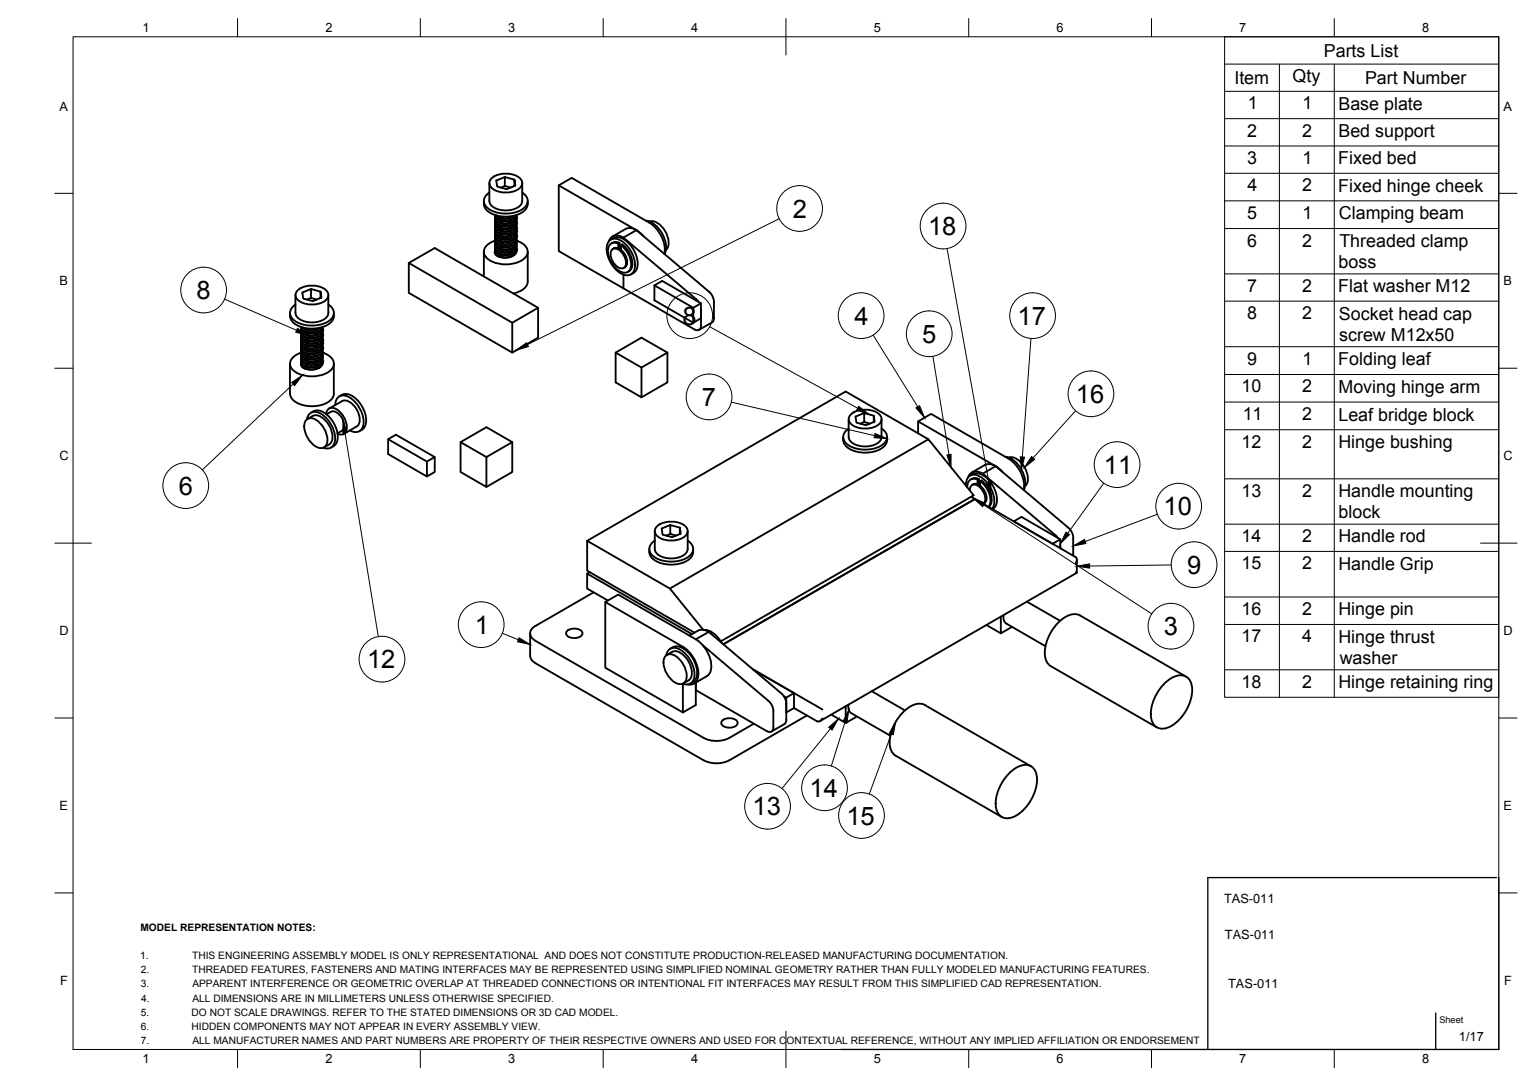
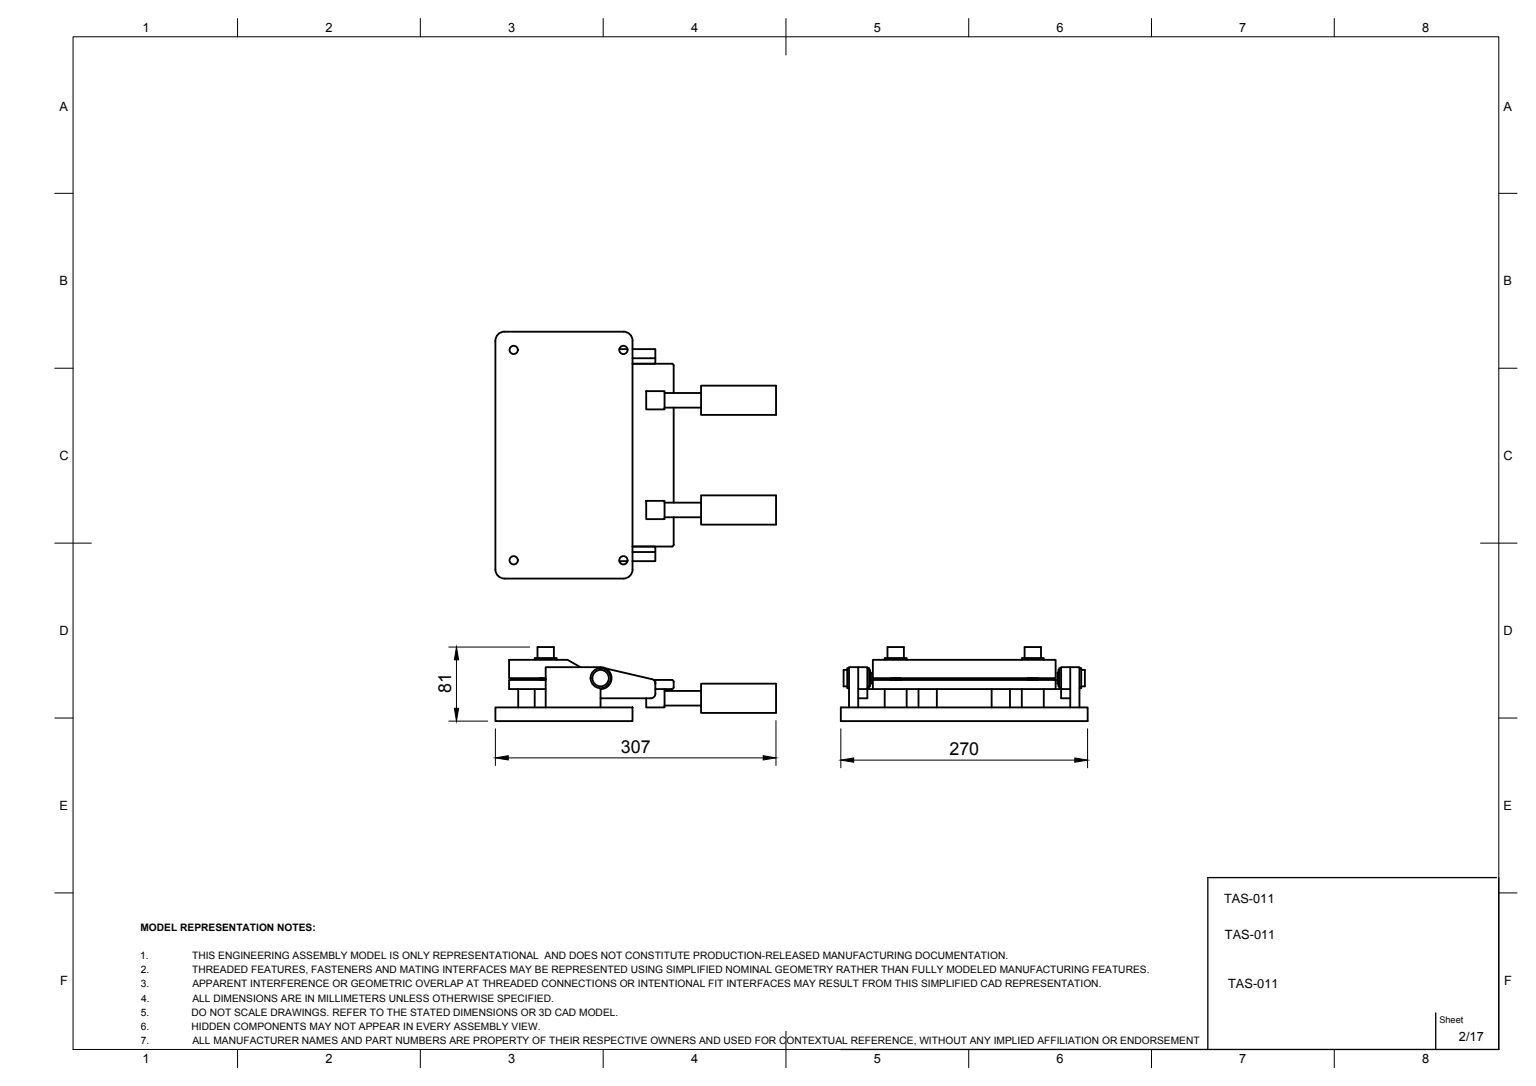
ISO-10303-21;
HEADER;
/* Generated by software containing ST-Developer
 * from STEP Tools, Inc. (www.steptools.com) 
 */

FILE_DESCRIPTION(
/* description */ (
'Independent manual bench leaf bending machine,200mm work width. Fabri
cated welded frame and folding leaf, repeated bushed and fully retaine
d hinge hardware, two handles with bonded grips, beveled clamping beam
 and modeledM12 clamp screws.2mm omitted-workpiece assembly reference 
gap, not a capacity claim. Native135deg hinge travel. Weld sizing, pro
duction fits, material condition, bending capacity, strength and life 
unassigned.'),
/* implementation_level */ '2;1');

FILE_NAME(
/* name */ 'TAS-011.step',
/* time_stamp */ '2026-11-14T09:11:34-08:00',
/* author */ (''),
/* organization */ (''),
/* preprocessor_version */ 'ST-DEVELOPER v20.2',
/* originating_system */ 'Autodesk Translation Framework v15.17.0.0',
/* authorisation */ '');

FILE_SCHEMA (('AUTOMOTIVE_DESIGN { 1 0 10303 214 3 1 1 }'));
ENDSEC;

DATA;
#10=MECHANICAL_DESIGN_GEOMETRIC_PRESENTATION_REPRESENTATION('',(#446,#447,
#448,#449,#450,#451,#452,#453,#454,#455,#456,#457,#458,#459,#460,#461,#462,
#463),#37701);
#11=ITEM_DEFINED_TRANSFORMATION($,$,#4362,#4673);
#12=ITEM_DEFINED_TRANSFORMATION($,$,#4434,#4674);
#13=ITEM_DEFINED_TRANSFORMATION($,$,#4393,#4675);
#14=ITEM_DEFINED_TRANSFORMATION($,$,#4441,#4676);
#15=ITEM_DEFINED_TRANSFORMATION($,$,#4406,#4677);
#16=ITEM_DEFINED_TRANSFORMATION($,$,#4454,#4678);
#17=ITEM_DEFINED_TRANSFORMATION($,$,#4488,#4679);
#18=ITEM_DEFINED_TRANSFORMATION($,$,#4497,#4680);
#19=ITEM_DEFINED_TRANSFORMATION($,$,#4419,#4681);
#20=ITEM_DEFINED_TRANSFORMATION($,$,#4577,#4682);
#21=ITEM_DEFINED_TRANSFORMATION($,$,#4596,#4683);
#22=ITEM_DEFINED_TRANSFORMATION($,$,#4603,#4684);
#23=ITEM_DEFINED_TRANSFORMATION($,$,#4612,#4685);
#24=ITEM_DEFINED_TRANSFORMATION($,$,#4619,#4686);
#25=ITEM_DEFINED_TRANSFORMATION($,$,#4625,#4687);
#26=ITEM_DEFINED_TRANSFORMATION($,$,#4635,#4688);
#27=ITEM_DEFINED_TRANSFORMATION($,$,#4653,#4689);
#28=ITEM_DEFINED_TRANSFORMATION($,$,#4662,#4690);
#29=ITEM_DEFINED_TRANSFORMATION($,$,#4434,#4691);
#30=ITEM_DEFINED_TRANSFORMATION($,$,#4441,#4692);
#31=ITEM_DEFINED_TRANSFORMATION($,$,#4454,#4693);
#32=ITEM_DEFINED_TRANSFORMATION($,$,#4488,#4694);
#33=ITEM_DEFINED_TRANSFORMATION($,$,#4497,#4695);
#34=ITEM_DEFINED_TRANSFORMATION($,$,#4577,#4696);
#35=ITEM_DEFINED_TRANSFORMATION($,$,#4596,#4697);
#36=ITEM_DEFINED_TRANSFORMATION($,$,#4603,#4698);
#37=ITEM_DEFINED_TRANSFORMATION($,$,#4612,#4699);
#38=ITEM_DEFINED_TRANSFORMATION($,$,#4619,#4700);
#39=ITEM_DEFINED_TRANSFORMATION($,$,#4625,#4701);
#40=ITEM_DEFINED_TRANSFORMATION($,$,#4653,#4702);
#41=ITEM_DEFINED_TRANSFORMATION($,$,#4635,#4703);
#42=ITEM_DEFINED_TRANSFORMATION($,$,#4653,#4704);
#43=ITEM_DEFINED_TRANSFORMATION($,$,#4653,#4705);
#44=ITEM_DEFINED_TRANSFORMATION($,$,#4662,#4706);
#45=(
REPRESENTATION_RELATIONSHIP($,$,#37779,#37778)
REPRESENTATION_RELATIONSHIP_WITH_TRANSFORMATION(#11)
SHAPE_REPRESENTATION_RELATIONSHIP()
);
#46=(
REPRESENTATION_RELATIONSHIP($,$,#37783,#37778)
REPRESENTATION_RELATIONSHIP_WITH_TRANSFORMATION(#12)
SHAPE_REPRESENTATION_RELATIONSHIP()
);
#47=(
REPRESENTATION_RELATIONSHIP($,$,#37780,#37778)
REPRESENTATION_RELATIONSHIP_WITH_TRANSFORMATION(#13)
SHAPE_REPRESENTATION_RELATIONSHIP()
);
#48=(
REPRESENTATION_RELATIONSHIP($,$,#37784,#37778)
REPRESENTATION_RELATIONSHIP_WITH_TRANSFORMATION(#14)
SHAPE_REPRESENTATION_RELATIONSHIP()
);
#49=(
REPRESENTATION_RELATIONSHIP($,$,#37781,#37778)
REPRESENTATION_RELATIONSHIP_WITH_TRANSFORMATION(#15)
SHAPE_REPRESENTATION_RELATIONSHIP()
);
#50=(
REPRESENTATION_RELATIONSHIP($,$,#37785,#37778)
REPRESENTATION_RELATIONSHIP_WITH_TRANSFORMATION(#16)
SHAPE_REPRESENTATION_RELATIONSHIP()
);
#51=(
REPRESENTATION_RELATIONSHIP($,$,#37786,#37778)
REPRESENTATION_RELATIONSHIP_WITH_TRANSFORMATION(#17)
SHAPE_REPRESENTATION_RELATIONSHIP()
);
#52=(
REPRESENTATION_RELATIONSHIP($,$,#37787,#37778)
REPRESENTATION_RELATIONSHIP_WITH_TRANSFORMATION(#18)
SHAPE_REPRESENTATION_RELATIONSHIP()
);
#53=(
REPRESENTATION_RELATIONSHIP($,$,#37782,#37778)
REPRESENTATION_RELATIONSHIP_WITH_TRANSFORMATION(#19)
SHAPE_REPRESENTATION_RELATIONSHIP()
);
#54=(
REPRESENTATION_RELATIONSHIP($,$,#37788,#37778)
REPRESENTATION_RELATIONSHIP_WITH_TRANSFORMATION(#20)
SHAPE_REPRESENTATION_RELATIONSHIP()
);
#55=(
REPRESENTATION_RELATIONSHIP($,$,#37789,#37778)
REPRESENTATION_RELATIONSHIP_WITH_TRANSFORMATION(#21)
SHAPE_REPRESENTATION_RELATIONSHIP()
);
#56=(
REPRESENTATION_RELATIONSHIP($,$,#37790,#37778)
REPRESENTATION_RELATIONSHIP_WITH_TRANSFORMATION(#22)
SHAPE_REPRESENTATION_RELATIONSHIP()
);
#57=(
REPRESENTATION_RELATIONSHIP($,$,#37791,#37778)
REPRESENTATION_RELATIONSHIP_WITH_TRANSFORMATION(#23)
SHAPE_REPRESENTATION_RELATIONSHIP()
);
#58=(
REPRESENTATION_RELATIONSHIP($,$,#37792,#37778)
REPRESENTATION_RELATIONSHIP_WITH_TRANSFORMATION(#24)
SHAPE_REPRESENTATION_RELATIONSHIP()
);
#59=(
REPRESENTATION_RELATIONSHIP($,$,#37793,#37778)
REPRESENTATION_RELATIONSHIP_WITH_TRANSFORMATION(#25)
SHAPE_REPRESENTATION_RELATIONSHIP()
);
#60=(
REPRESENTATION_RELATIONSHIP($,$,#37794,#37778)
REPRESENTATION_RELATIONSHIP_WITH_TRANSFORMATION(#26)
SHAPE_REPRESENTATION_RELATIONSHIP()
);
#61=(
REPRESENTATION_RELATIONSHIP($,$,#37795,#37778)
REPRESENTATION_RELATIONSHIP_WITH_TRANSFORMATION(#27)
SHAPE_REPRESENTATION_RELATIONSHIP()
);
#62=(
REPRESENTATION_RELATIONSHIP($,$,#37796,#37778)
REPRESENTATION_RELATIONSHIP_WITH_TRANSFORMATION(#28)
SHAPE_REPRESENTATION_RELATIONSHIP()
);
#63=(
REPRESENTATION_RELATIONSHIP($,$,#37783,#37778)
REPRESENTATION_RELATIONSHIP_WITH_TRANSFORMATION(#29)
SHAPE_REPRESENTATION_RELATIONSHIP()
);
#64=(
REPRESENTATION_RELATIONSHIP($,$,#37784,#37778)
REPRESENTATION_RELATIONSHIP_WITH_TRANSFORMATION(#30)
SHAPE_REPRESENTATION_RELATIONSHIP()
);
#65=(
REPRESENTATION_RELATIONSHIP($,$,#37785,#37778)
REPRESENTATION_RELATIONSHIP_WITH_TRANSFORMATION(#31)
SHAPE_REPRESENTATION_RELATIONSHIP()
);
#66=(
REPRESENTATION_RELATIONSHIP($,$,#37786,#37778)
REPRESENTATION_RELATIONSHIP_WITH_TRANSFORMATION(#32)
SHAPE_REPRESENTATION_RELATIONSHIP()
);
#67=(
REPRESENTATION_RELATIONSHIP($,$,#37787,#37778)
REPRESENTATION_RELATIONSHIP_WITH_TRANSFORMATION(#33)
SHAPE_REPRESENTATION_RELATIONSHIP()
);
#68=(
REPRESENTATION_RELATIONSHIP($,$,#37788,#37778)
REPRESENTATION_RELATIONSHIP_WITH_TRANSFORMATION(#34)
SHAPE_REPRESENTATION_RELATIONSHIP()
);
#69=(
REPRESENTATION_RELATIONSHIP($,$,#37789,#37778)
REPRESENTATION_RELATIONSHIP_WITH_TRANSFORMATION(#35)
SHAPE_REPRESENTATION_RELATIONSHIP()
);
#70=(
REPRESENTATION_RELATIONSHIP($,$,#37790,#37778)
REPRESENTATION_RELATIONSHIP_WITH_TRANSFORMATION(#36)
SHAPE_REPRESENTATION_RELATIONSHIP()
);
#71=(
REPRESENTATION_RELATIONSHIP($,$,#37791,#37778)
REPRESENTATION_RELATIONSHIP_WITH_TRANSFORMATION(#37)
SHAPE_REPRESENTATION_RELATIONSHIP()
);
#72=(
REPRESENTATION_RELATIONSHIP($,$,#37792,#37778)
REPRESENTATION_RELATIONSHIP_WITH_TRANSFORMATION(#38)
SHAPE_REPRESENTATION_RELATIONSHIP()
);
#73=(
REPRESENTATION_RELATIONSHIP($,$,#37793,#37778)
REPRESENTATION_RELATIONSHIP_WITH_TRANSFORMATION(#39)
SHAPE_REPRESENTATION_RELATIONSHIP()
);
#74=(
REPRESENTATION_RELATIONSHIP($,$,#37795,#37778)
REPRESENTATION_RELATIONSHIP_WITH_TRANSFORMATION(#40)
SHAPE_REPRESENTATION_RELATIONSHIP()
);
#75=(
REPRESENTATION_RELATIONSHIP($,$,#37794,#37778)
REPRESENTATION_RELATIONSHIP_WITH_TRANSFORMATION(#41)
SHAPE_REPRESENTATION_RELATIONSHIP()
);
#76=(
REPRESENTATION_RELATIONSHIP($,$,#37795,#37778)
REPRESENTATION_RELATIONSHIP_WITH_TRANSFORMATION(#42)
SHAPE_REPRESENTATION_RELATIONSHIP()
);
#77=(
REPRESENTATION_RELATIONSHIP($,$,#37795,#37778)
REPRESENTATION_RELATIONSHIP_WITH_TRANSFORMATION(#43)
SHAPE_REPRESENTATION_RELATIONSHIP()
);
#78=(
REPRESENTATION_RELATIONSHIP($,$,#37796,#37778)
REPRESENTATION_RELATIONSHIP_WITH_TRANSFORMATION(#44)
SHAPE_REPRESENTATION_RELATIONSHIP()
);
#79=CONTEXT_DEPENDENT_SHAPE_REPRESENTATION(#45,#37744);
#80=CONTEXT_DEPENDENT_SHAPE_REPRESENTATION(#46,#37745);
#81=CONTEXT_DEPENDENT_SHAPE_REPRESENTATION(#47,#37746);
#82=CONTEXT_DEPENDENT_SHAPE_REPRESENTATION(#48,#37747);
#83=CONTEXT_DEPENDENT_SHAPE_REPRESENTATION(#49,#37748);
#84=CONTEXT_DEPENDENT_SHAPE_REPRESENTATION(#50,#37749);
#85=CONTEXT_DEPENDENT_SHAPE_REPRESENTATION(#51,#37750);
#86=CONTEXT_DEPENDENT_SHAPE_REPRESENTATION(#52,#37751);
#87=CONTEXT_DEPENDENT_SHAPE_REPRESENTATION(#53,#37752);
#88=CONTEXT_DEPENDENT_SHAPE_REPRESENTATION(#54,#37753);
#89=CONTEXT_DEPENDENT_SHAPE_REPRESENTATION(#55,#37754);
#90=CONTEXT_DEPENDENT_SHAPE_REPRESENTATION(#56,#37755);
#91=CONTEXT_DEPENDENT_SHAPE_REPRESENTATION(#57,#37756);
#92=CONTEXT_DEPENDENT_SHAPE_REPRESENTATION(#58,#37757);
#93=CONTEXT_DEPENDENT_SHAPE_REPRESENTATION(#59,#37758);
#94=CONTEXT_DEPENDENT_SHAPE_REPRESENTATION(#60,#37759);
#95=CONTEXT_DEPENDENT_SHAPE_REPRESENTATION(#61,#37760);
#96=CONTEXT_DEPENDENT_SHAPE_REPRESENTATION(#62,#37761);
#97=CONTEXT_DEPENDENT_SHAPE_REPRESENTATION(#63,#37762);
#98=CONTEXT_DEPENDENT_SHAPE_REPRESENTATION(#64,#37763);
#99=CONTEXT_DEPENDENT_SHAPE_REPRESENTATION(#65,#37764);
#100=CONTEXT_DEPENDENT_SHAPE_REPRESENTATION(#66,#37765);
#101=CONTEXT_DEPENDENT_SHAPE_REPRESENTATION(#67,#37766);
#102=CONTEXT_DEPENDENT_SHAPE_REPRESENTATION(#68,#37767);
#103=CONTEXT_DEPENDENT_SHAPE_REPRESENTATION(#69,#37768);
#104=CONTEXT_DEPENDENT_SHAPE_REPRESENTATION(#70,#37769);
#105=CONTEXT_DEPENDENT_SHAPE_REPRESENTATION(#71,#37770);
#106=CONTEXT_DEPENDENT_SHAPE_REPRESENTATION(#72,#37771);
#107=CONTEXT_DEPENDENT_SHAPE_REPRESENTATION(#73,#37772);
#108=CONTEXT_DEPENDENT_SHAPE_REPRESENTATION(#74,#37773);
#109=CONTEXT_DEPENDENT_SHAPE_REPRESENTATION(#75,#37774);
#110=CONTEXT_DEPENDENT_SHAPE_REPRESENTATION(#76,#37775);
#111=CONTEXT_DEPENDENT_SHAPE_REPRESENTATION(#77,#37776);
#112=CONTEXT_DEPENDENT_SHAPE_REPRESENTATION(#78,#37777);
#113=NEXT_ASSEMBLY_USAGE_OCCURRENCE('Base plate:1','Base plate:1',
'Base plate:1',#37798,#37799,'Base plate:1');
#114=NEXT_ASSEMBLY_USAGE_OCCURRENCE('Bed support:1','Bed support:1',
'Bed support:1',#37798,#37803,'Bed support:1');
#115=NEXT_ASSEMBLY_USAGE_OCCURRENCE('Fixed bed:1','Fixed bed:1',
'Fixed bed:1',#37798,#37800,'Fixed bed:1');
#116=NEXT_ASSEMBLY_USAGE_OCCURRENCE('Fixed hinge cheek:1',
'Fixed hinge cheek:1','Fixed hinge cheek:1',#37798,#37804,
'Fixed hinge cheek:1');
#117=NEXT_ASSEMBLY_USAGE_OCCURRENCE('Clamping beam:1','Clamping beam:1',
'Clamping beam:1',#37798,#37801,'Clamping beam:1');
#118=NEXT_ASSEMBLY_USAGE_OCCURRENCE('Threaded clamp boss:1',
'Threaded clamp boss:1','Threaded clamp boss:1',#37798,#37805,
'Threaded clamp boss:1');
#119=NEXT_ASSEMBLY_USAGE_OCCURRENCE('Flat washer M12:1',
'Flat washer M12:1','Flat washer M12:1',#37798,#37806,
'Flat washer M12:1');
#120=NEXT_ASSEMBLY_USAGE_OCCURRENCE('Socket head cap screw M12x50:1',
'Socket head cap screw M12x50:1','Socket head cap screw M12x50:1',#37798,
#37807,'Socket head cap screw M12x50:1');
#121=NEXT_ASSEMBLY_USAGE_OCCURRENCE('Folding leaf:1','Folding leaf:1',
'Folding leaf:1',#37798,#37802,'Folding leaf:1');
#122=NEXT_ASSEMBLY_USAGE_OCCURRENCE('Moving hinge arm:1',
'Moving hinge arm:1','Moving hinge arm:1',#37798,#37808,
'Moving hinge arm:1');
#123=NEXT_ASSEMBLY_USAGE_OCCURRENCE('Leaf bridge block:1',
'Leaf bridge block:1','Leaf bridge block:1',#37798,#37809,
'Leaf bridge block:1');
#124=NEXT_ASSEMBLY_USAGE_OCCURRENCE('Hinge bushing:1','Hinge bushing:1',
'Hinge bushing:1',#37798,#37810,'Hinge bushing:1');
#125=NEXT_ASSEMBLY_USAGE_OCCURRENCE('Handle mounting block:1',
'Handle mounting block:1','Handle mounting block:1',#37798,#37811,
'Handle mounting block:1');
#126=NEXT_ASSEMBLY_USAGE_OCCURRENCE('Handle rod:1','Handle rod:1',
'Handle rod:1',#37798,#37812,'Handle rod:1');
#127=NEXT_ASSEMBLY_USAGE_OCCURRENCE('Handle grip:1','Handle grip:1',
'Handle grip:1',#37798,#37813,'Handle grip:1');
#128=NEXT_ASSEMBLY_USAGE_OCCURRENCE('Hinge pin:1','Hinge pin:1',
'Hinge pin:1',#37798,#37814,'Hinge pin:1');
#129=NEXT_ASSEMBLY_USAGE_OCCURRENCE('Hinge thrust washer:1',
'Hinge thrust washer:1','Hinge thrust washer:1',#37798,#37815,
'Hinge thrust washer:1');
#130=NEXT_ASSEMBLY_USAGE_OCCURRENCE('Hinge retaining ring:1',
'Hinge retaining ring:1','Hinge retaining ring:1',#37798,#37816,
'Hinge retaining ring:1');
#131=NEXT_ASSEMBLY_USAGE_OCCURRENCE('Bed support:2','Bed support:2',
'Bed support:2',#37798,#37803,'Bed support:2');
#132=NEXT_ASSEMBLY_USAGE_OCCURRENCE('Fixed hinge cheek:2',
'Fixed hinge cheek:2','Fixed hinge cheek:2',#37798,#37804,
'Fixed hinge cheek:2');
#133=NEXT_ASSEMBLY_USAGE_OCCURRENCE('Threaded clamp boss:2',
'Threaded clamp boss:2','Threaded clamp boss:2',#37798,#37805,
'Threaded clamp boss:2');
#134=NEXT_ASSEMBLY_USAGE_OCCURRENCE('Flat washer M12:2',
'Flat washer M12:2','Flat washer M12:2',#37798,#37806,
'Flat washer M12:2');
#135=NEXT_ASSEMBLY_USAGE_OCCURRENCE('Socket head cap screw M12x50:2',
'Socket head cap screw M12x50:2','Socket head cap screw M12x50:2',#37798,
#37807,'Socket head cap screw M12x50:2');
#136=NEXT_ASSEMBLY_USAGE_OCCURRENCE('Moving hinge arm:2',
'Moving hinge arm:2','Moving hinge arm:2',#37798,#37808,
'Moving hinge arm:2');
#137=NEXT_ASSEMBLY_USAGE_OCCURRENCE('Leaf bridge block:2',
'Leaf bridge block:2','Leaf bridge block:2',#37798,#37809,
'Leaf bridge block:2');
#138=NEXT_ASSEMBLY_USAGE_OCCURRENCE('Hinge bushing:2','Hinge bushing:2',
'Hinge bushing:2',#37798,#37810,'Hinge bushing:2');
#139=NEXT_ASSEMBLY_USAGE_OCCURRENCE('Handle mounting block:2',
'Handle mounting block:2','Handle mounting block:2',#37798,#37811,
'Handle mounting block:2');
#140=NEXT_ASSEMBLY_USAGE_OCCURRENCE('Handle rod:2','Handle rod:2',
'Handle rod:2',#37798,#37812,'Handle rod:2');
#141=NEXT_ASSEMBLY_USAGE_OCCURRENCE('Handle grip:2','Handle grip:2',
'Handle grip:2',#37798,#37813,'Handle grip:2');
#142=NEXT_ASSEMBLY_USAGE_OCCURRENCE('Hinge thrust washer:2',
'Hinge thrust washer:2','Hinge thrust washer:2',#37798,#37815,
'Hinge thrust washer:2');
#143=NEXT_ASSEMBLY_USAGE_OCCURRENCE('Hinge pin:2','Hinge pin:2',
'Hinge pin:2',#37798,#37814,'Hinge pin:2');
#144=NEXT_ASSEMBLY_USAGE_OCCURRENCE('Hinge thrust washer:3',
'Hinge thrust washer:3','Hinge thrust washer:3',#37798,#37815,
'Hinge thrust washer:3');
#145=NEXT_ASSEMBLY_USAGE_OCCURRENCE('Hinge thrust washer:4',
'Hinge thrust washer:4','Hinge thrust washer:4',#37798,#37815,
'Hinge thrust washer:4');
#146=NEXT_ASSEMBLY_USAGE_OCCURRENCE('Hinge retaining ring:2',
'Hinge retaining ring:2','Hinge retaining ring:2',#37798,#37816,
'Hinge retaining ring:2');
#147=CONICAL_SURFACE('',#4560,5.5,0.78539816339745);
#148=B_SPLINE_SURFACE_WITH_KNOTS('',3,3,((#12501,#12502,#12503,#12504,#12505,
#12506,#12507,#12508,#12509,#12510,#12511,#12512,#12513,#12514,#12515,#12516,
#12517,#12518,#12519,#12520,#12521,#12522,#12523,#12524,#12525,#12526,#12527,
#12528,#12529,#12530,#12531,#12532,#12533,#12534,#12535,#12536,#12537,#12538,
#12539,#12540,#12541,#12542,#12543,#12544,#12545,#12546,#12547,#12548,#12549,
#12550,#12551,#12552,#12553,#12554,#12555,#12556,#12557,#12558,#12559,#12560,
#12561,#12562,#12563,#12564,#12565,#12566,#12567,#12568,#12569,#12570,#12571,
#12572,#12573,#12574,#12575,#12576,#12577,#12578,#12579,#12580,#12581,#12582,
#12583,#12584,#12585,#12586,#12587,#12588,#12589,#12590,#12591,#12592,#12593,
#12594,#12595,#12596,#12597,#12598,#12599,#12600,#12601,#12602,#12603,#12604,
#12605,#12606,#12607,#12608,#12609,#12610,#12611,#12612,#12613,#12614,#12615,
#12616,#12617,#12618,#12619,#12620,#12621,#12622,#12623,#12624,#12625,#12626,
#12627,#12628,#12629,#12630,#12631,#12632,#12633,#12634,#12635,#12636,#12637,
#12638,#12639,#12640,#12641,#12642,#12643,#12644,#12645,#12646,#12647,#12648,
#12649,#12650,#12651),(#12652,#12653,#12654,#12655,#12656,#12657,#12658,
#12659,#12660,#12661,#12662,#12663,#12664,#12665,#12666,#12667,#12668,#12669,
#12670,#12671,#12672,#12673,#12674,#12675,#12676,#12677,#12678,#12679,#12680,
#12681,#12682,#12683,#12684,#12685,#12686,#12687,#12688,#12689,#12690,#12691,
#12692,#12693,#12694,#12695,#12696,#12697,#12698,#12699,#12700,#12701,#12702,
#12703,#12704,#12705,#12706,#12707,#12708,#12709,#12710,#12711,#12712,#12713,
#12714,#12715,#12716,#12717,#12718,#12719,#12720,#12721,#12722,#12723,#12724,
#12725,#12726,#12727,#12728,#12729,#12730,#12731,#12732,#12733,#12734,#12735,
#12736,#12737,#12738,#12739,#12740,#12741,#12742,#12743,#12744,#12745,#12746,
#12747,#12748,#12749,#12750,#12751,#12752,#12753,#12754,#12755,#12756,#12757,
#12758,#12759,#12760,#12761,#12762,#12763,#12764,#12765,#12766,#12767,#12768,
#12769,#12770,#12771,#12772,#12773,#12774,#12775,#12776,#12777,#12778,#12779,
#12780,#12781,#12782,#12783,#12784,#12785,#12786,#12787,#12788,#12789,#12790,
#12791,#12792,#12793,#12794,#12795,#12796,#12797,#12798,#12799,#12800,#12801,
#12802),(#12803,#12804,#12805,#12806,#12807,#12808,#12809,#12810,#12811,
#12812,#12813,#12814,#12815,#12816,#12817,#12818,#12819,#12820,#12821,#12822,
#12823,#12824,#12825,#12826,#12827,#12828,#12829,#12830,#12831,#12832,#12833,
#12834,#12835,#12836,#12837,#12838,#12839,#12840,#12841,#12842,#12843,#12844,
#12845,#12846,#12847,#12848,#12849,#12850,#12851,#12852,#12853,#12854,#12855,
#12856,#12857,#12858,#12859,#12860,#12861,#12862,#12863,#12864,#12865,#12866,
#12867,#12868,#12869,#12870,#12871,#12872,#12873,#12874,#12875,#12876,#12877,
#12878,#12879,#12880,#12881,#12882,#12883,#12884,#12885,#12886,#12887,#12888,
#12889,#12890,#12891,#12892,#12893,#12894,#12895,#12896,#12897,#12898,#12899,
#12900,#12901,#12902,#12903,#12904,#12905,#12906,#12907,#12908,#12909,#12910,
#12911,#12912,#12913,#12914,#12915,#12916,#12917,#12918,#12919,#12920,#12921,
#12922,#12923,#12924,#12925,#12926,#12927,#12928,#12929,#12930,#12931,#12932,
#12933,#12934,#12935,#12936,#12937,#12938,#12939,#12940,#12941,#12942,#12943,
#12944,#12945,#12946,#12947,#12948,#12949,#12950,#12951,#12952,#12953),
(#12954,#12955,#12956,#12957,#12958,#12959,#12960,#12961,#12962,#12963,
#12964,#12965,#12966,#12967,#12968,#12969,#12970,#12971,#12972,#12973,#12974,
#12975,#12976,#12977,#12978,#12979,#12980,#12981,#12982,#12983,#12984,#12985,
#12986,#12987,#12988,#12989,#12990,#12991,#12992,#12993,#12994,#12995,#12996,
#12997,#12998,#12999,#13000,#13001,#13002,#13003,#13004,#13005,#13006,#13007,
#13008,#13009,#13010,#13011,#13012,#13013,#13014,#13015,#13016,#13017,#13018,
#13019,#13020,#13021,#13022,#13023,#13024,#13025,#13026,#13027,#13028,#13029,
#13030,#13031,#13032,#13033,#13034,#13035,#13036,#13037,#13038,#13039,#13040,
#13041,#13042,#13043,#13044,#13045,#13046,#13047,#13048,#13049,#13050,#13051,
#13052,#13053,#13054,#13055,#13056,#13057,#13058,#13059,#13060,#13061,#13062,
#13063,#13064,#13065,#13066,#13067,#13068,#13069,#13070,#13071,#13072,#13073,
#13074,#13075,#13076,#13077,#13078,#13079,#13080,#13081,#13082,#13083,#13084,
#13085,#13086,#13087,#13088,#13089,#13090,#13091,#13092,#13093,#13094,#13095,
#13096,#13097,#13098,#13099,#13100,#13101,#13102,#13103,#13104)),
 .UNSPECIFIED.,.F.,.F.,.F.,(4,4),(4,1,1,1,1,1,1,1,1,1,1,1,1,1,1,1,1,1,1,
1,1,1,1,1,1,1,1,1,1,1,1,1,1,1,1,1,1,1,1,1,1,1,1,1,1,1,1,1,1,1,1,1,1,1,1,
1,1,1,1,1,1,1,1,1,1,1,1,1,1,1,1,1,1,1,1,1,1,1,1,1,1,1,1,1,1,1,1,1,1,1,1,
1,1,1,1,1,1,1,1,1,1,1,1,1,1,1,1,1,1,1,1,1,1,1,1,1,1,1,1,1,1,1,1,1,1,1,1,
1,1,1,1,1,1,1,1,1,1,1,1,1,1,1,1,1,1,1,1,1,4),(-6.2431789936198E-5,0.112802168308183),
(11.8516712330609,12.3505987470977,12.8494638293446,13.3483289115915,13.8471939938383,
14.3460590760852,14.8449241583321,15.343789240579,15.8426543228258,16.3415194050727,
16.8403844873196,17.3392495695665,17.8381146518133,18.3369797340602,18.8358448163071,
19.334709898554,19.8335749808009,20.3324400630477,20.8313051452946,21.3301702275415,
21.8290353097884,22.3279003920352,22.8267654742821,23.325630556529,23.8244956387759,
24.3233607210227,24.8222258032696,25.3210908855165,25.8199559677634,26.3188210500103,
26.8176861322571,27.316551214504,27.8154162967509,28.3142813789978,28.8131464612446,
29.3120115434915,29.8108766257384,30.3097417079853,30.8086067902321,31.307471872479,
31.8063369547259,32.3052020369728,32.8040671192197,33.3029322014665,33.8017972837134,
34.3006623659603,34.7995274482072,35.298392530454,35.7972576127009,36.2961226949478,
36.7949877771947,37.2938528594415,37.7927179416884,38.2915830239353,38.7904481061822,
39.2893131884291,39.7881782706759,40.2870433529228,40.7859084351697,41.2847735174166,
41.7836385996634,42.2825036819103,42.7813687641572,43.2802338464041,43.779098928651,
44.2779640108978,44.7768290931447,45.2756941753916,45.7745592576385,46.2734243398853,
46.7722894221322,47.2711545043791,47.770019586626,48.2688846688728,48.7677497511197,
49.2666148333666,49.7654799156135,50.2643449978603,50.7632100801072,51.2620751623541,
51.760940244601,52.2598053268479,52.7586704090947,53.2575354913416,53.7564005735885,
54.2552656558354,54.7541307380822,55.2529958203291,55.751860902576,56.2507259848229,
56.7495910670697,57.2484561493166,57.7473212315635,58.2461863138104,58.7450513960573,
59.2439164783041,59.742781560551,60.2416466427979,60.7405117250448,61.2393768072916,
61.7382418895385,62.2371069717854,62.7359720540323,63.2348371362792,63.733702218526,
64.2325673007729,64.7314323830198,65.2302974652667,65.7291625475135,66.2280276297604,
66.7268927120073,67.2257577942542,67.724622876501,68.2234879587479,68.7223530409948,
69.2212181232417,69.7200832054885,70.2189482877354,70.7178133699823,71.2166784522292,
71.7155435344761,72.2144086167229,72.7132736989698,73.2121387812167,73.7110038634636,
74.2098689457104,74.7087340279573,75.2075991102042,75.7064641924511,76.205329274698,
76.7041943569448,77.2030594391917,77.7019245214386,78.2007896036855,78.6996546859323,
79.1985197681792,79.6973848504261,80.196249932673,80.6951150149198,81.1939800971667,
81.6928451794136,82.1917102616605,82.6905753439074,83.1894404261542,83.6883055084011,
84.187170590648,84.6860356728949,85.1849007551417,85.6837658373886),
 .UNSPECIFIED.);
#149=B_SPLINE_SURFACE_WITH_KNOTS('',3,3,((#13322,#13323,#13324,#13325,#13326,
#13327,#13328,#13329,#13330,#13331,#13332,#13333,#13334,#13335,#13336,#13337,
#13338,#13339,#13340,#13341,#13342,#13343,#13344,#13345,#13346,#13347,#13348,
#13349,#13350,#13351,#13352,#13353,#13354,#13355,#13356,#13357,#13358,#13359,
#13360,#13361,#13362,#13363,#13364,#13365,#13366,#13367,#13368,#13369,#13370,
#13371,#13372,#13373,#13374,#13375,#13376,#13377,#13378,#13379,#13380,#13381,
#13382,#13383,#13384,#13385,#13386,#13387,#13388,#13389,#13390,#13391,#13392,
#13393,#13394,#13395,#13396,#13397,#13398,#13399,#13400,#13401,#13402,#13403,
#13404,#13405,#13406,#13407,#13408,#13409,#13410,#13411,#13412,#13413,#13414,
#13415,#13416,#13417,#13418,#13419,#13420,#13421,#13422,#13423,#13424,#13425,
#13426,#13427,#13428,#13429,#13430,#13431,#13432,#13433,#13434,#13435,#13436,
#13437,#13438,#13439,#13440,#13441,#13442,#13443,#13444,#13445,#13446,#13447,
#13448,#13449,#13450,#13451,#13452,#13453,#13454,#13455,#13456,#13457,#13458,
#13459,#13460,#13461,#13462,#13463,#13464,#13465,#13466,#13467,#13468,#13469,
#13470,#13471,#13472),(#13473,#13474,#13475,#13476,#13477,#13478,#13479,
#13480,#13481,#13482,#13483,#13484,#13485,#13486,#13487,#13488,#13489,#13490,
#13491,#13492,#13493,#13494,#13495,#13496,#13497,#13498,#13499,#13500,#13501,
#13502,#13503,#13504,#13505,#13506,#13507,#13508,#13509,#13510,#13511,#13512,
#13513,#13514,#13515,#13516,#13517,#13518,#13519,#13520,#13521,#13522,#13523,
#13524,#13525,#13526,#13527,#13528,#13529,#13530,#13531,#13532,#13533,#13534,
#13535,#13536,#13537,#13538,#13539,#13540,#13541,#13542,#13543,#13544,#13545,
#13546,#13547,#13548,#13549,#13550,#13551,#13552,#13553,#13554,#13555,#13556,
#13557,#13558,#13559,#13560,#13561,#13562,#13563,#13564,#13565,#13566,#13567,
#13568,#13569,#13570,#13571,#13572,#13573,#13574,#13575,#13576,#13577,#13578,
#13579,#13580,#13581,#13582,#13583,#13584,#13585,#13586,#13587,#13588,#13589,
#13590,#13591,#13592,#13593,#13594,#13595,#13596,#13597,#13598,#13599,#13600,
#13601,#13602,#13603,#13604,#13605,#13606,#13607,#13608,#13609,#13610,#13611,
#13612,#13613,#13614,#13615,#13616,#13617,#13618,#13619,#13620,#13621,#13622,
#13623),(#13624,#13625,#13626,#13627,#13628,#13629,#13630,#13631,#13632,
#13633,#13634,#13635,#13636,#13637,#13638,#13639,#13640,#13641,#13642,#13643,
#13644,#13645,#13646,#13647,#13648,#13649,#13650,#13651,#13652,#13653,#13654,
#13655,#13656,#13657,#13658,#13659,#13660,#13661,#13662,#13663,#13664,#13665,
#13666,#13667,#13668,#13669,#13670,#13671,#13672,#13673,#13674,#13675,#13676,
#13677,#13678,#13679,#13680,#13681,#13682,#13683,#13684,#13685,#13686,#13687,
#13688,#13689,#13690,#13691,#13692,#13693,#13694,#13695,#13696,#13697,#13698,
#13699,#13700,#13701,#13702,#13703,#13704,#13705,#13706,#13707,#13708,#13709,
#13710,#13711,#13712,#13713,#13714,#13715,#13716,#13717,#13718,#13719,#13720,
#13721,#13722,#13723,#13724,#13725,#13726,#13727,#13728,#13729,#13730,#13731,
#13732,#13733,#13734,#13735,#13736,#13737,#13738,#13739,#13740,#13741,#13742,
#13743,#13744,#13745,#13746,#13747,#13748,#13749,#13750,#13751,#13752,#13753,
#13754,#13755,#13756,#13757,#13758,#13759,#13760,#13761,#13762,#13763,#13764,
#13765,#13766,#13767,#13768,#13769,#13770,#13771,#13772,#13773,#13774),
(#13775,#13776,#13777,#13778,#13779,#13780,#13781,#13782,#13783,#13784,
#13785,#13786,#13787,#13788,#13789,#13790,#13791,#13792,#13793,#13794,#13795,
#13796,#13797,#13798,#13799,#13800,#13801,#13802,#13803,#13804,#13805,#13806,
#13807,#13808,#13809,#13810,#13811,#13812,#13813,#13814,#13815,#13816,#13817,
#13818,#13819,#13820,#13821,#13822,#13823,#13824,#13825,#13826,#13827,#13828,
#13829,#13830,#13831,#13832,#13833,#13834,#13835,#13836,#13837,#13838,#13839,
#13840,#13841,#13842,#13843,#13844,#13845,#13846,#13847,#13848,#13849,#13850,
#13851,#13852,#13853,#13854,#13855,#13856,#13857,#13858,#13859,#13860,#13861,
#13862,#13863,#13864,#13865,#13866,#13867,#13868,#13869,#13870,#13871,#13872,
#13873,#13874,#13875,#13876,#13877,#13878,#13879,#13880,#13881,#13882,#13883,
#13884,#13885,#13886,#13887,#13888,#13889,#13890,#13891,#13892,#13893,#13894,
#13895,#13896,#13897,#13898,#13899,#13900,#13901,#13902,#13903,#13904,#13905,
#13906,#13907,#13908,#13909,#13910,#13911,#13912,#13913,#13914,#13915,#13916,
#13917,#13918,#13919,#13920,#13921,#13922,#13923,#13924,#13925)),
 .UNSPECIFIED.,.F.,.F.,.F.,(4,4),(4,1,1,1,1,1,1,1,1,1,1,1,1,1,1,1,1,1,1,
1,1,1,1,1,1,1,1,1,1,1,1,1,1,1,1,1,1,1,1,1,1,1,1,1,1,1,1,1,1,1,1,1,1,1,1,
1,1,1,1,1,1,1,1,1,1,1,1,1,1,1,1,1,1,1,1,1,1,1,1,1,1,1,1,1,1,1,1,1,1,1,1,
1,1,1,1,1,1,1,1,1,1,1,1,1,1,1,1,1,1,1,1,1,1,1,1,1,1,1,1,1,1,1,1,1,1,1,1,
1,1,1,1,1,1,1,1,1,1,1,1,1,1,1,1,1,1,1,1,1,4),(-4.55374339698837E-5,0.1128189478572),
(14.3984001269718,14.8972652092187,15.3961302914656,15.8949953737124,16.3938604559593,
16.8927255382062,17.3915906204531,17.8904557026999,18.3893207849468,18.8881858671937,
19.3870509494406,19.8859160316874,20.3847811139343,20.8836461961812,21.3825112784281,
21.881376360675,22.3802414429218,22.8791065251687,23.3779716074156,23.8768366896625,
24.3757017719093,24.8745668541562,25.3734319364031,25.87229701865,26.3711621008968,
26.8700271831437,27.3688922653906,27.8677573476375,28.3666224298844,28.8654875121312,
29.3643525943781,29.863217676625,30.3620827588719,30.8609478411187,31.3598129233656,
31.8586780056125,32.3575430878594,32.8564081701062,33.3552732523531,33.8541383346,
34.3530034168469,34.8518684990938,35.3507335813406,35.8495986635875,36.3484637458344,
36.8473288280813,37.3461939103281,37.845058992575,38.3439240748219,38.8427891570688,
39.3416542393157,39.8405193215625,40.3393844038094,40.8382494860563,41.3371145683032,
41.83597965055,42.3348447327969,42.8337098150438,43.3325748972907,43.8314399795375,
44.3303050617844,44.8291701440313,45.3280352262782,45.8269003085251,46.3257653907719,
46.8246304730188,47.3234955552657,47.8223606375126,48.3212257197594,48.8200908020063,
49.3189558842532,49.8178209665001,50.316686048747,50.8155511309938,51.3144162132407,
51.8132812954876,52.3121463777345,52.8110114599813,53.3098765422282,53.8087416244751,
54.307606706722,54.8064717889688,55.3053368712157,55.8042019534626,56.3030670357095,
56.8019321179564,57.3007972002032,57.7996622824501,58.298527364697,58.7973924469439,
59.2962575291907,59.7951226114376,60.2939876936845,60.7928527759314,61.2917178581782,
61.7905829404251,62.289448022672,62.7883131049189,63.2871781871658,63.7860432694126,
64.2849083516595,64.7837734339064,65.2826385161533,65.7815035984001,66.280368680647,
66.7792337628939,67.2780988451408,67.7769639273876,68.2758290096345,68.7746940918814,
69.2735591741283,69.7724242563752,70.271289338622,70.7701544208689,71.2690195031158,
71.7678845853627,72.2667496676095,72.7656147498564,73.2644798321033,73.7633449143502,
74.2622099965971,74.7610750788439,75.2599401610908,75.7588052433377,76.2576703255846,
76.7565354078314,77.2554004900783,77.7542655723252,78.2531306545721,78.7519957368189,
79.2508608190658,79.7497259013127,80.2485909835596,80.7474560658064,81.2463211480533,
81.7451862303002,82.2440513125471,82.742916394794,83.2417814770408,83.7406465592877,
84.2395116415346,84.7383767237815,85.2372418060283,85.7361068882752,86.2349719705221,
86.733837052769,87.2327021350158,87.7315672172627,88.2304947397941),
 .UNSPECIFIED.);
#150=B_SPLINE_SURFACE_WITH_KNOTS('',3,3,((#34220,#34221,#34222,#34223,#34224,
#34225,#34226,#34227,#34228,#34229,#34230,#34231,#34232,#34233,#34234,#34235,
#34236,#34237,#34238,#34239,#34240,#34241,#34242,#34243,#34244,#34245,#34246,
#34247,#34248,#34249,#34250,#34251,#34252,#34253,#34254,#34255,#34256,#34257,
#34258,#34259,#34260,#34261,#34262,#34263,#34264,#34265,#34266,#34267,#34268,
#34269,#34270,#34271,#34272,#34273,#34274,#34275,#34276,#34277,#34278,#34279,
#34280,#34281,#34282,#34283,#34284,#34285,#34286,#34287,#34288,#34289,#34290,
#34291,#34292,#34293,#34294,#34295,#34296,#34297,#34298,#34299,#34300,#34301,
#34302,#34303,#34304,#34305,#34306,#34307,#34308,#34309,#34310,#34311,#34312,
#34313,#34314,#34315,#34316,#34317,#34318,#34319,#34320,#34321,#34322,#34323,
#34324,#34325,#34326,#34327,#34328,#34329,#34330,#34331,#34332,#34333,#34334,
#34335,#34336,#34337,#34338,#34339,#34340,#34341,#34342,#34343,#34344,#34345,
#34346,#34347,#34348,#34349,#34350,#34351,#34352,#34353,#34354,#34355,#34356,
#34357,#34358,#34359,#34360,#34361,#34362,#34363,#34364,#34365,#34366,#34367,
#34368,#34369,#34370,#34371,#34372,#34373,#34374,#34375,#34376,#34377,#34378,
#34379,#34380,#34381,#34382,#34383,#34384,#34385,#34386,#34387,#34388,#34389,
#34390,#34391,#34392,#34393,#34394,#34395,#34396,#34397,#34398,#34399,#34400,
#34401,#34402,#34403,#34404,#34405,#34406,#34407,#34408,#34409,#34410,#34411,
#34412,#34413,#34414,#34415,#34416,#34417,#34418,#34419,#34420,#34421,#34422,
#34423,#34424,#34425,#34426,#34427,#34428,#34429,#34430,#34431,#34432,#34433,
#34434,#34435,#34436,#34437,#34438,#34439,#34440,#34441,#34442,#34443,#34444,
#34445,#34446,#34447,#34448,#34449,#34450,#34451,#34452,#34453,#34454,#34455,
#34456,#34457,#34458,#34459,#34460,#34461,#34462,#34463,#34464,#34465,#34466,
#34467,#34468,#34469,#34470,#34471,#34472,#34473,#34474,#34475,#34476,#34477,
#34478,#34479,#34480,#34481,#34482,#34483,#34484,#34485,#34486,#34487,#34488,
#34489,#34490,#34491,#34492,#34493,#34494,#34495,#34496,#34497,#34498,#34499,
#34500,#34501,#34502,#34503,#34504,#34505,#34506,#34507,#34508,#34509,#34510,
#34511,#34512,#34513,#34514,#34515,#34516,#34517,#34518,#34519,#34520,#34521,
#34522,#34523,#34524,#34525,#34526,#34527,#34528,#34529,#34530,#34531,#34532,
#34533,#34534,#34535,#34536,#34537,#34538,#34539,#34540,#34541,#34542,#34543,
#34544,#34545,#34546,#34547,#34548,#34549,#34550,#34551,#34552,#34553,#34554,
#34555,#34556,#34557,#34558,#34559,#34560,#34561,#34562,#34563,#34564,#34565,
#34566,#34567,#34568,#34569,#34570,#34571,#34572,#34573,#34574,#34575,#34576,
#34577,#34578,#34579,#34580,#34581,#34582),(#34583,#34584,#34585,#34586,
#34587,#34588,#34589,#34590,#34591,#34592,#34593,#34594,#34595,#34596,#34597,
#34598,#34599,#34600,#34601,#34602,#34603,#34604,#34605,#34606,#34607,#34608,
#34609,#34610,#34611,#34612,#34613,#34614,#34615,#34616,#34617,#34618,#34619,
#34620,#34621,#34622,#34623,#34624,#34625,#34626,#34627,#34628,#34629,#34630,
#34631,#34632,#34633,#34634,#34635,#34636,#34637,#34638,#34639,#34640,#34641,
#34642,#34643,#34644,#34645,#34646,#34647,#34648,#34649,#34650,#34651,#34652,
#34653,#34654,#34655,#34656,#34657,#34658,#34659,#34660,#34661,#34662,#34663,
#34664,#34665,#34666,#34667,#34668,#34669,#34670,#34671,#34672,#34673,#34674,
#34675,#34676,#34677,#34678,#34679,#34680,#34681,#34682,#34683,#34684,#34685,
#34686,#34687,#34688,#34689,#34690,#34691,#34692,#34693,#34694,#34695,#34696,
#34697,#34698,#34699,#34700,#34701,#34702,#34703,#34704,#34705,#34706,#34707,
#34708,#34709,#34710,#34711,#34712,#34713,#34714,#34715,#34716,#34717,#34718,
#34719,#34720,#34721,#34722,#34723,#34724,#34725,#34726,#34727,#34728,#34729,
#34730,#34731,#34732,#34733,#34734,#34735,#34736,#34737,#34738,#34739,#34740,
#34741,#34742,#34743,#34744,#34745,#34746,#34747,#34748,#34749,#34750,#34751,
#34752,#34753,#34754,#34755,#34756,#34757,#34758,#34759,#34760,#34761,#34762,
#34763,#34764,#34765,#34766,#34767,#34768,#34769,#34770,#34771,#34772,#34773,
#34774,#34775,#34776,#34777,#34778,#34779,#34780,#34781,#34782,#34783,#34784,
#34785,#34786,#34787,#34788,#34789,#34790,#34791,#34792,#34793,#34794,#34795,
#34796,#34797,#34798,#34799,#34800,#34801,#34802,#34803,#34804,#34805,#34806,
#34807,#34808,#34809,#34810,#34811,#34812,#34813,#34814,#34815,#34816,#34817,
#34818,#34819,#34820,#34821,#34822,#34823,#34824,#34825,#34826,#34827,#34828,
#34829,#34830,#34831,#34832,#34833,#34834,#34835,#34836,#34837,#34838,#34839,
#34840,#34841,#34842,#34843,#34844,#34845,#34846,#34847,#34848,#34849,#34850,
#34851,#34852,#34853,#34854,#34855,#34856,#34857,#34858,#34859,#34860,#34861,
#34862,#34863,#34864,#34865,#34866,#34867,#34868,#34869,#34870,#34871,#34872,
#34873,#34874,#34875,#34876,#34877,#34878,#34879,#34880,#34881,#34882,#34883,
#34884,#34885,#34886,#34887,#34888,#34889,#34890,#34891,#34892,#34893,#34894,
#34895,#34896,#34897,#34898,#34899,#34900,#34901,#34902,#34903,#34904,#34905,
#34906,#34907,#34908,#34909,#34910,#34911,#34912,#34913,#34914,#34915,#34916,
#34917,#34918,#34919,#34920,#34921,#34922,#34923,#34924,#34925,#34926,#34927,
#34928,#34929,#34930,#34931,#34932,#34933,#34934,#34935,#34936,#34937,#34938,
#34939,#34940,#34941,#34942,#34943,#34944,#34945),(#34946,#34947,#34948,
#34949,#34950,#34951,#34952,#34953,#34954,#34955,#34956,#34957,#34958,#34959,
#34960,#34961,#34962,#34963,#34964,#34965,#34966,#34967,#34968,#34969,#34970,
#34971,#34972,#34973,#34974,#34975,#34976,#34977,#34978,#34979,#34980,#34981,
#34982,#34983,#34984,#34985,#34986,#34987,#34988,#34989,#34990,#34991,#34992,
#34993,#34994,#34995,#34996,#34997,#34998,#34999,#35000,#35001,#35002,#35003,
#35004,#35005,#35006,#35007,#35008,#35009,#35010,#35011,#35012,#35013,#35014,
#35015,#35016,#35017,#35018,#35019,#35020,#35021,#35022,#35023,#35024,#35025,
#35026,#35027,#35028,#35029,#35030,#35031,#35032,#35033,#35034,#35035,#35036,
#35037,#35038,#35039,#35040,#35041,#35042,#35043,#35044,#35045,#35046,#35047,
#35048,#35049,#35050,#35051,#35052,#35053,#35054,#35055,#35056,#35057,#35058,
#35059,#35060,#35061,#35062,#35063,#35064,#35065,#35066,#35067,#35068,#35069,
#35070,#35071,#35072,#35073,#35074,#35075,#35076,#35077,#35078,#35079,#35080,
#35081,#35082,#35083,#35084,#35085,#35086,#35087,#35088,#35089,#35090,#35091,
#35092,#35093,#35094,#35095,#35096,#35097,#35098,#35099,#35100,#35101,#35102,
#35103,#35104,#35105,#35106,#35107,#35108,#35109,#35110,#35111,#35112,#35113,
#35114,#35115,#35116,#35117,#35118,#35119,#35120,#35121,#35122,#35123,#35124,
#35125,#35126,#35127,#35128,#35129,#35130,#35131,#35132,#35133,#35134,#35135,
#35136,#35137,#35138,#35139,#35140,#35141,#35142,#35143,#35144,#35145,#35146,
#35147,#35148,#35149,#35150,#35151,#35152,#35153,#35154,#35155,#35156,#35157,
#35158,#35159,#35160,#35161,#35162,#35163,#35164,#35165,#35166,#35167,#35168,
#35169,#35170,#35171,#35172,#35173,#35174,#35175,#35176,#35177,#35178,#35179,
#35180,#35181,#35182,#35183,#35184,#35185,#35186,#35187,#35188,#35189,#35190,
#35191,#35192,#35193,#35194,#35195,#35196,#35197,#35198,#35199,#35200,#35201,
#35202,#35203,#35204,#35205,#35206,#35207,#35208,#35209,#35210,#35211,#35212,
#35213,#35214,#35215,#35216,#35217,#35218,#35219,#35220,#35221,#35222,#35223,
#35224,#35225,#35226,#35227,#35228,#35229,#35230,#35231,#35232,#35233,#35234,
#35235,#35236,#35237,#35238,#35239,#35240,#35241,#35242,#35243,#35244,#35245,
#35246,#35247,#35248,#35249,#35250,#35251,#35252,#35253,#35254,#35255,#35256,
#35257,#35258,#35259,#35260,#35261,#35262,#35263,#35264,#35265,#35266,#35267,
#35268,#35269,#35270,#35271,#35272,#35273,#35274,#35275,#35276,#35277,#35278,
#35279,#35280,#35281,#35282,#35283,#35284,#35285,#35286,#35287,#35288,#35289,
#35290,#35291,#35292,#35293,#35294,#35295,#35296,#35297,#35298,#35299,#35300,
#35301,#35302,#35303,#35304,#35305,#35306,#35307,#35308),(#35309,#35310,
#35311,#35312,#35313,#35314,#35315,#35316,#35317,#35318,#35319,#35320,#35321,
#35322,#35323,#35324,#35325,#35326,#35327,#35328,#35329,#35330,#35331,#35332,
#35333,#35334,#35335,#35336,#35337,#35338,#35339,#35340,#35341,#35342,#35343,
#35344,#35345,#35346,#35347,#35348,#35349,#35350,#35351,#35352,#35353,#35354,
#35355,#35356,#35357,#35358,#35359,#35360,#35361,#35362,#35363,#35364,#35365,
#35366,#35367,#35368,#35369,#35370,#35371,#35372,#35373,#35374,#35375,#35376,
#35377,#35378,#35379,#35380,#35381,#35382,#35383,#35384,#35385,#35386,#35387,
#35388,#35389,#35390,#35391,#35392,#35393,#35394,#35395,#35396,#35397,#35398,
#35399,#35400,#35401,#35402,#35403,#35404,#35405,#35406,#35407,#35408,#35409,
#35410,#35411,#35412,#35413,#35414,#35415,#35416,#35417,#35418,#35419,#35420,
#35421,#35422,#35423,#35424,#35425,#35426,#35427,#35428,#35429,#35430,#35431,
#35432,#35433,#35434,#35435,#35436,#35437,#35438,#35439,#35440,#35441,#35442,
#35443,#35444,#35445,#35446,#35447,#35448,#35449,#35450,#35451,#35452,#35453,
#35454,#35455,#35456,#35457,#35458,#35459,#35460,#35461,#35462,#35463,#35464,
#35465,#35466,#35467,#35468,#35469,#35470,#35471,#35472,#35473,#35474,#35475,
#35476,#35477,#35478,#35479,#35480,#35481,#35482,#35483,#35484,#35485,#35486,
#35487,#35488,#35489,#35490,#35491,#35492,#35493,#35494,#35495,#35496,#35497,
#35498,#35499,#35500,#35501,#35502,#35503,#35504,#35505,#35506,#35507,#35508,
#35509,#35510,#35511,#35512,#35513,#35514,#35515,#35516,#35517,#35518,#35519,
#35520,#35521,#35522,#35523,#35524,#35525,#35526,#35527,#35528,#35529,#35530,
#35531,#35532,#35533,#35534,#35535,#35536,#35537,#35538,#35539,#35540,#35541,
#35542,#35543,#35544,#35545,#35546,#35547,#35548,#35549,#35550,#35551,#35552,
#35553,#35554,#35555,#35556,#35557,#35558,#35559,#35560,#35561,#35562,#35563,
#35564,#35565,#35566,#35567,#35568,#35569,#35570,#35571,#35572,#35573,#35574,
#35575,#35576,#35577,#35578,#35579,#35580,#35581,#35582,#35583,#35584,#35585,
#35586,#35587,#35588,#35589,#35590,#35591,#35592,#35593,#35594,#35595,#35596,
#35597,#35598,#35599,#35600,#35601,#35602,#35603,#35604,#35605,#35606,#35607,
#35608,#35609,#35610,#35611,#35612,#35613,#35614,#35615,#35616,#35617,#35618,
#35619,#35620,#35621,#35622,#35623,#35624,#35625,#35626,#35627,#35628,#35629,
#35630,#35631,#35632,#35633,#35634,#35635,#35636,#35637,#35638,#35639,#35640,
#35641,#35642,#35643,#35644,#35645,#35646,#35647,#35648,#35649,#35650,#35651,
#35652,#35653,#35654,#35655,#35656,#35657,#35658,#35659,#35660,#35661,#35662,
#35663,#35664,#35665,#35666,#35667,#35668,#35669,#35670,#35671)),
 .UNSPECIFIED.,.F.,.F.,.F.,(4,4),(4,1,1,1,1,1,1,1,1,1,1,1,1,1,1,1,1,1,1,
1,1,1,1,1,1,1,1,1,1,1,1,1,1,1,1,1,1,1,1,1,1,1,1,1,1,1,1,1,1,1,1,1,1,1,1,
1,1,1,1,1,1,1,1,1,1,1,1,1,1,1,1,1,1,1,1,1,1,1,1,1,1,1,1,1,1,1,1,1,1,1,1,
1,1,1,1,1,1,1,1,1,1,1,1,1,1,1,1,1,1,1,1,1,1,1,1,1,1,1,1,1,1,1,1,1,1,1,1,
1,1,1,1,1,1,1,1,1,1,1,1,1,1,1,1,1,1,1,1,1,1,1,1,1,1,1,1,1,1,1,1,1,1,1,1,
1,1,1,1,1,1,1,1,1,1,1,1,1,1,1,1,1,1,1,1,1,1,1,1,1,1,1,1,1,1,1,1,1,1,1,1,
1,1,1,1,1,1,1,1,1,1,1,1,1,1,1,1,1,1,1,1,1,1,1,1,1,1,1,1,1,1,1,1,1,1,1,1,
1,1,1,1,1,1,1,1,1,1,1,1,1,1,1,1,1,1,1,1,1,1,1,1,1,1,1,1,1,1,1,1,1,1,1,1,
1,1,1,1,1,1,1,1,1,1,1,1,1,1,1,1,1,1,1,1,1,1,1,1,1,1,1,1,1,1,1,1,1,1,1,1,
1,1,1,1,1,1,1,1,1,1,1,1,1,1,1,1,1,1,1,1,1,1,1,1,1,1,1,1,1,1,1,1,1,1,1,1,
1,1,1,1,1,1,1,1,1,1,1,1,1,1,1,1,1,4),(-4.46121474024446E-5,0.115356621383595),
(11.6153617464843,12.1145577438013,12.6136939684918,13.1128301931823,13.6119664178728,
14.1111026425634,14.6102388672539,15.1093750919444,15.608511316635,16.1076475413255,
16.606783766016,17.1059199907065,17.6050562153971,18.1041924400876,18.6033286647781,
19.1024648894686,19.6016011141592,20.1007373388497,20.5998735635402,21.0990097882307,
21.5981460129213,22.0972822376118,22.5964184623023,23.0955546869928,23.5946909116834,
24.0938271363739,24.5929633610644,25.092099585755,25.5912358104455,26.090372035136,
26.5895082598265,27.0886444845171,27.5877807092076,28.0869169338981,28.5860531585886,
29.0851893832792,29.5843256079697,30.0834618326602,30.5825980573507,31.0817342820413,
31.5808705067318,32.0800067314223,32.5791429561128,33.0782791808034,33.5774154054939,
34.0765516301844,34.575687854875,35.0748240795655,35.573960304256,36.0730965289465,
36.5722327536371,37.0713689783276,37.5705052030181,38.0696414277086,38.5687776523992,
39.0679138770897,39.5670501017802,40.0661863264707,40.5653225511613,41.0644587758518,
41.5635950005423,42.0627312252329,42.5618674499234,43.0610036746139,43.5601398993044,
44.059276123995,44.5584123486855,45.057548573376,45.5566847980665,46.0558210227571,
46.5549572474476,47.0540934721381,47.5532296968286,48.0523659215192,48.5515021462097,
49.0506383709002,49.5497745955907,50.0489108202813,50.5480470449718,51.0471832696623,
51.5463194943529,52.0454557190434,52.5445919437339,53.0437281684244,53.542864393115,
54.0420006178055,54.541136842496,55.0402730671865,55.5394092918771,56.0385455165676,
56.5376817412581,57.0368179659486,57.5359541906392,58.0350904153297,58.5342266400202,
59.0333628647107,59.5324990894013,60.0316353140918,60.5307715387823,61.0299077634728,
61.5290439881634,62.0281802128539,62.5273164375444,63.026452662235,63.5255888869255,
64.024725111616,64.5238613363065,65.0229975609971,65.5221337856876,66.0212700103781,
66.5204062350686,67.0195424597592,67.5186786844497,68.0178149091402,68.5169511338307,
69.0160873585213,69.5152235832118,70.0143598079023,70.5134960325929,71.0126322572834,
71.5117684819739,72.0109047066644,72.510040931355,73.0091771560455,73.508313380736,
74.0074496054265,74.5065858301171,75.0057220548076,75.5048582794981,76.0039945041887,
76.5031307288792,77.0022669535697,77.5014031782602,78.0005394029507,78.4996756276413,
78.9988118523318,79.4979480770223,79.9970843017128,80.4962205264034,80.9953567510939,
81.4944929757844,81.993629200475,82.4927654251655,82.991901649856,83.4910378745465,
83.9901740992371,84.4893103239276,84.9884465486181,85.4875827733086,85.9867189979992,
86.4858552226897,86.9849914473802,87.4841276720708,87.9832638967613,88.4824001214518,
88.9815363461423,89.4806725708329,89.9798087955234,90.4789450202139,90.9780812449044,
91.477217469595,91.9763536942855,92.475489918976,92.9746261436665,93.4737623683571,
93.9728985930476,94.4720348177381,94.9711710424286,95.4703072671192,95.9694434918097,
96.4685797165002,96.9677159411908,97.4668521658813,97.9659883905718,98.4651246152623,
98.9642608399529,99.4633970646434,99.9625332893339,100.461669514024,100.960805738715,
101.459941963405,101.959078188096,102.458214412787,102.957350637477,103.456486862168,
103.955623086858,104.454759311549,104.953895536239,105.45303176093,105.95216798562,
106.451304210311,106.950440435001,107.449576659692,107.948712884382,108.447849109073,
108.946985333763,109.446121558454,109.945257783144,110.444394007835,110.943530232525,
111.442666457216,111.941802681907,112.440938906597,112.940075131288,113.439211355978,
113.938347580669,114.437483805359,114.93662003005,115.43575625474,115.934892479431,
116.434028704121,116.933164928812,117.432301153502,117.931437378193,118.430573602883,
118.929709827574,119.428846052264,119.927982276955,120.427118501645,120.926254726336,
121.425390951027,121.924527175717,122.423663400408,122.922799625098,123.421935849789,
123.921072074479,124.42020829917,124.91934452386,125.418480748551,125.917616973241,
126.416753197932,126.915889422622,127.415025647313,127.914161872003,128.413298096694,
128.912434321384,129.411570546075,129.910706770766,130.409842995456,130.908979220147,
131.408115444837,131.907251669528,132.406387894218,132.905524118909,133.404660343599,
133.90379656829,134.40293279298,134.902069017671,135.401205242361,135.900341467052,
136.399477691742,136.898613916433,137.397750141123,137.896886365814,138.396022590504,
138.895158815195,139.394295039885,139.893431264576,140.392567489267,140.891703713957,
141.390839938648,141.889976163338,142.389112388029,142.888248612719,143.38738483741,
143.8865210621,144.385657286791,144.884793511481,145.383929736172,145.883065960862,
146.382202185553,146.881338410243,147.380474634934,147.879610859624,148.378747084315,
148.877883309006,149.377019533696,149.876155758387,150.375291983077,150.874428207768,
151.373564432458,151.872700657149,152.371836881839,152.87097310653,153.37010933122,
153.869245555911,154.368381780601,154.867518005292,155.366654229982,155.865790454673,
156.364926679363,156.864062904054,157.363199128744,157.862335353435,158.361471578126,
158.860607802816,159.359744027507,159.858880252197,160.358016476888,160.857152701578,
161.356288926269,161.855425150959,162.35456137565,162.85369760034,163.352833825031,
163.851970049721,164.351106274412,164.850242499102,165.349378723793,165.848514948483,
166.347651173174,166.846787397864,167.345923622555,167.845059847246,168.344196071936,
168.843332296627,169.342468521317,169.841604746008,170.340740970698,170.839877195389,
171.339013420079,171.83814964477,172.33728586946,172.836422094151,173.335558318841,
173.834694543532,174.333830768222,174.832966992913,175.332103217603,175.831239442294,
176.330375666984,176.829511891675,177.328648116366,177.827784341056,178.326920565747,
178.826056790437,179.325193015128,179.824329239818,180.323465464509,180.822601689199,
181.32173791389,181.82087413858,182.320010363271,182.819146587961,183.318282812652,
183.817419037342,184.316555262033,184.815691486723,185.314827711414,185.813963936104,
186.313100160795,186.812236385486,187.311372610176,187.810508834867,188.309645059557,
188.808781284248,189.307917508938,189.807053733629,190.306189958319,190.80532618301,
191.3044624077),.UNSPECIFIED.);
#151=B_SPLINE_SURFACE_WITH_KNOTS('',3,3,((#35779,#35780,#35781,#35782,#35783,
#35784,#35785,#35786,#35787,#35788,#35789,#35790,#35791,#35792,#35793,#35794,
#35795,#35796,#35797,#35798,#35799,#35800,#35801,#35802,#35803,#35804,#35805,
#35806,#35807,#35808,#35809,#35810,#35811,#35812,#35813,#35814,#35815,#35816,
#35817,#35818,#35819,#35820,#35821,#35822,#35823,#35824,#35825,#35826,#35827,
#35828,#35829,#35830,#35831,#35832,#35833,#35834,#35835,#35836,#35837,#35838,
#35839,#35840,#35841,#35842,#35843,#35844,#35845,#35846,#35847,#35848,#35849,
#35850,#35851,#35852,#35853,#35854,#35855,#35856,#35857,#35858,#35859,#35860,
#35861,#35862,#35863,#35864,#35865,#35866,#35867,#35868,#35869,#35870,#35871,
#35872,#35873,#35874,#35875,#35876,#35877,#35878,#35879,#35880,#35881,#35882,
#35883,#35884,#35885,#35886,#35887,#35888,#35889,#35890,#35891,#35892,#35893,
#35894,#35895,#35896,#35897,#35898,#35899,#35900,#35901,#35902,#35903,#35904,
#35905,#35906,#35907,#35908,#35909,#35910,#35911,#35912,#35913,#35914,#35915,
#35916,#35917,#35918,#35919,#35920,#35921,#35922,#35923,#35924,#35925,#35926,
#35927,#35928,#35929,#35930,#35931,#35932,#35933,#35934,#35935,#35936,#35937,
#35938,#35939,#35940,#35941,#35942,#35943,#35944,#35945,#35946,#35947,#35948,
#35949,#35950,#35951,#35952,#35953,#35954,#35955,#35956,#35957,#35958,#35959,
#35960,#35961,#35962,#35963,#35964,#35965,#35966,#35967,#35968,#35969,#35970,
#35971,#35972,#35973,#35974,#35975,#35976,#35977,#35978,#35979,#35980,#35981,
#35982,#35983,#35984,#35985,#35986,#35987,#35988,#35989,#35990,#35991,#35992,
#35993,#35994,#35995,#35996,#35997,#35998,#35999,#36000,#36001,#36002,#36003,
#36004,#36005,#36006,#36007,#36008,#36009,#36010,#36011,#36012,#36013,#36014,
#36015,#36016,#36017,#36018,#36019,#36020,#36021,#36022,#36023,#36024,#36025,
#36026,#36027,#36028,#36029,#36030,#36031,#36032,#36033,#36034,#36035,#36036,
#36037,#36038,#36039,#36040,#36041,#36042,#36043,#36044,#36045,#36046,#36047,
#36048,#36049,#36050,#36051,#36052,#36053,#36054,#36055,#36056,#36057,#36058,
#36059,#36060,#36061,#36062,#36063,#36064,#36065,#36066,#36067,#36068,#36069,
#36070,#36071,#36072,#36073,#36074,#36075,#36076,#36077,#36078,#36079,#36080,
#36081,#36082,#36083,#36084,#36085,#36086,#36087,#36088,#36089,#36090,#36091,
#36092,#36093,#36094,#36095,#36096,#36097,#36098,#36099,#36100,#36101,#36102,
#36103,#36104,#36105,#36106,#36107,#36108,#36109,#36110,#36111,#36112,#36113,
#36114,#36115,#36116,#36117,#36118,#36119,#36120,#36121,#36122,#36123,#36124,
#36125,#36126,#36127,#36128,#36129,#36130,#36131,#36132,#36133,#36134,#36135,
#36136,#36137,#36138,#36139,#36140,#36141,#36142,#36143,#36144,#36145),
(#36146,#36147,#36148,#36149,#36150,#36151,#36152,#36153,#36154,#36155,
#36156,#36157,#36158,#36159,#36160,#36161,#36162,#36163,#36164,#36165,#36166,
#36167,#36168,#36169,#36170,#36171,#36172,#36173,#36174,#36175,#36176,#36177,
#36178,#36179,#36180,#36181,#36182,#36183,#36184,#36185,#36186,#36187,#36188,
#36189,#36190,#36191,#36192,#36193,#36194,#36195,#36196,#36197,#36198,#36199,
#36200,#36201,#36202,#36203,#36204,#36205,#36206,#36207,#36208,#36209,#36210,
#36211,#36212,#36213,#36214,#36215,#36216,#36217,#36218,#36219,#36220,#36221,
#36222,#36223,#36224,#36225,#36226,#36227,#36228,#36229,#36230,#36231,#36232,
#36233,#36234,#36235,#36236,#36237,#36238,#36239,#36240,#36241,#36242,#36243,
#36244,#36245,#36246,#36247,#36248,#36249,#36250,#36251,#36252,#36253,#36254,
#36255,#36256,#36257,#36258,#36259,#36260,#36261,#36262,#36263,#36264,#36265,
#36266,#36267,#36268,#36269,#36270,#36271,#36272,#36273,#36274,#36275,#36276,
#36277,#36278,#36279,#36280,#36281,#36282,#36283,#36284,#36285,#36286,#36287,
#36288,#36289,#36290,#36291,#36292,#36293,#36294,#36295,#36296,#36297,#36298,
#36299,#36300,#36301,#36302,#36303,#36304,#36305,#36306,#36307,#36308,#36309,
#36310,#36311,#36312,#36313,#36314,#36315,#36316,#36317,#36318,#36319,#36320,
#36321,#36322,#36323,#36324,#36325,#36326,#36327,#36328,#36329,#36330,#36331,
#36332,#36333,#36334,#36335,#36336,#36337,#36338,#36339,#36340,#36341,#36342,
#36343,#36344,#36345,#36346,#36347,#36348,#36349,#36350,#36351,#36352,#36353,
#36354,#36355,#36356,#36357,#36358,#36359,#36360,#36361,#36362,#36363,#36364,
#36365,#36366,#36367,#36368,#36369,#36370,#36371,#36372,#36373,#36374,#36375,
#36376,#36377,#36378,#36379,#36380,#36381,#36382,#36383,#36384,#36385,#36386,
#36387,#36388,#36389,#36390,#36391,#36392,#36393,#36394,#36395,#36396,#36397,
#36398,#36399,#36400,#36401,#36402,#36403,#36404,#36405,#36406,#36407,#36408,
#36409,#36410,#36411,#36412,#36413,#36414,#36415,#36416,#36417,#36418,#36419,
#36420,#36421,#36422,#36423,#36424,#36425,#36426,#36427,#36428,#36429,#36430,
#36431,#36432,#36433,#36434,#36435,#36436,#36437,#36438,#36439,#36440,#36441,
#36442,#36443,#36444,#36445,#36446,#36447,#36448,#36449,#36450,#36451,#36452,
#36453,#36454,#36455,#36456,#36457,#36458,#36459,#36460,#36461,#36462,#36463,
#36464,#36465,#36466,#36467,#36468,#36469,#36470,#36471,#36472,#36473,#36474,
#36475,#36476,#36477,#36478,#36479,#36480,#36481,#36482,#36483,#36484,#36485,
#36486,#36487,#36488,#36489,#36490,#36491,#36492,#36493,#36494,#36495,#36496,
#36497,#36498,#36499,#36500,#36501,#36502,#36503,#36504,#36505,#36506,#36507,
#36508,#36509,#36510,#36511,#36512),(#36513,#36514,#36515,#36516,#36517,
#36518,#36519,#36520,#36521,#36522,#36523,#36524,#36525,#36526,#36527,#36528,
#36529,#36530,#36531,#36532,#36533,#36534,#36535,#36536,#36537,#36538,#36539,
#36540,#36541,#36542,#36543,#36544,#36545,#36546,#36547,#36548,#36549,#36550,
#36551,#36552,#36553,#36554,#36555,#36556,#36557,#36558,#36559,#36560,#36561,
#36562,#36563,#36564,#36565,#36566,#36567,#36568,#36569,#36570,#36571,#36572,
#36573,#36574,#36575,#36576,#36577,#36578,#36579,#36580,#36581,#36582,#36583,
#36584,#36585,#36586,#36587,#36588,#36589,#36590,#36591,#36592,#36593,#36594,
#36595,#36596,#36597,#36598,#36599,#36600,#36601,#36602,#36603,#36604,#36605,
#36606,#36607,#36608,#36609,#36610,#36611,#36612,#36613,#36614,#36615,#36616,
#36617,#36618,#36619,#36620,#36621,#36622,#36623,#36624,#36625,#36626,#36627,
#36628,#36629,#36630,#36631,#36632,#36633,#36634,#36635,#36636,#36637,#36638,
#36639,#36640,#36641,#36642,#36643,#36644,#36645,#36646,#36647,#36648,#36649,
#36650,#36651,#36652,#36653,#36654,#36655,#36656,#36657,#36658,#36659,#36660,
#36661,#36662,#36663,#36664,#36665,#36666,#36667,#36668,#36669,#36670,#36671,
#36672,#36673,#36674,#36675,#36676,#36677,#36678,#36679,#36680,#36681,#36682,
#36683,#36684,#36685,#36686,#36687,#36688,#36689,#36690,#36691,#36692,#36693,
#36694,#36695,#36696,#36697,#36698,#36699,#36700,#36701,#36702,#36703,#36704,
#36705,#36706,#36707,#36708,#36709,#36710,#36711,#36712,#36713,#36714,#36715,
#36716,#36717,#36718,#36719,#36720,#36721,#36722,#36723,#36724,#36725,#36726,
#36727,#36728,#36729,#36730,#36731,#36732,#36733,#36734,#36735,#36736,#36737,
#36738,#36739,#36740,#36741,#36742,#36743,#36744,#36745,#36746,#36747,#36748,
#36749,#36750,#36751,#36752,#36753,#36754,#36755,#36756,#36757,#36758,#36759,
#36760,#36761,#36762,#36763,#36764,#36765,#36766,#36767,#36768,#36769,#36770,
#36771,#36772,#36773,#36774,#36775,#36776,#36777,#36778,#36779,#36780,#36781,
#36782,#36783,#36784,#36785,#36786,#36787,#36788,#36789,#36790,#36791,#36792,
#36793,#36794,#36795,#36796,#36797,#36798,#36799,#36800,#36801,#36802,#36803,
#36804,#36805,#36806,#36807,#36808,#36809,#36810,#36811,#36812,#36813,#36814,
#36815,#36816,#36817,#36818,#36819,#36820,#36821,#36822,#36823,#36824,#36825,
#36826,#36827,#36828,#36829,#36830,#36831,#36832,#36833,#36834,#36835,#36836,
#36837,#36838,#36839,#36840,#36841,#36842,#36843,#36844,#36845,#36846,#36847,
#36848,#36849,#36850,#36851,#36852,#36853,#36854,#36855,#36856,#36857,#36858,
#36859,#36860,#36861,#36862,#36863,#36864,#36865,#36866,#36867,#36868,#36869,
#36870,#36871,#36872,#36873,#36874,#36875,#36876,#36877,#36878,#36879),
(#36880,#36881,#36882,#36883,#36884,#36885,#36886,#36887,#36888,#36889,
#36890,#36891,#36892,#36893,#36894,#36895,#36896,#36897,#36898,#36899,#36900,
#36901,#36902,#36903,#36904,#36905,#36906,#36907,#36908,#36909,#36910,#36911,
#36912,#36913,#36914,#36915,#36916,#36917,#36918,#36919,#36920,#36921,#36922,
#36923,#36924,#36925,#36926,#36927,#36928,#36929,#36930,#36931,#36932,#36933,
#36934,#36935,#36936,#36937,#36938,#36939,#36940,#36941,#36942,#36943,#36944,
#36945,#36946,#36947,#36948,#36949,#36950,#36951,#36952,#36953,#36954,#36955,
#36956,#36957,#36958,#36959,#36960,#36961,#36962,#36963,#36964,#36965,#36966,
#36967,#36968,#36969,#36970,#36971,#36972,#36973,#36974,#36975,#36976,#36977,
#36978,#36979,#36980,#36981,#36982,#36983,#36984,#36985,#36986,#36987,#36988,
#36989,#36990,#36991,#36992,#36993,#36994,#36995,#36996,#36997,#36998,#36999,
#37000,#37001,#37002,#37003,#37004,#37005,#37006,#37007,#37008,#37009,#37010,
#37011,#37012,#37013,#37014,#37015,#37016,#37017,#37018,#37019,#37020,#37021,
#37022,#37023,#37024,#37025,#37026,#37027,#37028,#37029,#37030,#37031,#37032,
#37033,#37034,#37035,#37036,#37037,#37038,#37039,#37040,#37041,#37042,#37043,
#37044,#37045,#37046,#37047,#37048,#37049,#37050,#37051,#37052,#37053,#37054,
#37055,#37056,#37057,#37058,#37059,#37060,#37061,#37062,#37063,#37064,#37065,
#37066,#37067,#37068,#37069,#37070,#37071,#37072,#37073,#37074,#37075,#37076,
#37077,#37078,#37079,#37080,#37081,#37082,#37083,#37084,#37085,#37086,#37087,
#37088,#37089,#37090,#37091,#37092,#37093,#37094,#37095,#37096,#37097,#37098,
#37099,#37100,#37101,#37102,#37103,#37104,#37105,#37106,#37107,#37108,#37109,
#37110,#37111,#37112,#37113,#37114,#37115,#37116,#37117,#37118,#37119,#37120,
#37121,#37122,#37123,#37124,#37125,#37126,#37127,#37128,#37129,#37130,#37131,
#37132,#37133,#37134,#37135,#37136,#37137,#37138,#37139,#37140,#37141,#37142,
#37143,#37144,#37145,#37146,#37147,#37148,#37149,#37150,#37151,#37152,#37153,
#37154,#37155,#37156,#37157,#37158,#37159,#37160,#37161,#37162,#37163,#37164,
#37165,#37166,#37167,#37168,#37169,#37170,#37171,#37172,#37173,#37174,#37175,
#37176,#37177,#37178,#37179,#37180,#37181,#37182,#37183,#37184,#37185,#37186,
#37187,#37188,#37189,#37190,#37191,#37192,#37193,#37194,#37195,#37196,#37197,
#37198,#37199,#37200,#37201,#37202,#37203,#37204,#37205,#37206,#37207,#37208,
#37209,#37210,#37211,#37212,#37213,#37214,#37215,#37216,#37217,#37218,#37219,
#37220,#37221,#37222,#37223,#37224,#37225,#37226,#37227,#37228,#37229,#37230,
#37231,#37232,#37233,#37234,#37235,#37236,#37237,#37238,#37239,#37240,#37241,
#37242,#37243,#37244,#37245,#37246)),.UNSPECIFIED.,.F.,.F.,.F.,(4,4),(4,
1,1,1,1,1,1,1,1,1,1,1,1,1,1,1,1,1,1,1,1,1,1,1,1,1,1,1,1,1,1,1,1,1,1,1,1,
1,1,1,1,1,1,1,1,1,1,1,1,1,1,1,1,1,1,1,1,1,1,1,1,1,1,1,1,1,1,1,1,1,1,1,1,
1,1,1,1,1,1,1,1,1,1,1,1,1,1,1,1,1,1,1,1,1,1,1,1,1,1,1,1,1,1,1,1,1,1,1,1,
1,1,1,1,1,1,1,1,1,1,1,1,1,1,1,1,1,1,1,1,1,1,1,1,1,1,1,1,1,1,1,1,1,1,1,1,
1,1,1,1,1,1,1,1,1,1,1,1,1,1,1,1,1,1,1,1,1,1,1,1,1,1,1,1,1,1,1,1,1,1,1,1,
1,1,1,1,1,1,1,1,1,1,1,1,1,1,1,1,1,1,1,1,1,1,1,1,1,1,1,1,1,1,1,1,1,1,1,1,
1,1,1,1,1,1,1,1,1,1,1,1,1,1,1,1,1,1,1,1,1,1,1,1,1,1,1,1,1,1,1,1,1,1,1,1,
1,1,1,1,1,1,1,1,1,1,1,1,1,1,1,1,1,1,1,1,1,1,1,1,1,1,1,1,1,1,1,1,1,1,1,1,
1,1,1,1,1,1,1,1,1,1,1,1,1,1,1,1,1,1,1,1,1,1,1,1,1,1,1,1,1,1,1,1,1,1,1,1,
1,1,1,1,1,1,1,1,1,1,1,1,1,1,1,1,1,1,1,1,1,1,1,1,1,1,1,1,1,1,1,1,1,1,1,1,
1,1,1,4),(-5.96503795939263E-5,0.115340908092672),(8.30592286723182,8.80479480237994,
9.30366673752807,9.80253867267619,10.3014106078243,10.8002825429724,11.2991544781206,
11.7980264132687,12.2968983484168,12.7957702835649,13.2946422187131,13.7935141538612,
14.2923860890093,14.7912580241574,15.2901299593056,15.7890018944537,16.2878738296018,
16.7867457647499,17.2856176998981,17.7844896350462,18.2833615701943,18.7822335053424,
19.2811054404905,19.7799773756387,20.2788493107868,20.7777212459349,21.276593181083,
21.7754651162312,22.2743370513793,22.7732089865274,23.2720809216755,23.7709528568237,
24.2698247919718,24.7686967271199,25.267568662268,25.7664405974162,26.2653125325643,
26.7641844677124,27.2630564028605,27.7619283380087,28.2608002731568,28.7596722083049,
29.258544143453,29.7574160786012,30.2562880137493,30.7551599488974,31.2540318840455,
31.7529038191936,32.2517757543418,32.7506476894899,33.249519624638,33.7483915597861,
34.2472634949343,34.7461354300824,35.2450073652305,35.7438793003786,36.2427512355268,
36.7416231706749,37.240495105823,37.7393670409711,38.2382389761193,38.7371109112674,
39.2359828464155,39.7348547815636,40.2337267167118,40.7325986518599,41.231470587008,
41.7303425221561,42.2292144573043,42.7280863924524,43.2269583276005,43.7258302627486,
44.2247021978968,44.7235741330449,45.222446068193,45.7213180033411,46.2201899384892,
46.7190618736374,47.2179338087855,47.7168057439336,48.2156776790817,48.7145496142299,
49.213421549378,49.7122934845261,50.2111654196742,50.7100373548224,51.2089092899705,
51.7077812251186,52.2066531602667,52.7055250954149,53.204397030563,53.7032689657111,
54.2021409008592,54.7010128360074,55.1998847711555,55.6987567063036,56.1976286414517,
56.6965005765999,57.195372511748,57.6942444468961,58.1931163820442,58.6919883171924,
59.1908602523405,59.6897321874886,60.1886041226367,60.6874760577848,61.186347992933,
61.6852199280811,62.1840918632292,62.6829637983773,63.1818357335255,63.6807076686736,
64.1795796038217,64.6784515389698,65.177323474118,65.6761954092661,66.1750673444142,
66.6739392795623,67.1728112147104,67.6716831498586,68.1705550850067,68.6694270201548,
69.168298955303,69.6671708904511,70.1660428255992,70.6649147607473,71.1637866958955,
71.6626586310436,72.1615305661917,72.6604025013398,73.1592744364879,73.6581463716361,
74.1570183067842,74.6558902419323,75.1547621770804,75.6536341122286,76.1525060473767,
76.6513779825248,77.1502499176729,77.6491218528211,78.1479937879692,78.6468657231173,
79.1457376582654,79.6446095934135,80.1434815285617,80.6423534637098,81.1412253988579,
81.640097334006,82.1389692691542,82.6378412043023,83.1367131394504,83.6355850745985,
84.1344570097467,84.6333289448948,85.1322008800429,85.631072815191,86.1299447503392,
86.6288166854873,87.1276886206354,87.6265605557835,88.1254324909317,88.6243044260798,
89.1231763612279,89.622048296376,90.1209202315242,90.6197921666723,91.1186641018204,
91.6175360369685,92.1164079721167,92.6152799072648,93.1141518424129,93.613023777561,
94.1118957127092,94.6107676478573,95.1096395830054,95.6085115181535,96.1073834533017,
96.6062553884498,97.1051273235979,97.603999258746,98.1028711938941,98.6017431290423,
99.1006150641904,99.5994869993385,100.098358934487,100.597230869635,101.096102804783,
101.594974739931,102.093846675079,102.592718610227,103.091590545375,103.590462480524,
104.089334415672,104.58820635082,105.087078285968,105.585950221116,106.084822156264,
106.583694091412,107.08256602656,107.581437961709,108.080309896857,108.579181832005,
109.078053767153,109.576925702301,110.075797637449,110.574669572597,111.073541507745,
111.572413442893,112.071285378042,112.57015731319,113.069029248338,113.567901183486,
114.066773118634,114.565645053782,115.06451698893,115.563388924078,116.062260859227,
116.561132794375,117.060004729523,117.558876664671,118.057748599819,118.556620534967,
119.055492470115,119.554364405263,120.053236340412,120.55210827556,121.050980210708,
121.549852145856,122.048724081004,122.547596016152,123.0464679513,123.545339886448,
124.044211821597,124.543083756745,125.041955691893,125.540827627041,126.039699562189,
126.538571497337,127.037443432485,127.536315367633,128.035187302782,128.53405923793,
129.032931173078,129.531803108226,130.030675043374,130.529546978522,131.02841891367,
131.527290848818,132.026162783967,132.525034719115,133.023906654263,133.522778589411,
134.021650524559,134.520522459707,135.019394394855,135.518266330003,136.017138265152,
136.5160102003,137.014882135448,137.513754070596,138.012626005744,138.511497940892,
139.01036987604,139.509241811188,140.008113746337,140.506985681485,141.005857616633,
141.504729551781,142.003601486929,142.502473422077,143.001345357225,143.500217292373,
143.999089227522,144.49796116267,144.996833097818,145.495705032966,145.994576968114,
146.493448903262,146.99232083841,147.491192773558,147.990064708707,148.488936643855,
148.987808579003,149.486680514151,149.985552449299,150.484424384447,150.983296319595,
151.482168254743,151.981040189892,152.47991212504,152.978784060188,153.477655995336,
153.976527930484,154.475399865632,154.97427180078,155.473143735928,155.972015671077,
156.470887606225,156.969759541373,157.468631476521,157.967503411669,158.466375346817,
158.965247281965,159.464119217113,159.962991152262,160.46186308741,160.960735022558,
161.459606957706,161.958478892854,162.457350828002,162.95622276315,163.455094698298,
163.953966633447,164.452838568595,164.951710503743,165.450582438891,165.949454374039,
166.448326309187,166.947198244335,167.446070179483,167.944942114632,168.44381404978,
168.942685984928,169.441557920076,169.940429855224,170.439301790372,170.93817372552,
171.437045660668,171.935917595817,172.434789530965,172.933661466113,173.432533401261,
173.931405336409,174.430277271557,174.929149206705,175.428021141853,175.926893077002,
176.42576501215,176.924636947298,177.423508882446,177.922380817594,178.421252752742,
178.92012468789,179.418996623038,179.917868558187,180.416740493335,180.915612428483,
181.414484363631,181.913356298779,182.412228233927,182.911100169075,183.409972104223,
183.908844039372,184.40771597452,184.906587909668,185.405459844816,185.904331779964,
186.403203715112,186.90207565026,187.400947585408,187.899819520556,188.398691455705,
188.897563390853,189.396435326001,189.895366911529),.UNSPECIFIED.);
#152=B_SPLINE_CURVE_WITH_KNOTS('',3,(#5917,#5918,#5919,#5920,#5921,#5922,
#5923,#5924,#5925,#5926,#5927,#5928),.UNSPECIFIED.,.F.,.F.,(4,1,1,1,1,1,
1,1,1,4),(80.7654236598523,81.1939800971667,81.6928451794136,82.1917102616605,
82.6905753439074,83.1894404261542,83.6883055084011,84.187170590648,84.6860356728949,
84.8230016469244),.UNSPECIFIED.);
#153=B_SPLINE_CURVE_WITH_KNOTS('',3,(#5930,#5931,#5932,#5933,#5934),
 .UNSPECIFIED.,.F.,.F.,(4,1,4),(84.8230016469244,85.1849007551417,85.6837658373886),
 .UNSPECIFIED.);
#154=B_SPLINE_CURVE_WITH_KNOTS('',3,(#5938,#5939,#5940,#5941,#5942,#5943,
#5944,#5945,#5946,#5947,#5948,#5949,#5950,#5951,#5952,#5953,#5954,#5955,
#5956,#5957,#5958,#5959,#5960,#5961,#5962,#5963,#5964,#5965,#5966,#5967,
#5968,#5969,#5970,#5971,#5972,#5973,#5974,#5975,#5976,#5977,#5978,#5979,
#5980,#5981,#5982,#5983,#5984,#5985,#5986,#5987,#5988,#5989),
 .UNSPECIFIED.,.F.,.F.,(4,3,3,3,3,3,3,3,3,3,3,3,3,3,3,3,3,4),(84.8230016469244,
84.9058580301686,84.9887137387844,85.0715624591206,85.1544337152411,85.2372418060283,
85.3204458619835,85.4036336567022,85.4868246260799,85.5700099876162,85.6532174303604,
85.7361068882752,85.8191359181166,85.9021481942019,85.9851620989545,86.0681715464416,
86.151200160365,86.2062322090242),.UNSPECIFIED.);
#155=B_SPLINE_CURVE_WITH_KNOTS('',3,(#5990,#5991,#5992,#5993,#5994,#5995,
#5996,#5997,#5998,#5999,#6000,#6001),.UNSPECIFIED.,.F.,.F.,(4,1,1,1,1,1,
1,1,1,4),(80.7654089732259,81.2463211480533,81.7451862303002,82.2440513125471,
82.742916394794,83.2417814770408,83.7406465592877,84.2395116415346,84.7383767237815,
84.8230016469244),.UNSPECIFIED.);
#156=B_SPLINE_CURVE_WITH_KNOTS('',3,(#6007,#6008,#6009,#6010,#6011,#6012,
#6013,#6014,#6015,#6016,#6017,#6018,#6019,#6020,#6021,#6022,#6023,#6024,
#6025,#6026,#6027,#6028,#6029,#6030,#6031,#6032,#6033,#6034,#6035,#6036,
#6037,#6038,#6039,#6040,#6041,#6042,#6043,#6044,#6045,#6046,#6047,#6048,
#6049,#6050,#6051,#6052,#6053,#6054,#6055,#6056,#6057,#6058,#6059,#6060,
#6061,#6062,#6063,#6064,#6065,#6066,#6067,#6068,#6069,#6070,#6071,#6072,
#6073,#6074,#6075,#6076,#6077,#6078,#6079,#6080,#6081,#6082,#6083,#6084,
#6085,#6086,#6087,#6088,#6089,#6090,#6091,#6092,#6093,#6094,#6095,#6096,
#6097,#6098,#6099,#6100,#6101,#6102,#6103,#6104,#6105,#6106,#6107,#6108,
#6109,#6110,#6111,#6112,#6113,#6114,#6115,#6116,#6117,#6118,#6119,#6120,
#6121,#6122,#6123,#6124,#6125,#6126,#6127,#6128,#6129,#6130,#6131,#6132,
#6133,#6134,#6135,#6136,#6137,#6138,#6139,#6140,#6141,#6142,#6143,#6144,
#6145,#6146,#6147,#6148,#6149,#6150,#6151,#6152,#6153,#6154),
 .UNSPECIFIED.,.F.,.F.,(4,3,3,3,3,3,3,3,3,3,3,3,3,3,3,3,3,3,3,3,3,3,3,3,
3,3,3,3,3,3,3,3,3,3,3,3,3,3,3,3,3,3,3,3,3,3,3,3,3,4),(74.4822133280158,
74.5653991646366,74.6486051631925,74.7087340279573,74.7919387913187,74.8751273240303,
74.9583190715775,75.0415052315879,75.1247134988495,75.2075991102042,75.2908038725438,
75.3739924042304,75.4571841507579,75.5403703097531,75.6235785760172,75.7064641924511,
75.789668956311,75.8728574895209,75.9560492375621,76.039235398063,76.1224436658041,
76.205329274698,76.2885340372514,76.3717225691568,76.454914315908,76.5381004751292,
76.6213087416209,76.7041943569448,76.7873991181458,76.8705876486823,76.9537793940503,
77.0369655518835,77.1201738169931,77.2030594391917,77.2862642100853,77.3694527503662,
77.452644505469,77.5358306730124,77.619038947697,77.7019245214386,77.7851292641372,
77.8683177761065,77.9515095029856,78.034695642409,78.1179038894172,78.2007896036855,
78.2855462877003,78.3686837869672,78.454250063356,78.5398163397448),
 .UNSPECIFIED.);
#157=B_SPLINE_CURVE_WITH_KNOTS('',3,(#6155,#6156,#6157,#6158,#6159,#6160,
#6161,#6162,#6163),.UNSPECIFIED.,.F.,.F.,(4,1,1,1,1,1,4),(78.5398163723456,
78.6996546859323,79.1985197681792,79.6973848504261,80.196249932673,80.6951150149198,
80.7654236598523),.UNSPECIFIED.);
#158=B_SPLINE_CURVE_WITH_KNOTS('',3,(#6165,#6166,#6167,#6168,#6169,#6170,
#6171,#6172,#6173),.UNSPECIFIED.,.F.,.F.,(4,1,1,1,1,1,4),(78.5398163397448,
78.7519957368189,79.2508608190658,79.7497259013127,80.2485909835596,80.7474560658064,
80.7654089732259),.UNSPECIFIED.);
#159=B_SPLINE_CURVE_WITH_KNOTS('',3,(#6174,#6175,#6176,#6177,#6178,#6179,
#6180,#6181,#6182,#6183,#6184,#6185),.UNSPECIFIED.,.F.,.F.,(4,1,1,1,1,1,
1,1,1,4),(74.4822262911247,74.7610750788439,75.2599401610908,75.7588052433377,
76.2576703255846,76.7565354078314,77.2554004900783,77.7542655723252,78.2531306545721,
78.5398163397448),.UNSPECIFIED.);
#160=B_SPLINE_CURVE_WITH_KNOTS('',3,(#6191,#6192,#6193,#6194,#6195,#6196,
#6197,#6198,#6199,#6200,#6201,#6202,#6203,#6204,#6205,#6206,#6207,#6208,
#6209,#6210,#6211,#6212,#6213,#6214,#6215,#6216,#6217,#6218,#6219,#6220,
#6221,#6222,#6223,#6224,#6225,#6226,#6227,#6228,#6229,#6230,#6231,#6232,
#6233,#6234,#6235,#6236,#6237,#6238,#6239,#6240,#6241,#6242,#6243,#6244,
#6245,#6246,#6247,#6248,#6249,#6250,#6251,#6252,#6253,#6254,#6255,#6256,
#6257,#6258,#6259,#6260,#6261,#6262,#6263,#6264,#6265,#6266,#6267,#6268,
#6269,#6270,#6271,#6272,#6273,#6274,#6275,#6276,#6277,#6278,#6279,#6280,
#6281,#6282,#6283,#6284,#6285,#6286,#6287,#6288,#6289,#6290,#6291,#6292,
#6293,#6294,#6295,#6296,#6297,#6298,#6299,#6300,#6301,#6302,#6303,#6304,
#6305,#6306,#6307,#6308,#6309,#6310,#6311,#6312,#6313,#6314,#6315,#6316,
#6317,#6318,#6319,#6320,#6321,#6322,#6323,#6324,#6325,#6326,#6327,#6328,
#6329,#6330,#6331,#6332,#6333,#6334,#6335,#6336,#6337,#6338,#6339,#6340,
#6341),.UNSPECIFIED.,.F.,.F.,(4,3,3,3,3,3,3,3,3,3,3,3,3,3,3,3,3,3,3,3,3,
3,3,3,3,3,3,3,3,3,3,3,3,3,3,3,3,3,3,3,3,3,3,3,3,3,3,3,3,3,4),(68.1990246102961,
68.2234879587479,68.3066927217448,68.3898812540909,68.473073001274,68.5562591609217,
68.6394674278267,68.7223530409948,68.805557803992,68.8887463363385,68.9719380835218,
69.0551242431698,69.1383325100748,69.2212181232417,69.3044228862387,69.3876114185846,
69.4708031657675,69.5539893254153,69.6371975923201,69.7200832054885,69.8032879684856,
69.8864765008317,69.969668248015,70.052854407663,70.136062674568,70.2189482877354,
70.3021530507327,70.3853415830785,70.4685333302618,70.5517194899096,70.6349277568148,
70.7178133699823,70.8010181329782,70.8842066653234,70.9673984125055,71.0505845721522,
71.1337928390561,71.2166784522292,71.2998832152294,71.3830717475779,71.4662634947639,
71.5494496544144,71.6326579213223,71.7155435344761,71.7987482974668,71.8819368298066,
71.9651285769834,72.0483147366248,72.1315230035237,72.2144086167229,72.2566310325652),
 .UNSPECIFIED.);
#161=B_SPLINE_CURVE_WITH_KNOTS('',3,(#6342,#6343,#6344,#6345,#6346,#6347,
#6348,#6349,#6350,#6351,#6352,#6353,#6354,#6355,#6356,#6357,#6358,#6359,
#6360,#6361,#6362,#6363,#6364,#6365,#6366,#6367,#6368,#6369,#6370,#6371,
#6372,#6373,#6374,#6375,#6376,#6377,#6378,#6379,#6380,#6381,#6382,#6383,
#6384,#6385,#6386,#6387,#6388,#6389,#6390,#6391,#6392,#6393,#6394,#6395,
#6396,#6397,#6398,#6399,#6400,#6401,#6402,#6403,#6404,#6405,#6406,#6407,
#6408,#6409,#6410,#6411,#6412,#6413,#6414,#6415,#6416,#6417,#6418,#6419,
#6420,#6421,#6422,#6423,#6424,#6425,#6426),.UNSPECIFIED.,.F.,.F.,(4,3,3,
3,3,3,3,3,3,3,3,3,3,3,3,3,3,3,3,3,3,3,3,3,3,3,3,3,4),(72.2566310327204,
72.3395787750688,72.4225108202044,72.5054456631146,72.5883776325168,72.6713290333548,
72.7132736989698,72.7964784619549,72.8796669942889,72.9628587414601,73.046044901096,
73.1292531679893,73.2121387812167,73.2953435442142,73.3785320765606,73.4617238237443,
73.5449099833926,73.6281182502978,73.7110038634636,73.7942086265049,73.8773971588956,
73.9605889061234,74.0437750658158,74.1269833327648,74.2098689457104,74.2930744028643,
74.3762623723983,74.4594439181691,74.4822133280158),.UNSPECIFIED.);
#162=B_SPLINE_CURVE_WITH_KNOTS('',3,(#6428,#6429,#6430,#6431,#6432,#6433,
#6434,#6435,#6436),.UNSPECIFIED.,.F.,.F.,(4,1,1,1,1,1,4),(72.2566310325652,
72.2667496676095,72.7656147498564,73.2644798321033,73.7633449143502,74.2622099965971,
74.4822262911247),.UNSPECIFIED.);
#163=B_SPLINE_CURVE_WITH_KNOTS('',3,(#6437,#6438,#6439,#6440,#6441,#6442,
#6443,#6444,#6445,#6446,#6447,#6448,#6449,#6450,#6451,#6452,#6453,#6454,
#6455,#6456,#6457,#6458,#6459,#6460,#6461,#6462,#6463,#6464,#6465,#6466,
#6467,#6468,#6469,#6470,#6471,#6472,#6473,#6474,#6475,#6476,#6477,#6478,
#6479,#6480,#6481,#6482,#6483,#6484,#6485,#6486,#6487,#6488,#6489,#6490,
#6491,#6492,#6493,#6494,#6495,#6496,#6497,#6498,#6499,#6500,#6501,#6502,
#6503,#6504,#6505,#6506,#6507,#6508,#6509,#6510,#6511,#6512,#6513,#6514,
#6515,#6516,#6517,#6518,#6519,#6520,#6521,#6522,#6523,#6524,#6525,#6526,
#6527,#6528,#6529,#6530,#6531,#6532,#6533,#6534,#6535,#6536,#6537,#6538,
#6539,#6540,#6541,#6542,#6543,#6544,#6545,#6546,#6547,#6548,#6549,#6550,
#6551,#6552,#6553,#6554,#6555,#6556,#6557,#6558,#6559,#6560,#6561,#6562,
#6563,#6564,#6565,#6566,#6567,#6568,#6569,#6570,#6571,#6572,#6573,#6574,
#6575,#6576,#6577,#6578,#6579,#6580,#6581,#6582,#6583,#6584),
 .UNSPECIFIED.,.F.,.F.,(4,3,3,3,3,3,3,3,3,3,3,3,3,3,3,3,3,3,3,3,3,3,3,3,
3,3,3,3,3,3,3,3,3,3,3,3,3,3,3,3,3,3,3,3,3,3,3,3,3,4),(68.1990161073015,
68.2758290096345,68.3590337726316,68.4422223049775,68.5254140521607,68.6086002118086,
68.6918084787137,68.7746940918814,68.8578988548785,68.9410873872244,69.0242791344076,
69.1074652940555,69.1906735609605,69.2735591741283,69.3567639371251,69.4399524694712,
69.5231442166544,69.6063303763024,69.6895386432074,69.7724242563752,69.8556290193721,
69.9388175517181,70.0220092989012,70.1051954585491,70.1884037254542,70.271289338622,
70.3544941016189,70.4376826339646,70.5208743811479,70.6040605407956,70.6872688077007,
70.7701544208689,70.8533591838659,70.9365477162118,71.0197394633952,71.1029256230433,
71.1861338899484,71.2690195031158,71.352224266113,71.4354127984596,71.5186045456429,
71.6017907052906,71.6849989721958,71.7678845853627,71.8510125628734,71.9341240557072,
72.0172382375382,72.1003472864947,72.1834776083169,72.2566310325652),
 .UNSPECIFIED.);
#164=B_SPLINE_CURVE_WITH_KNOTS('',3,(#6590,#6591,#6592,#6593,#6594,#6595,
#6596,#6597,#6598,#6599,#6600,#6601),.UNSPECIFIED.,.F.,.F.,(4,1,1,1,1,1,
1,1,1,4),(61.9158664354373,62.2371069717854,62.7359720540323,63.2348371362792,
63.733702218526,64.2325673007729,64.7314323830198,65.2302974652667,65.7291625475135,
65.9734457216197),.UNSPECIFIED.);
#165=B_SPLINE_CURVE_WITH_KNOTS('',3,(#6602,#6603,#6604,#6605,#6606,#6607,
#6608,#6609,#6610,#6611,#6612,#6613,#6614,#6615,#6616,#6617,#6618,#6619,
#6620,#6621,#6622,#6623,#6624,#6625,#6626,#6627,#6628,#6629,#6630,#6631,
#6632,#6633,#6634,#6635,#6636,#6637,#6638,#6639,#6640,#6641,#6642,#6643,
#6644,#6645,#6646,#6647,#6648,#6649,#6650,#6651,#6652,#6653,#6654,#6655,
#6656,#6657,#6658,#6659,#6660,#6661,#6662,#6663,#6664,#6665,#6666,#6667,
#6668,#6669,#6670,#6671,#6672,#6673,#6674,#6675,#6676,#6677,#6678,#6679,
#6680,#6681,#6682,#6683),.UNSPECIFIED.,.F.,.F.,(4,3,3,3,3,3,3,3,3,3,3,3,
3,3,3,3,3,3,3,3,3,3,3,3,3,3,3,4),(65.9734457253856,66.0575770114745,66.1428023206174,
66.2280276297604,66.3112323927575,66.3944209251034,66.4776126722867,66.5607988319345,
66.6440070988396,66.7268927120073,66.8100974750044,66.8932860073503,66.9764777545334,
67.0596639141813,67.1428721810863,67.2257577942542,67.3089625572514,67.3921510895973,
67.4753428367804,67.5585289964282,67.6417372633332,67.724622876501,67.8078273552862,
67.8910155036496,67.974204708283,68.0573885356163,68.1405895310058,68.1990246102961),
 .UNSPECIFIED.);
#166=B_SPLINE_CURVE_WITH_KNOTS('',3,(#6685,#6686,#6687,#6688,#6689,#6690,
#6691,#6692,#6693,#6694,#6695,#6696,#6697,#6698,#6699,#6700,#6701,#6702,
#6703,#6704,#6705,#6706,#6707,#6708,#6709,#6710,#6711,#6712,#6713,#6714,
#6715,#6716,#6717,#6718,#6719,#6720,#6721,#6722,#6723,#6724,#6725,#6726,
#6727,#6728,#6729,#6730,#6731,#6732,#6733,#6734,#6735,#6736,#6737,#6738,
#6739,#6740,#6741,#6742,#6743,#6744,#6745,#6746,#6747,#6748,#6749,#6750,
#6751,#6752,#6753,#6754,#6755,#6756,#6757,#6758,#6759,#6760,#6761,#6762,
#6763,#6764,#6765,#6766),.UNSPECIFIED.,.F.,.F.,(4,3,3,3,3,3,3,3,3,3,3,3,
3,3,3,3,3,3,3,3,3,3,3,3,3,3,3,4),(65.9734457253856,66.0568706822057,66.1402945367021,
66.2237400485274,66.280368680647,66.3635734436441,66.4467619759899,66.529953723173,
66.6131398828208,66.6963481497259,66.7792337628939,66.8624385258909,66.945627058237,
67.0288188054201,67.1120049650679,67.1952132319729,67.2780988451408,67.3613036081377,
67.4444921404837,67.5276838876669,67.6108700473146,67.6940783142196,67.7769639273876,
67.8601680001445,67.9448800269338,68.0280644468231,68.1135402770623,68.1990161073015),
 .UNSPECIFIED.);
#167=B_SPLINE_CURVE_WITH_KNOTS('',3,(#6767,#6768,#6769,#6770,#6771,#6772,
#6773,#6774,#6775,#6776,#6777,#6778),.UNSPECIFIED.,.F.,.F.,(4,1,1,1,1,1,
1,1,1,4),(61.9158726512869,62.289448022672,62.7883131049189,63.2871781871658,
63.7860432694126,64.2849083516595,64.7837734339064,65.2826385161533,65.7815035984001,
65.9734456901994),.UNSPECIFIED.);
#168=B_SPLINE_CURVE_WITH_KNOTS('',3,(#6784,#6785,#6786,#6787,#6788,#6789,
#6790,#6791,#6792,#6793,#6794,#6795,#6796,#6797,#6798,#6799,#6800,#6801,
#6802,#6803,#6804,#6805,#6806,#6807,#6808,#6809,#6810,#6811,#6812,#6813,
#6814,#6815,#6816,#6817,#6818,#6819,#6820,#6821,#6822,#6823,#6824,#6825,
#6826,#6827,#6828,#6829,#6830,#6831,#6832,#6833,#6834,#6835,#6836,#6837,
#6838,#6839,#6840,#6841,#6842,#6843,#6844,#6845,#6846,#6847,#6848,#6849,
#6850,#6851,#6852,#6853,#6854,#6855,#6856,#6857,#6858,#6859,#6860,#6861,
#6862,#6863,#6864,#6865,#6866,#6867,#6868,#6869,#6870,#6871,#6872,#6873,
#6874,#6875,#6876,#6877,#6878,#6879,#6880,#6881,#6882,#6883,#6884,#6885,
#6886,#6887,#6888,#6889,#6890,#6891,#6892,#6893,#6894,#6895,#6896,#6897,
#6898,#6899,#6900,#6901,#6902,#6903,#6904,#6905,#6906,#6907,#6908,#6909,
#6910,#6911,#6912,#6913,#6914,#6915,#6916,#6917,#6918,#6919,#6920,#6921,
#6922,#6923,#6924,#6925,#6926,#6927,#6928,#6929,#6930,#6931,#6932,#6933,
#6934),.UNSPECIFIED.,.F.,.F.,(4,3,3,3,3,3,3,3,3,3,3,3,3,3,3,3,3,3,3,3,3,
3,3,3,3,3,3,3,3,3,3,3,3,3,3,3,3,3,3,3,3,3,3,3,3,3,3,3,3,3,4),(55.6326446456766,
55.7158491503551,55.751860902576,55.835065665573,55.9182541979186,56.0014459451018,
56.0846321047497,56.1678403716548,56.2507259848229,56.3339307478201,56.4171192801657,
56.5003110273488,56.5834971869966,56.6667054539017,56.7495910670697,56.8327958300666,
56.9159843624127,56.9991761095957,57.0823622692435,57.1655705361485,57.2484561493166,
57.3316609123136,57.4148494446596,57.4980411918429,57.5812273514908,57.6644356183958,
57.7473212315635,57.8305259945606,57.9137145269063,57.9969062740895,58.0800924337372,
58.1633007006423,58.2461863138104,58.3293910768073,58.4125796091535,58.4957713563367,
58.5789575159845,58.6621657828895,58.7450513960573,58.8282561590543,58.9114446914002,
58.9946364385832,59.0778225982313,59.1610308651363,59.2439164783041,59.3268318318306,
59.4097299979322,59.4926282254384,59.5755226544865,59.6584334114035,59.690260418206),
 .UNSPECIFIED.);
#169=B_SPLINE_CURVE_WITH_KNOTS('',3,(#6935,#6936,#6937,#6938,#6939,#6940,
#6941,#6942,#6943),.UNSPECIFIED.,.F.,.F.,(4,1,1,1,1,1,4),(59.690260418206,
59.742781560551,60.2416466427979,60.7405117250448,61.2393768072916,61.7382418895385,
61.9158664354373),.UNSPECIFIED.);
#170=B_SPLINE_CURVE_WITH_KNOTS('',3,(#6945,#6946,#6947,#6948,#6949,#6950,
#6951,#6952,#6953),.UNSPECIFIED.,.F.,.F.,(4,1,1,1,1,1,4),(59.690260418206,
59.7951226114376,60.2939876936845,60.7928527759314,61.2917178581782,61.7905829404251,
61.9158726512869),.UNSPECIFIED.);
#171=B_SPLINE_CURVE_WITH_KNOTS('',3,(#6954,#6955,#6956,#6957,#6958,#6959,
#6960,#6961,#6962,#6963,#6964,#6965,#6966,#6967,#6968,#6969,#6970,#6971,
#6972,#6973,#6974,#6975,#6976,#6977,#6978,#6979,#6980,#6981,#6982,#6983,
#6984,#6985,#6986,#6987,#6988,#6989,#6990,#6991,#6992,#6993,#6994,#6995,
#6996,#6997,#6998,#6999,#7000,#7001,#7002,#7003,#7004,#7005,#7006,#7007,
#7008,#7009,#7010,#7011,#7012,#7013,#7014,#7015,#7016,#7017,#7018,#7019,
#7020,#7021,#7022,#7023,#7024,#7025,#7026,#7027,#7028,#7029,#7030,#7031,
#7032,#7033,#7034,#7035,#7036,#7037,#7038,#7039,#7040,#7041,#7042,#7043,
#7044,#7045,#7046,#7047,#7048,#7049,#7050,#7051,#7052,#7053,#7054,#7055,
#7056,#7057,#7058,#7059,#7060,#7061,#7062,#7063,#7064,#7065,#7066,#7067,
#7068,#7069,#7070,#7071,#7072,#7073,#7074,#7075,#7076,#7077,#7078,#7079,
#7080,#7081,#7082,#7083,#7084,#7085,#7086,#7087,#7088,#7089,#7090,#7091,
#7092,#7093,#7094,#7095,#7096,#7097,#7098,#7099,#7100,#7101),
 .UNSPECIFIED.,.F.,.F.,(4,3,3,3,3,3,3,3,3,3,3,3,3,3,3,3,3,3,3,3,3,3,3,3,
3,3,3,3,3,3,3,3,3,3,3,3,3,3,3,3,3,3,3,3,3,3,3,3,3,4),(55.6326489767496,
55.7184254651061,55.8042019534626,55.8874067164596,55.970595248806,56.0537869959891,
56.136973155637,56.220181422542,56.3030670357095,56.3862717987066,56.4694603310523,
56.5526520782354,56.6358382378835,56.7190465047884,56.8019321179564,56.8851368809535,
56.9683254132997,57.0515171604829,57.1347033201307,57.2179115870357,57.3007972002032,
57.3840019632003,57.4671904955464,57.5503822427296,57.6335684023773,57.7167766692823,
57.7996622824501,57.8828670454471,57.9660555777933,58.0492473249765,58.1324334846246,
58.2156417515297,58.298527364697,58.3817321276939,58.4649206600397,58.5481124072229,
58.6312985668706,58.7145068337754,58.7973924469439,58.880597209941,58.9637857422865,
59.0469774894696,59.1301636491172,59.2133719160221,59.2962575291907,59.3791492032558,
59.4620306976914,59.5449010195121,59.627782428294,59.690260418206),
 .UNSPECIFIED.);
#172=B_SPLINE_CURVE_WITH_KNOTS('',3,(#7107,#7108,#7109,#7110,#7111,#7112,
#7113,#7114,#7115,#7116,#7117,#7118,#7119,#7120,#7121,#7122,#7123,#7124,
#7125,#7126,#7127,#7128,#7129,#7130,#7131,#7132,#7133,#7134,#7135,#7136,
#7137,#7138,#7139,#7140,#7141,#7142,#7143,#7144,#7145,#7146,#7147,#7148,
#7149,#7150,#7151,#7152,#7153,#7154,#7155,#7156,#7157,#7158,#7159,#7160,
#7161,#7162,#7163,#7164,#7165,#7166,#7167,#7168,#7169,#7170,#7171,#7172,
#7173,#7174,#7175,#7176,#7177,#7178,#7179,#7180,#7181,#7182,#7183,#7184,
#7185,#7186,#7187,#7188,#7189,#7190,#7191,#7192,#7193,#7194,#7195,#7196,
#7197,#7198,#7199,#7200,#7201,#7202,#7203,#7204,#7205,#7206,#7207,#7208,
#7209,#7210,#7211,#7212,#7213,#7214,#7215,#7216,#7217,#7218,#7219,#7220,
#7221,#7222,#7223,#7224,#7225,#7226,#7227,#7228,#7229,#7230,#7231,#7232,
#7233,#7234,#7235,#7236,#7237,#7238,#7239,#7240,#7241,#7242,#7243,#7244,
#7245,#7246,#7247,#7248,#7249,#7250,#7251,#7252,#7253,#7254),
 .UNSPECIFIED.,.F.,.F.,(4,3,3,3,3,3,3,3,3,3,3,3,3,3,3,3,3,3,3,3,3,3,3,3,
3,3,3,3,3,3,3,3,3,3,3,3,3,3,3,3,3,3,3,3,3,3,3,3,3,4),(49.3494924806201,
49.4326810632531,49.5158807763432,49.5990669442003,49.6822752488321,49.7654799156135,
49.8486846786105,49.9318732109565,50.0150649581396,50.0982511177874,50.1814593846924,
50.2643449978603,50.3475497608573,50.4307382932033,50.5139300403864,50.5971162000342,
50.6803244669392,50.7632100801072,50.8464148431043,50.9296033754502,51.0127951226334,
51.0959812822813,51.1791895491863,51.2620751623541,51.3452799253512,51.4284684576972,
51.5116602048803,51.5948463645282,51.6780546314332,51.760940244601,51.844145007598,
51.9273335399439,52.0105252871271,52.0937114467749,52.1769197136799,52.2598053268479,
52.343010089845,52.4261986221908,52.509390369374,52.5925765290218,52.6757847959268,
52.7586704090947,52.8418751720917,52.9250637044375,53.0082554516206,53.0914416112682,
53.1746498781732,53.2575354913416,53.3441594282935,53.4070751109103),
 .UNSPECIFIED.);
#173=B_SPLINE_CURVE_WITH_KNOTS('',3,(#7255,#7256,#7257,#7258,#7259,#7260,
#7261,#7262,#7263,#7264,#7265,#7266,#7267,#7268,#7269,#7270,#7271,#7272,
#7273,#7274,#7275,#7276,#7277,#7278,#7279,#7280,#7281,#7282,#7283,#7284,
#7285,#7286,#7287,#7288,#7289,#7290,#7291,#7292,#7293,#7294,#7295,#7296,
#7297,#7298,#7299,#7300,#7301,#7302,#7303,#7304,#7305,#7306,#7307,#7308,
#7309,#7310,#7311,#7312,#7313,#7314,#7315,#7316,#7317,#7318,#7319,#7320,
#7321,#7322,#7323,#7324,#7325,#7326,#7327,#7328,#7329,#7330,#7331,#7332,
#7333,#7334,#7335,#7336,#7337,#7338,#7339),.UNSPECIFIED.,.F.,.F.,(4,3,3,
3,3,3,3,3,3,3,3,3,3,3,3,3,3,3,3,3,3,3,3,3,3,3,3,3,4),(53.4070751110264,
53.4944064766669,53.577468684068,53.6605312927296,53.7436119100014,53.7564005735885,
53.8396053365855,53.9227938689313,54.0059856161145,54.0891717757623,54.1723800426672,
54.2552656558354,54.3384704188324,54.4216589511783,54.5048506983614,54.5880368580093,
54.6712451249142,54.7541307380822,54.8373355010792,54.920524033425,55.0037157806081,
55.0869019402558,55.1701102071608,55.2529958203291,55.3361997661843,55.419392877731,
55.5025745053791,55.5857617771024,55.6326446456766),.UNSPECIFIED.);
#174=B_SPLINE_CURVE_WITH_KNOTS('',3,(#7341,#7342,#7343,#7344,#7345,#7346,
#7347,#7348,#7349,#7350,#7351,#7352,#7353,#7354,#7355,#7356,#7357,#7358,
#7359,#7360,#7361,#7362,#7363,#7364,#7365,#7366,#7367,#7368,#7369,#7370,
#7371,#7372,#7373,#7374,#7375,#7376,#7377,#7378,#7379,#7380,#7381,#7382,
#7383,#7384,#7385,#7386,#7387,#7388,#7389,#7390,#7391,#7392,#7393,#7394,
#7395,#7396,#7397,#7398,#7399,#7400,#7401,#7402,#7403,#7404,#7405,#7406,
#7407,#7408,#7409,#7410,#7411,#7412,#7413,#7414,#7415,#7416,#7417,#7418,
#7419,#7420,#7421,#7422),.UNSPECIFIED.,.F.,.F.,(4,3,3,3,3,3,3,3,3,3,3,3,
3,3,3,3,3,3,3,3,3,3,3,3,3,3,3,4),(53.4070751111526,53.4899407286186,53.5728065866223,
53.6556666653888,53.7385482014372,53.8087416244751,53.8919463874721,53.9751349198181,
54.0583266670012,54.1415128266491,54.224721093554,54.307606706722,54.390811469719,
54.4740000020651,54.5571917492483,54.6403779088962,54.7235861758011,54.8064717889688,
54.8896765519659,54.9728650843119,55.056056831495,55.1392429911428,55.2224512580478,
55.3053368712157,55.3885448552999,55.4717348798802,55.5549254912121,55.6326489767496),
 .UNSPECIFIED.);
#175=B_SPLINE_CURVE_WITH_KNOTS('',3,(#7423,#7424,#7425,#7426,#7427,#7428,
#7429,#7430,#7431,#7432,#7433,#7434,#7435,#7436,#7437,#7438,#7439,#7440,
#7441,#7442,#7443,#7444,#7445,#7446,#7447,#7448,#7449,#7450,#7451,#7452,
#7453,#7454,#7455,#7456,#7457,#7458,#7459,#7460,#7461,#7462,#7463,#7464,
#7465,#7466,#7467,#7468,#7469,#7470,#7471,#7472,#7473,#7474,#7475,#7476,
#7477,#7478,#7479,#7480,#7481,#7482,#7483,#7484,#7485,#7486,#7487,#7488,
#7489,#7490,#7491,#7492,#7493,#7494,#7495,#7496,#7497,#7498,#7499,#7500,
#7501,#7502,#7503,#7504,#7505,#7506,#7507,#7508,#7509,#7510,#7511,#7512,
#7513,#7514,#7515,#7516,#7517,#7518,#7519,#7520,#7521,#7522,#7523,#7524,
#7525,#7526,#7527,#7528,#7529,#7530,#7531,#7532,#7533,#7534,#7535,#7536,
#7537,#7538,#7539,#7540,#7541,#7542,#7543,#7544,#7545,#7546,#7547,#7548,
#7549,#7550,#7551,#7552,#7553,#7554,#7555,#7556,#7557,#7558,#7559,#7560,
#7561,#7562,#7563,#7564,#7565,#7566,#7567,#7568,#7569,#7570,#7571,#7572,
#7573),.UNSPECIFIED.,.F.,.F.,(4,3,3,3,3,3,3,3,3,3,3,3,3,3,3,3,3,3,3,3,3,
3,3,3,3,3,3,3,3,3,3,3,3,3,3,3,3,3,3,3,3,3,3,3,3,3,3,3,3,3,4),(49.349485040032,
49.432683045519,49.5158673552897,49.5990562489482,49.6822420940411,49.7654475102057,
49.8178209665001,49.9010257294971,49.984214261843,50.0674060090262,50.150592168674,
50.233800435579,50.316686048747,50.399890811744,50.48307934409,50.5662710912732,
50.649457250921,50.732665517826,50.8155511309938,50.8987558939908,50.9819444263367,
51.0651361735199,51.1483223331677,51.2315306000727,51.3144162132407,51.3976209762378,
51.4808095085838,51.564001255767,51.6471874154149,51.7303956823199,51.8132812954876,
51.8964860584847,51.9796745908306,52.0628663380137,52.1460524976615,52.2292607645664,
52.3121463777345,52.3953511407315,52.4785396730773,52.5617314202605,52.6449175799084,
52.7281258468134,52.8110114599813,52.8942162229782,52.977404755324,53.060596502507,
53.1437826621548,53.2269909290597,53.3098765422282,53.3983951832703,53.4070751110264),
 .UNSPECIFIED.);
#176=B_SPLINE_CURVE_WITH_KNOTS('',3,(#7579,#7580,#7581,#7582,#7583,#7584,
#7585,#7586,#7587,#7588,#7589,#7590,#7591,#7592,#7593,#7594,#7595,#7596,
#7597,#7598,#7599,#7600,#7601,#7602,#7603,#7604,#7605,#7606,#7607,#7608,
#7609,#7610,#7611,#7612,#7613,#7614,#7615,#7616,#7617,#7618,#7619,#7620,
#7621,#7622,#7623,#7624,#7625,#7626,#7627,#7628,#7629,#7630,#7631,#7632,
#7633,#7634,#7635,#7636,#7637,#7638,#7639,#7640,#7641,#7642,#7643,#7644,
#7645,#7646,#7647,#7648,#7649,#7650,#7651,#7652,#7653,#7654,#7655,#7656,
#7657,#7658,#7659,#7660,#7661,#7662,#7663,#7664,#7665,#7666,#7667,#7668,
#7669,#7670,#7671,#7672,#7673,#7674,#7675,#7676,#7677,#7678,#7679,#7680,
#7681,#7682,#7683,#7684,#7685,#7686,#7687,#7688,#7689,#7690,#7691,#7692,
#7693,#7694,#7695,#7696,#7697,#7698,#7699,#7700,#7701,#7702,#7703,#7704,
#7705,#7706,#7707,#7708,#7709,#7710,#7711,#7712,#7713,#7714,#7715,#7716,
#7717,#7718,#7719,#7720,#7721,#7722,#7723,#7724,#7725,#7726,#7727,#7728,
#7729),.UNSPECIFIED.,.F.,.F.,(4,3,3,3,3,3,3,3,3,3,3,3,3,3,3,3,3,3,3,3,3,
3,3,3,3,3,3,3,3,3,3,3,3,3,3,3,3,3,3,3,3,3,3,3,3,3,3,3,3,3,4),(43.0662846573068,
43.1494705378359,43.2326756410144,43.2802338464041,43.3634386094009,43.4466271417468,
43.5298188889299,43.6130050485777,43.6962133154828,43.779098928651,43.8623036916481,
43.945492223994,44.0286839711771,44.1118701308249,44.1950783977299,44.2779640108978,
44.3611687738949,44.4443573062409,44.5275490534239,44.6107352130717,44.6939434799768,
44.7768290931447,44.8600338561417,44.9432223884882,45.0264141356714,45.1096002953193,
45.1928085622243,45.2756941753916,45.3588989383885,45.4420874707345,45.5252792179175,
45.6084653775653,45.6916736444701,45.7745592576385,45.8577640206358,45.9409525529818,
46.0241443001649,46.1073304598125,46.1905387267174,46.2734243398853,46.3566291028823,
46.439817635228,46.5230093824112,46.6061955420591,46.6894038089641,46.7722894221322,
46.8553557362354,46.9384085402281,47.0214499107393,47.1044938151874,47.1238898038469),
 .UNSPECIFIED.);
#177=B_SPLINE_CURVE_WITH_KNOTS('',3,(#7730,#7731,#7732,#7733,#7734,#7735,
#7736,#7737,#7738,#7739,#7740,#7741,#7742,#7743,#7744,#7745,#7746,#7747,
#7748,#7749,#7750,#7751,#7752,#7753,#7754,#7755,#7756,#7757,#7758,#7759,
#7760,#7761,#7762,#7763,#7764,#7765,#7766,#7767,#7768,#7769,#7770,#7771,
#7772,#7773,#7774,#7775,#7776,#7777,#7778,#7779,#7780,#7781,#7782,#7783,
#7784,#7785,#7786,#7787,#7788,#7789,#7790,#7791,#7792,#7793,#7794,#7795,
#7796,#7797,#7798,#7799,#7800,#7801,#7802,#7803,#7804,#7805,#7806,#7807,
#7808,#7809,#7810,#7811),.UNSPECIFIED.,.F.,.F.,(4,3,3,3,3,3,3,3,3,3,3,3,
3,3,3,3,3,3,3,3,3,3,3,3,3,3,3,4),(47.1238898039573,47.2105854036145,47.2711545043791,
47.3543592673762,47.4375477997221,47.5207395469052,47.603925706553,47.6871339734579,
47.770019586626,47.8532243496231,47.9364128819692,48.0196046291524,48.1027907888001,
48.1859990557052,48.2688846688728,48.3520894318698,48.4352779642157,48.5184697113989,
48.6016558710467,48.6848641379517,48.7677497511197,48.8509545141168,48.9341430464628,
49.017334793646,49.1005209532939,49.183729220199,49.2666148333666,49.3494924806201),
 .UNSPECIFIED.);
#178=B_SPLINE_CURVE_WITH_KNOTS('',3,(#7813,#7814,#7815,#7816,#7817,#7818,
#7819,#7820,#7821,#7822,#7823,#7824,#7825,#7826,#7827,#7828,#7829,#7830,
#7831,#7832,#7833,#7834,#7835,#7836,#7837,#7838,#7839,#7840,#7841,#7842,
#7843,#7844,#7845,#7846,#7847,#7848,#7849,#7850,#7851,#7852,#7853,#7854,
#7855,#7856,#7857,#7858,#7859,#7860,#7861,#7862,#7863,#7864,#7865,#7866,
#7867,#7868,#7869,#7870,#7871,#7872,#7873,#7874,#7875,#7876,#7877,#7878,
#7879,#7880,#7881,#7882,#7883,#7884,#7885,#7886,#7887,#7888,#7889,#7890,
#7891,#7892,#7893,#7894,#7895,#7896,#7897),.UNSPECIFIED.,.F.,.F.,(4,3,3,
3,3,3,3,3,3,3,3,3,3,3,3,3,3,3,3,3,3,3,3,3,3,3,3,3,4),(47.1238898039889,
47.2091197733778,47.2943777275482,47.3234955552657,47.4067003182626,47.4898888506086,
47.5730805977918,47.6562667574395,47.7394750243445,47.8223606375126,47.9055654005096,
47.9887539328555,48.0719456800387,48.1551318396864,48.2383401065915,48.3212257197594,
48.4044304827564,48.4876190151023,48.5708107622854,48.6539969219332,48.7372051888382,
48.8200908020063,48.9032955650034,48.9864840973494,49.0696758445326,49.1528620041804,
49.2360702710854,49.3189558842532,49.349485040032),.UNSPECIFIED.);
#179=B_SPLINE_CURVE_WITH_KNOTS('',3,(#7898,#7899,#7900,#7901,#7902,#7903,
#7904,#7905,#7906,#7907,#7908,#7909,#7910,#7911,#7912,#7913,#7914,#7915,
#7916,#7917,#7918,#7919,#7920,#7921,#7922,#7923,#7924,#7925,#7926,#7927,
#7928,#7929,#7930,#7931,#7932,#7933,#7934,#7935,#7936,#7937,#7938,#7939,
#7940,#7941,#7942,#7943,#7944,#7945,#7946,#7947,#7948,#7949,#7950,#7951,
#7952,#7953,#7954,#7955,#7956,#7957,#7958,#7959,#7960,#7961,#7962,#7963,
#7964,#7965,#7966,#7967,#7968,#7969,#7970,#7971,#7972,#7973,#7974,#7975,
#7976,#7977,#7978,#7979,#7980,#7981,#7982,#7983,#7984,#7985,#7986,#7987,
#7988,#7989,#7990,#7991,#7992,#7993,#7994,#7995,#7996,#7997,#7998,#7999,
#8000,#8001,#8002,#8003,#8004,#8005,#8006,#8007,#8008,#8009,#8010,#8011,
#8012,#8013,#8014,#8015,#8016,#8017,#8018,#8019,#8020,#8021,#8022,#8023,
#8024,#8025,#8026,#8027,#8028,#8029,#8030,#8031,#8032,#8033,#8034,#8035,
#8036,#8037,#8038,#8039,#8040,#8041,#8042,#8043,#8044,#8045,#8046,#8047,
#8048),.UNSPECIFIED.,.F.,.F.,(4,3,3,3,3,3,3,3,3,3,3,3,3,3,3,3,3,3,3,3,3,
3,3,3,3,3,3,3,3,3,3,3,3,3,3,3,3,3,3,3,3,3,3,3,3,3,3,3,3,3,4),(43.066293790228,
43.1494805290637,43.2326671870035,43.3158711701376,43.3325748972907,43.4157796602877,
43.4989681926337,43.5821599398169,43.6653460994647,43.7485543663697,43.8314399795375,
43.9146447425345,43.9978332748805,44.0810250220636,44.1642111817114,44.2474194486164,
44.3303050617844,44.4135098247815,44.4966983571275,44.5798901043107,44.6630762639585,
44.7462845308635,44.8291701440313,44.9123749070284,44.9955634393744,45.0787551865576,
45.1619413462055,45.2451496131105,45.3280352262782,45.4112399892752,45.4944285216212,
45.5776202688043,45.6608064284521,45.7440146953571,45.8269003085251,45.9101050715222,
45.993293603868,46.0764853510512,46.159671510699,46.242879777604,46.3257653907719,
46.4089701537688,46.4921586861147,46.5753504332978,46.6585365929456,46.7417448598505,
46.8246304730188,46.9081622099044,46.9916752427181,47.0751808263689,47.1238898038469),
 .UNSPECIFIED.);
#180=B_SPLINE_CURVE_WITH_KNOTS('',3,(#8054,#8055,#8056,#8057,#8058,#8059,
#8060,#8061,#8062,#8063,#8064,#8065,#8066),.UNSPECIFIED.,.F.,.F.,(4,1,1,
1,1,1,1,1,1,1,4),(36.7831013013255,36.7949877771947,37.2938528594415,37.7927179416884,
38.2915830239353,38.7904481061822,39.2893131884291,39.7881782706759,40.2870433529228,
40.7859084351697,40.8407044966673),.UNSPECIFIED.);
#181=B_SPLINE_CURVE_WITH_KNOTS('',3,(#8067,#8068,#8069,#8070,#8071,#8072,
#8073,#8074,#8075,#8076,#8077,#8078,#8079,#8080,#8081,#8082,#8083,#8084,
#8085,#8086,#8087,#8088,#8089,#8090,#8091,#8092,#8093,#8094,#8095,#8096,
#8097,#8098,#8099,#8100,#8101,#8102,#8103,#8104,#8105,#8106,#8107,#8108,
#8109,#8110,#8111,#8112,#8113,#8114,#8115,#8116,#8117,#8118,#8119,#8120,
#8121,#8122,#8123,#8124,#8125,#8126,#8127,#8128,#8129,#8130,#8131,#8132,
#8133,#8134,#8135,#8136,#8137,#8138,#8139,#8140,#8141,#8142,#8143,#8144,
#8145,#8146,#8147,#8148,#8149,#8150,#8151),.UNSPECIFIED.,.F.,.F.,(4,3,3,
3,3,3,3,3,3,3,3,3,3,3,3,3,3,3,3,3,3,3,3,3,3,3,3,3,4),(40.8407044966673,
40.9236082621666,41.0064970381205,41.0893890046342,41.1722791221436,41.255188027838,
41.2847735174166,41.3679782804136,41.4511668127597,41.5343585599429,41.6175447195908,
41.7007529864957,41.7836385996634,41.8668433626605,41.9500318950066,42.0332236421897,
42.1164098018374,42.1996180687424,42.2825036819103,42.3657084449074,42.4488969772536,
42.5320887244368,42.6152748840845,42.6984831509895,42.7813687641572,42.8645746921478,
42.9477630246613,43.0309462152979,43.0662846573068),.UNSPECIFIED.);
#182=B_SPLINE_CURVE_WITH_KNOTS('',3,(#8153,#8154,#8155,#8156,#8157,#8158,
#8159,#8160,#8161,#8162,#8163,#8164,#8165,#8166,#8167,#8168,#8169,#8170,
#8171,#8172,#8173,#8174,#8175,#8176,#8177,#8178,#8179,#8180,#8181,#8182,
#8183,#8184,#8185,#8186,#8187,#8188,#8189,#8190,#8191,#8192,#8193,#8194,
#8195,#8196,#8197,#8198,#8199,#8200,#8201,#8202,#8203,#8204,#8205,#8206,
#8207,#8208,#8209,#8210,#8211,#8212,#8213,#8214,#8215,#8216,#8217,#8218,
#8219,#8220,#8221,#8222,#8223,#8224,#8225,#8226,#8227,#8228,#8229,#8230,
#8231,#8232,#8233,#8234),.UNSPECIFIED.,.F.,.F.,(4,3,3,3,3,3,3,3,3,3,3,3,
3,3,3,3,3,3,3,3,3,3,3,3,3,3,3,4),(40.8407044966673,40.9238896807017,41.007058573913,
41.0902305668682,41.1733970921888,41.2565855470319,41.3371145683032,41.4203193313002,
41.5035078636461,41.5866996108293,41.6698857704772,41.7530940373822,41.83597965055,
41.9191844135471,42.002372945893,42.0855646930761,42.1687508527239,42.2519591196289,
42.3348447327969,42.418049495794,42.50123802814,42.5844297753232,42.6676159349711,
42.7508242018762,42.8337098150438,42.9169142021957,43.0001074756034,43.066293790228),
 .UNSPECIFIED.);
#183=B_SPLINE_CURVE_WITH_KNOTS('',3,(#8235,#8236,#8237,#8238,#8239,#8240,
#8241,#8242,#8243,#8244,#8245,#8246,#8247,#8248,#8249,#8250,#8251,#8252,
#8253,#8254,#8255,#8256,#8257,#8258,#8259,#8260,#8261,#8262,#8263,#8264,
#8265,#8266,#8267,#8268,#8269,#8270,#8271,#8272,#8273,#8274,#8275,#8276,
#8277,#8278,#8279,#8280,#8281,#8282,#8283,#8284,#8285,#8286,#8287,#8288,
#8289,#8290,#8291,#8292,#8293,#8294,#8295,#8296,#8297,#8298,#8299,#8300,
#8301,#8302,#8303,#8304,#8305,#8306,#8307,#8308,#8309,#8310,#8311,#8312,
#8313,#8314,#8315,#8316,#8317,#8318,#8319,#8320,#8321,#8322,#8323,#8324,
#8325,#8326,#8327,#8328,#8329,#8330,#8331,#8332,#8333,#8334,#8335,#8336,
#8337,#8338,#8339,#8340,#8341,#8342,#8343,#8344,#8345,#8346,#8347,#8348,
#8349,#8350,#8351,#8352,#8353,#8354,#8355,#8356,#8357,#8358,#8359,#8360,
#8361,#8362,#8363,#8364,#8365,#8366,#8367,#8368,#8369,#8370,#8371,#8372,
#8373,#8374,#8375,#8376,#8377,#8378,#8379,#8380,#8381,#8382,#8383,#8384,
#8385),.UNSPECIFIED.,.F.,.F.,(4,3,3,3,3,3,3,3,3,3,3,3,3,3,3,3,3,3,3,3,3,
3,3,3,3,3,3,3,3,3,3,3,3,3,3,3,3,3,3,3,3,3,3,3,3,3,3,3,3,3,4),(36.7830907836671,
36.8473288280813,36.9305335910781,37.0137221234244,37.0969138706075,37.1801000302554,
37.2633082971604,37.3461939103281,37.4293986733251,37.512587205671,37.595778952854,
37.6789651125019,37.762173379407,37.845058992575,37.928263755572,38.011452287918,
38.0946440351011,38.1778301947487,38.2610384616539,38.3439240748219,38.427128837819,
38.5103173701645,38.5935091173477,38.6766952769955,38.7599035439005,38.8427891570688,
38.9259939200658,39.009182452412,39.0923741995953,39.1755603592432,39.2587686261481,
39.3416542393157,39.4248590023125,39.5080475346586,39.5912392818417,39.6744254414893,
39.7576337083944,39.8405193215625,39.9237240845596,40.0069126169054,40.0901043640886,
40.1732905237363,40.2564987906412,40.3393844038094,40.4225891668065,40.5057776991523,
40.5889694463354,40.6721556059833,40.7553638728884,40.8382494860563,40.8407044963635),
 .UNSPECIFIED.);
#184=B_SPLINE_CURVE_WITH_KNOTS('',3,(#8391,#8392,#8393,#8394,#8395,#8396,
#8397,#8398,#8399,#8400,#8401,#8402,#8403,#8404,#8405,#8406,#8407,#8408,
#8409,#8410,#8411,#8412,#8413,#8414,#8415,#8416,#8417,#8418,#8419,#8420,
#8421,#8422,#8423,#8424,#8425,#8426,#8427,#8428,#8429,#8430,#8431,#8432,
#8433,#8434,#8435,#8436,#8437,#8438,#8439,#8440,#8441,#8442,#8443,#8444,
#8445,#8446,#8447,#8448,#8449,#8450,#8451,#8452,#8453,#8454,#8455,#8456,
#8457,#8458,#8459,#8460,#8461,#8462,#8463,#8464,#8465,#8466,#8467,#8468,
#8469,#8470,#8471,#8472,#8473,#8474,#8475,#8476,#8477,#8478,#8479,#8480,
#8481,#8482,#8483,#8484,#8485,#8486,#8487,#8488,#8489,#8490,#8491,#8492,
#8493,#8494,#8495,#8496,#8497,#8498,#8499,#8500,#8501,#8502,#8503,#8504,
#8505,#8506,#8507,#8508,#8509,#8510,#8511,#8512,#8513,#8514,#8515,#8516,
#8517,#8518,#8519,#8520,#8521,#8522,#8523,#8524,#8525,#8526,#8527,#8528,
#8529,#8530,#8531,#8532,#8533,#8534,#8535,#8536,#8537,#8538),
 .UNSPECIFIED.,.F.,.F.,(4,3,3,3,3,3,3,3,3,3,3,3,3,3,3,3,3,3,3,3,3,3,3,3,
3,3,3,3,3,3,3,3,3,3,3,3,3,3,3,3,3,3,3,3,3,3,3,3,3,4),(30.4999301101848,
30.5831195524751,30.6663053868848,30.7495113023812,30.8086067902321,30.8918115532291,
30.9750000855751,31.0581918327582,31.141377992406,31.224586259311,31.307471872479,
31.3906766354761,31.473865167822,31.5570569150052,31.6402430746531,31.7234513415581,
31.8063369547259,31.889541717723,31.972730250069,32.0559219972522,32.1391081569,
32.222316423805,32.3052020369728,32.3884067999698,32.4715953323158,32.5547870794989,
32.6379732391468,32.7211815060518,32.8040671192197,32.8872718822167,32.9704604145627,
33.0536521617459,33.1368383213936,33.2200465882987,33.3029322014665,33.3861369644635,
33.4693254968094,33.5525172439925,33.6357034036404,33.7189116705454,33.8017972837134,
33.8850020467105,33.9681905790564,34.0513823262396,34.1345684858875,34.2177767527926,
34.3006623659603,34.3847827412953,34.4711509653915,34.5575191894877),
 .UNSPECIFIED.);
#185=B_SPLINE_CURVE_WITH_KNOTS('',3,(#8539,#8540,#8541,#8542,#8543,#8544,
#8545,#8546),.UNSPECIFIED.,.F.,.F.,(4,1,1,1,1,4),(34.5575191949046,34.7995274482072,
35.298392530454,35.7972576127009,36.2961226949478,36.7831013013255),
 .UNSPECIFIED.);
#186=B_SPLINE_CURVE_WITH_KNOTS('',3,(#8548,#8549,#8550,#8551,#8552,#8553,
#8554,#8555,#8556,#8557,#8558,#8559,#8560,#8561,#8562,#8563,#8564,#8565,
#8566,#8567,#8568,#8569,#8570,#8571,#8572,#8573,#8574,#8575,#8576,#8577,
#8578,#8579,#8580,#8581,#8582,#8583,#8584,#8585,#8586,#8587,#8588,#8589,
#8590,#8591,#8592,#8593,#8594,#8595,#8596,#8597,#8598,#8599,#8600,#8601,
#8602,#8603,#8604,#8605,#8606,#8607,#8608,#8609,#8610,#8611,#8612,#8613,
#8614,#8615,#8616,#8617,#8618,#8619,#8620,#8621,#8622,#8623,#8624,#8625,
#8626,#8627,#8628,#8629,#8630,#8631,#8632),.UNSPECIFIED.,.F.,.F.,(4,3,3,
3,3,3,3,3,3,3,3,3,3,3,3,3,3,3,3,3,3,3,3,3,3,3,3,3,4),(34.5575191894877,
34.6410858833927,34.7246534185875,34.8082419415075,34.8518684990938,34.9350732620908,
35.0182617944371,35.1014535416203,35.1846397012681,35.2678479681731,35.3507335813406,
35.4339383443377,35.5171268766836,35.6003186238667,35.6835047835147,35.7667130504196,
35.8495986635875,35.9328034265846,36.0159919589303,36.0991837061135,36.1823698657615,
36.2655781326667,36.3484637458344,36.4316678909786,36.5148555434348,36.5980411279957,
36.6812216768781,36.7644129039734,36.7830907836671),.UNSPECIFIED.);
#187=B_SPLINE_CURVE_WITH_KNOTS('',3,(#8633,#8634,#8635,#8636,#8637,#8638,
#8639,#8640,#8641,#8642,#8643,#8644,#8645,#8646,#8647,#8648,#8649,#8650,
#8651,#8652,#8653,#8654,#8655,#8656,#8657,#8658,#8659,#8660,#8661,#8662,
#8663,#8664,#8665,#8666,#8667,#8668,#8669,#8670,#8671,#8672,#8673,#8674,
#8675,#8676,#8677,#8678,#8679,#8680,#8681,#8682,#8683,#8684,#8685,#8686,
#8687,#8688,#8689,#8690,#8691,#8692,#8693,#8694,#8695,#8696,#8697,#8698,
#8699,#8700,#8701,#8702,#8703,#8704,#8705,#8706,#8707,#8708,#8709,#8710,
#8711,#8712,#8713,#8714,#8715,#8716,#8717,#8718,#8719,#8720,#8721,#8722,
#8723,#8724,#8725,#8726,#8727,#8728,#8729,#8730,#8731,#8732,#8733,#8734,
#8735,#8736,#8737,#8738,#8739,#8740,#8741,#8742,#8743,#8744,#8745,#8746,
#8747,#8748,#8749,#8750,#8751,#8752,#8753,#8754,#8755,#8756,#8757,#8758,
#8759,#8760,#8761,#8762,#8763,#8764,#8765,#8766,#8767,#8768,#8769,#8770,
#8771,#8772,#8773,#8774,#8775,#8776,#8777,#8778,#8779,#8780,#8781,#8782,
#8783),.UNSPECIFIED.,.F.,.F.,(4,3,3,3,3,3,3,3,3,3,3,3,3,3,3,3,3,3,3,3,3,
3,3,3,3,3,3,3,3,3,3,3,3,3,3,3,3,3,3,3,3,3,3,3,3,3,3,3,3,3,4),(30.4999360201024,
30.5831176496859,30.6663049468445,30.7494912023174,30.8326954253169,30.8609478411187,
30.9441526041158,31.0273411364619,31.1105328836451,31.193719043293,31.2769273101981,
31.3598129233656,31.4430176863626,31.5262062187086,31.6093979658918,31.6925841255396,
31.7757923924446,31.8586780056125,31.9418827686095,32.0250713009555,32.1082630481386,
32.1914492077864,32.2746574746914,32.3575430878594,32.4407478508565,32.5239363832024,
32.6071281303855,32.6903142900333,32.7735225569383,32.8564081701062,32.9396129331032,
33.0228014654491,33.1059932126322,33.1891793722801,33.272387639185,33.3552732523531,
33.4384780153501,33.5216665476963,33.6048582948794,33.6880444545274,33.7712527214324,
33.8541383346,33.937343097597,34.0205316299431,34.1037233771263,34.1869095367742,
34.2701178036792,34.3530034168469,34.4381472840239,34.5232671972151,34.5575191893576),
 .UNSPECIFIED.);
#188=B_SPLINE_CURVE_WITH_KNOTS('',3,(#8789,#8790,#8791,#8792,#8793,#8794,
#8795,#8796,#8797,#8798,#8799,#8800,#8801,#8802,#8803,#8804,#8805,#8806,
#8807,#8808,#8809,#8810,#8811,#8812,#8813,#8814,#8815,#8816,#8817,#8818,
#8819,#8820,#8821,#8822,#8823,#8824,#8825,#8826,#8827,#8828,#8829,#8830,
#8831,#8832,#8833,#8834,#8835,#8836,#8837,#8838,#8839,#8840,#8841,#8842,
#8843,#8844,#8845,#8846,#8847,#8848,#8849,#8850,#8851,#8852,#8853,#8854,
#8855,#8856,#8857,#8858,#8859,#8860,#8861,#8862,#8863,#8864,#8865,#8866,
#8867,#8868,#8869,#8870,#8871,#8872,#8873,#8874,#8875,#8876,#8877,#8878,
#8879,#8880,#8881,#8882,#8883,#8884,#8885,#8886,#8887,#8888,#8889,#8890,
#8891,#8892,#8893,#8894,#8895,#8896,#8897,#8898,#8899,#8900,#8901,#8902,
#8903,#8904,#8905,#8906,#8907,#8908,#8909,#8910,#8911,#8912,#8913,#8914,
#8915,#8916,#8917,#8918,#8919,#8920,#8921,#8922,#8923,#8924,#8925,#8926,
#8927,#8928,#8929,#8930,#8931,#8932,#8933,#8934,#8935,#8936,#8937,#8938,
#8939),.UNSPECIFIED.,.F.,.F.,(4,3,3,3,3,3,3,3,3,3,3,3,3,3,3,3,3,3,3,3,3,
3,3,3,3,3,3,3,3,3,3,3,3,3,3,3,3,3,3,3,3,3,3,3,3,3,3,3,3,3,4),(24.216717884951,
24.299921981893,24.3233607210227,24.4065654840083,24.4897540163421,24.5729457635133,
24.656131923149,24.7393401900419,24.8222258032696,24.905430566277,24.9886190986334,
25.0718108458273,25.1549970054856,25.2382052724013,25.3210908855165,25.4042956485073,
25.4874841808471,25.5706759280239,25.6538620876651,25.7370703545637,25.8199559677634,
25.9031607307635,25.9863492631122,26.0695410102983,26.1527271699493,26.2359354368573,
26.3188210500103,26.4020258130063,26.4852143453511,26.5684060925334,26.6515922521803,
26.7348005190843,26.8176861322571,26.9008908952543,26.9840794276,27.0672711747833,
27.150457334431,27.2336656013361,27.316551214504,27.3997559775011,27.4829445098478,
27.5661362570311,27.649322416679,27.7325306835841,27.8154162967509,27.8983765004895,
27.9813196738763,28.0642637478914,28.1472037199699,28.2301616567405,28.2743338821564),
 .UNSPECIFIED.);
#189=B_SPLINE_CURVE_WITH_KNOTS('',3,(#8940,#8941,#8942,#8943,#8944,#8945,
#8946,#8947,#8948,#8949,#8950,#8951,#8952,#8953,#8954,#8955,#8956,#8957,
#8958,#8959,#8960,#8961,#8962,#8963,#8964,#8965,#8966,#8967,#8968,#8969,
#8970,#8971,#8972,#8973,#8974,#8975,#8976,#8977,#8978,#8979,#8980,#8981,
#8982,#8983,#8984,#8985,#8986,#8987,#8988,#8989,#8990,#8991,#8992,#8993,
#8994,#8995,#8996,#8997,#8998,#8999,#9000,#9001,#9002,#9003,#9004,#9005,
#9006,#9007,#9008,#9009,#9010,#9011,#9012,#9013,#9014,#9015,#9016,#9017,
#9018,#9019,#9020,#9021,#9022,#9023,#9024),.UNSPECIFIED.,.F.,.F.,(4,3,3,
3,3,3,3,3,3,3,3,3,3,3,3,3,3,3,3,3,3,3,3,3,3,3,3,3,4),(28.2743338823081,
28.3142813789978,28.397486141995,28.4806746743415,28.5638664215248,28.6470525811728,
28.730260848078,28.8131464612446,28.8963512242415,28.9795397565875,29.0627315037705,
29.1459176634183,29.2291259303233,29.3120115434915,29.3952163064886,29.4784048388345,
29.5615965860178,29.6447827456656,29.7279910125707,29.8108766257384,29.8940813887354,
29.9772699210814,30.0604616682645,30.1436478279123,30.2268560948173,30.3097417079853,
30.3929456544943,30.4761344023573,30.4999301101848),.UNSPECIFIED.);
#190=B_SPLINE_CURVE_WITH_KNOTS('',3,(#9026,#9027,#9028,#9029,#9030,#9031,
#9032,#9033,#9034,#9035,#9036,#9037,#9038,#9039,#9040,#9041,#9042,#9043,
#9044,#9045,#9046,#9047,#9048,#9049,#9050,#9051,#9052,#9053,#9054,#9055,
#9056,#9057,#9058,#9059,#9060,#9061,#9062,#9063,#9064,#9065,#9066,#9067,
#9068,#9069,#9070,#9071,#9072,#9073,#9074,#9075,#9076,#9077,#9078,#9079,
#9080,#9081,#9082,#9083,#9084,#9085,#9086,#9087,#9088,#9089,#9090,#9091,
#9092,#9093,#9094,#9095,#9096,#9097,#9098,#9099,#9100,#9101,#9102,#9103,
#9104,#9105,#9106,#9107),.UNSPECIFIED.,.F.,.F.,(4,3,3,3,3,3,3,3,3,3,3,3,
3,3,3,3,3,3,3,3,3,3,3,3,3,3,3,4),(28.2743338823081,28.3666224298844,28.4498271928843,
28.5330157252333,28.6162074724194,28.6993936320702,28.7826018989782,28.8654875121312,
28.9486922751272,29.0318808074722,29.1150725546544,29.1982587143012,29.2814669812052,
29.3643525943781,29.4475573573753,29.5307458897214,29.6139376369048,29.6971237965528,
29.780332063458,29.863217676625,29.9464224396222,30.0296109719682,30.1128027191515,
30.1959888787995,30.2791971457046,30.3620827588719,30.4452883358325,30.4999360201024),
 .UNSPECIFIED.);
#191=B_SPLINE_CURVE_WITH_KNOTS('',3,(#9108,#9109,#9110,#9111,#9112,#9113,
#9114,#9115,#9116,#9117,#9118,#9119,#9120,#9121,#9122,#9123,#9124,#9125,
#9126,#9127,#9128,#9129,#9130,#9131,#9132,#9133,#9134,#9135,#9136,#9137,
#9138,#9139,#9140,#9141,#9142,#9143,#9144,#9145,#9146,#9147,#9148,#9149,
#9150,#9151,#9152,#9153,#9154,#9155,#9156,#9157,#9158,#9159,#9160,#9161,
#9162,#9163,#9164,#9165,#9166,#9167,#9168,#9169,#9170,#9171,#9172,#9173,
#9174,#9175,#9176,#9177,#9178,#9179,#9180,#9181,#9182,#9183,#9184,#9185,
#9186,#9187,#9188,#9189,#9190,#9191,#9192,#9193,#9194,#9195,#9196,#9197,
#9198,#9199,#9200,#9201,#9202,#9203,#9204,#9205,#9206,#9207,#9208,#9209,
#9210,#9211,#9212,#9213,#9214,#9215,#9216,#9217,#9218,#9219,#9220,#9221,
#9222,#9223,#9224,#9225,#9226,#9227,#9228,#9229,#9230,#9231,#9232,#9233,
#9234,#9235,#9236,#9237,#9238,#9239,#9240,#9241,#9242,#9243,#9244,#9245,
#9246,#9247,#9248,#9249,#9250,#9251,#9252,#9253,#9254,#9255),
 .UNSPECIFIED.,.F.,.F.,(4,3,3,3,3,3,3,3,3,3,3,3,3,3,3,3,3,3,3,3,3,3,3,3,
3,3,3,3,3,3,3,3,3,3,3,3,3,3,3,3,3,3,3,3,3,3,3,3,3,4),(24.2167209753283,
24.2999284446391,24.3757017719093,24.4589065342714,24.5420950659734,24.6252868125053,
24.7084729714987,24.791681237751,24.8745668541562,24.9577716175062,25.0409601502098,
25.1241518977543,25.2073380577647,25.2905463250312,25.3734319364031,25.4566366992492,
25.5398252314424,25.6230169784713,25.7062031379642,25.7894114047152,25.87229701865,
25.9555017816906,26.0386903140807,26.1218820613081,26.2050682210001,26.2882764879492,
26.3711621008968,26.4543668638941,26.5375553962401,26.6207471434236,26.7039333030718,
26.7871415699773,26.8700271831437,26.953231946129,27.0364204784631,27.1196122256344,
27.2027983852704,27.2860066521636,27.3688922653906,27.452097028398,27.5352855607541,
27.618477307948,27.7016634676065,27.7848717345221,27.8677573476375,27.950630740422,
28.0334950107661,28.116348080326,28.1992149244415,28.2743338821488),
 .UNSPECIFIED.);
#192=B_SPLINE_CURVE_WITH_KNOTS('',3,(#9261,#9262,#9263,#9264,#9265,#9266,
#9267,#9268,#9269),.UNSPECIFIED.,.F.,.F.,(4,1,1,1,1,1,4),(15.7079632679489,
15.8949953737124,16.3938604559593,16.8927255382062,17.3915906204531,17.8904557026999,
17.9335636647299),.UNSPECIFIED.);
#193=B_SPLINE_CURVE_WITH_KNOTS('',3,(#9271,#9272,#9273,#9274,#9275,#9276),
 .UNSPECIFIED.,.F.,.F.,(4,1,1,4),(14.3984001269718,14.8972652092187,15.3961302914656,
15.7079632679489),.UNSPECIFIED.);
#194=B_SPLINE_CURVE_WITH_KNOTS('',3,(#9280,#9281,#9282,#9283,#9284,#9285,
#9286,#9287,#9288,#9289,#9290,#9291,#9292,#9293,#9294,#9295,#9296,#9297,
#9298,#9299,#9300,#9301,#9302,#9303,#9304,#9305,#9306,#9307,#9308,#9309,
#9310,#9311,#9312,#9313,#9314,#9315,#9316,#9317,#9318,#9319,#9320,#9321,
#9322,#9323,#9324,#9325,#9326,#9327,#9328,#9329,#9330,#9331,#9332,#9333,
#9334,#9335,#9336,#9337,#9338,#9339,#9340,#9341,#9342,#9343,#9344,#9345,
#9346,#9347,#9348,#9349),.UNSPECIFIED.,.F.,.F.,(4,3,3,3,3,3,3,3,3,3,3,3,
3,3,3,3,3,3,3,3,3,3,3,4),(13.8759337553362,13.9589611884219,14.0419725517034,
14.1249865839979,14.2079967440506,14.2910269801202,14.3460590760852,14.4292629924508,
14.51245069532,14.5956416479347,14.6788270336895,14.7620345691255,14.8449241583321,
14.9281250993385,15.0113097465424,15.0944975472168,15.1776797345729,15.2608840240016,
15.343789240579,15.4267884627978,15.5097751925943,15.592750663241,15.6757311232471,
15.7079632679489),.UNSPECIFIED.);
#195=B_SPLINE_CURVE_WITH_KNOTS('',3,(#9350,#9351,#9352,#9353,#9354,#9355,
#9356,#9357,#9358,#9359,#9360,#9361,#9362,#9363,#9364,#9365,#9366,#9367,
#9368,#9369,#9370,#9371,#9372,#9373,#9374,#9375,#9376,#9377,#9378,#9379,
#9380,#9381,#9382,#9383,#9384,#9385,#9386,#9387,#9388,#9389,#9390,#9391,
#9392,#9393,#9394,#9395,#9396,#9397,#9398,#9399,#9400,#9401,#9402,#9403,
#9404,#9405,#9406,#9407,#9408,#9409,#9410,#9411,#9412,#9413,#9414,#9415,
#9416,#9417,#9418,#9419,#9420,#9421,#9422,#9423,#9424,#9425,#9426,#9427,
#9428,#9429,#9430,#9431,#9432,#9433,#9434),.UNSPECIFIED.,.F.,.F.,(4,3,3,
3,3,3,3,3,3,3,3,3,3,3,3,3,3,3,3,3,3,3,3,3,3,3,3,3,4),(15.7079632680893,
15.7950775824961,15.8426543228258,15.9258568205529,16.0090430574305,16.0922324840386,
16.1754163139598,16.2586222581903,16.3415194050727,16.4247252502413,16.5079148782708,
16.5911077317026,16.6742950011921,16.7575043732806,16.8403844873196,16.9235888701302,
17.0067770180441,17.0899683778634,17.1731541493092,17.2563620303484,17.3392495695665,
17.4224543918057,17.5056429836855,17.5888347902833,17.672021009163,17.7552293344183,
17.8381146518133,17.921318645311,17.9335664739021),.UNSPECIFIED.);
#196=B_SPLINE_CURVE_WITH_KNOTS('',3,(#9440,#9441,#9442,#9443,#9444,#9445,
#9446,#9447,#9448,#9449,#9450,#9451,#9452,#9453,#9454,#9455,#9456,#9457,
#9458,#9459,#9460,#9461,#9462,#9463,#9464,#9465,#9466,#9467,#9468,#9469,
#9470,#9471,#9472,#9473,#9474,#9475,#9476,#9477,#9478,#9479,#9480,#9481,
#9482,#9483,#9484,#9485,#9486,#9487,#9488,#9489,#9490,#9491,#9492,#9493,
#9494,#9495,#9496,#9497,#9498,#9499,#9500,#9501,#9502,#9503,#9504,#9505,
#9506,#9507),.UNSPECIFIED.,.F.,.F.,(4,2,2,2,2,2,2,2,2,2,2,2,2,2,2,2,2,2,
2,2,2,2,2,2,2,2,2,2,2,2,2,2,2,4),(3.21211487024883E-5,0.0789352746093392,
0.125900885216109,0.194687536519382,0.235964866096197,0.260949154170126,
0.318423911537595,0.387900638259459,0.463726389496267,0.514560383592697,
0.580602031721947,0.645219715092042,0.720385217165228,0.769263684680726,
0.826314664490939,0.892514875423717,0.99193614383231,1.0300811327044,1.08495853522793,
1.15083401376278,1.24505839048266,1.2860599861693,1.34209173725548,1.4085307353683,
1.49904769502063,1.54210420930418,1.6033802411766,1.67075334491485,1.74659608796949,
1.79662732553455,1.85318325250244,1.92072567690366,2.01576766849767,2.0528946271821),
 .UNSPECIFIED.);
#197=B_SPLINE_CURVE_WITH_KNOTS('',3,(#9510,#9511,#9512,#9513,#9514,#9515,
#9516,#9517,#9518,#9519,#9520,#9521,#9522,#9523,#9524,#9525,#9526,#9527,
#9528,#9529,#9530,#9531,#9532,#9533,#9534,#9535,#9536,#9537,#9538,#9539,
#9540,#9541,#9542,#9543,#9544,#9545,#9546,#9547,#9548,#9549,#9550,#9551,
#9552,#9553,#9554,#9555,#9556,#9557,#9558,#9559,#9560,#9561,#9562,#9563,
#9564,#9565,#9566,#9567,#9568,#9569,#9570,#9571,#9572,#9573,#9574,#9575,
#9576,#9577,#9578,#9579,#9580,#9581,#9582,#9583,#9584,#9585,#9586,#9587,
#9588,#9589,#9590,#9591,#9592,#9593,#9594,#9595,#9596,#9597,#9598,#9599,
#9600,#9601,#9602,#9603,#9604,#9605,#9606,#9607),.UNSPECIFIED.,.F.,.F.,
(4,2,2,2,2,2,2,2,2,2,2,2,2,2,2,2,2,2,2,2,2,2,2,2,2,2,2,2,2,2,2,2,2,2,2,
2,2,2,2,2,2,2,2,2,2,2,2,2,4),(-5.86775810127551,-5.77865085129505,-5.72879583160343,
-5.64761852141392,-5.61689286788677,-5.54175378043255,-5.49593445407308,
-5.4210022791591,-5.36917519324587,-5.32999908682785,-5.26057884393074,
-5.20983829062336,-5.11311910543699,-5.05694894394058,-4.98922760967673,
-4.89378617981899,-4.85349774549445,-4.79705316735085,-4.73079766409471,
-4.6414271299511,-4.59765033110434,-4.53624621476361,-4.46895286460035,
-4.39375558925325,-4.3422088475698,-4.2887681416752,-4.21895559732193,-4.12372343019229,
-4.08333396673305,-4.02676275422254,-3.96056758056503,-3.87140429745958,
-3.8274912977314,-3.7659411752726,-3.69875702039177,-3.6270581440989,-3.57197264493549,
-3.51871698633678,-3.48379939085449,-3.45946983959537,-3.40770778211876,
-3.31627953506947,-3.25897883939447,-3.19263751159846,-3.09559065383727,
-3.05613493947002,-3.00105661676876,-2.93406942190934,-2.93406320703471),
 .UNSPECIFIED.);
#198=B_SPLINE_CURVE_WITH_KNOTS('',3,(#9613,#9614,#9615,#9616,#9617,#9618,
#9619,#9620,#9621,#9622,#9623,#9624,#9625,#9626,#9627,#9628,#9629,#9630,
#9631,#9632,#9633,#9634,#9635,#9636,#9637),.UNSPECIFIED.,.F.,.F.,(4,3,3,
3,3,3,3,3,4),(63.5596986986593,63.6465864533654,63.7334716784127,63.8203763732837,
63.8547305276003,63.9421373160612,64.0295237721704,64.116898968737,64.141416212773),
 .UNSPECIFIED.);
#199=B_SPLINE_CURVE_WITH_KNOTS('',3,(#9638,#9639,#9640,#9641,#9642,#9643,
#9644,#9645,#9646,#9647,#9648,#9649,#9650,#9651,#9652,#9653,#9654,#9655,
#9656,#9657,#9658,#9659,#9660,#9661,#9662,#9663,#9664,#9665,#9666,#9667,
#9668,#9669,#9670,#9671,#9672,#9673,#9674,#9675,#9676,#9677,#9678,#9679,
#9680,#9681,#9682,#9683,#9684,#9685,#9686,#9687,#9688,#9689,#9690,#9691,
#9692,#9693,#9694,#9695,#9696,#9697,#9698,#9699,#9700,#9701,#9702,#9703,
#9704,#9705,#9706,#9707,#9708,#9709,#9710,#9711,#9712,#9713,#9714,#9715,
#9716,#9717,#9718,#9719,#9720,#9721,#9722,#9723,#9724,#9725,#9726,#9727,
#9728,#9729,#9730,#9731,#9732,#9733,#9734,#9735,#9736,#9737),
 .UNSPECIFIED.,.F.,.F.,(4,2,2,2,2,2,2,2,2,2,2,2,2,2,2,2,2,2,2,2,2,2,2,2,
2,2,2,2,2,2,2,2,2,2,2,2,2,2,2,2,2,2,2,2,2,2,2,2,2,4),(2.0528946271821,2.05626576241009,
2.11302674968695,2.1830480906073,2.26413783199407,2.31157823672075,2.38070629598805,
2.44266215948112,2.49346033978971,2.56725647762745,2.61934692210331,2.69359183141892,
2.76083907262114,2.82229340458244,2.86610520161253,2.95542529828825,3.02169497932261,
3.07812176742366,3.11844011147168,3.2138055265495,3.27997468806069,3.33443328707101,
3.37351131970449,3.47132296969718,3.53831306246984,3.594430509328,3.64658886723371,
3.72050260660357,3.78778092905754,3.84919614272541,3.89300151309997,3.98233280802618,
4.04860055488936,4.10503243207252,4.14534577607919,4.24072351997691,4.3105533054657,
4.36390165735659,4.41591933462917,4.49067966246195,4.55794899396488,4.61937890270551,
4.6439987187184,4.69174215466658,4.75022353405068,4.79591121803213,4.84141672820665,
4.87360389107397,4.8998465902543,4.9868883946957),.UNSPECIFIED.);
#200=B_SPLINE_CURVE_WITH_KNOTS('',3,(#9739,#9740,#9741,#9742,#9743,#9744,
#9745,#9746,#9747,#9748,#9749,#9750,#9751,#9752,#9753,#9754,#9755,#9756,
#9757,#9758,#9759,#9760,#9761,#9762,#9763,#9764,#9765,#9766,#9767,#9768,
#9769,#9770,#9771,#9772,#9773,#9774,#9775,#9776,#9777,#9778,#9779,#9780,
#9781,#9782,#9783,#9784,#9785,#9786,#9787,#9788,#9789,#9790,#9791,#9792,
#9793,#9794,#9795,#9796,#9797,#9798,#9799,#9800,#9801,#9802,#9803,#9804,
#9805,#9806,#9807,#9808,#9809,#9810,#9811,#9812,#9813,#9814,#9815,#9816,
#9817,#9818,#9819,#9820,#9821,#9822,#9823,#9824,#9825,#9826,#9827,#9828,
#9829,#9830,#9831,#9832,#9833,#9834,#9835,#9836,#9837,#9838),
 .UNSPECIFIED.,.F.,.F.,(4,2,2,2,2,2,2,2,2,2,2,2,2,2,2,2,2,2,2,2,2,2,2,2,
2,2,2,2,2,2,2,2,2,2,2,2,2,2,2,2,2,2,2,2,2,2,2,2,2,4),(-2.93406320703471,
-2.87143399520746,-2.80165066855307,-2.78957633910132,-2.71955698375995,
-2.66455054203141,-2.64104511916306,-2.58128673311468,-2.54612054414229,
-2.49425519550508,-2.41918658143175,-2.35194063334941,-2.29048684232513,
-2.24665291139098,-2.15736466716485,-2.09112088683949,-2.03465266774453,
-1.99431292889813,-1.89898389290717,-1.83330110908048,-1.77821193978767,
-1.73874744368731,-1.64171364265346,-1.57537757862754,-1.51806752718927,
-1.42663305972774,-1.37487191786161,-1.35054239140323,-1.31562238273091,
-1.2623809917774,-1.20733488400603,-1.13558991658024,-1.06839518968176,
-1.0068654029055,-0.962977971966592,-0.873771092672304,-0.807566317326094,
-0.751021334432702,-0.710631251450796,-0.615394224793618,-0.547614894728043,
-0.491462320766733,-0.439215915126281,-0.365393474686328,-0.31952736516029,
-0.244028081793439,-0.213798227303348,-0.122271307731145,-0.0727085983661,
-4.44326005386446E-5),.UNSPECIFIED.);
#201=B_SPLINE_CURVE_WITH_KNOTS('',3,(#9839,#9840,#9841,#9842,#9843,#9844),
 .UNSPECIFIED.,.F.,.F.,(4,1,1,4),(-60.4048973677144,-60.3626749518721,-59.8638098696252,
-59.8231584322936),.UNSPECIFIED.);
#202=B_SPLINE_CURVE_WITH_KNOTS('',3,(#9850,#9851,#9852,#9853,#9854),
 .UNSPECIFIED.,.F.,.F.,(4,1,4),(57.2764810726534,57.3694844583909,57.8582308908959),
 .UNSPECIFIED.);
#203=B_SPLINE_CURVE_WITH_KNOTS('',3,(#9855,#9856,#9857,#9858,#9859,#9860,
#9861,#9862,#9863,#9864,#9865,#9866,#9867,#9868,#9869,#9870,#9871,#9872,
#9873,#9874,#9875,#9876,#9877,#9878,#9879,#9880,#9881,#9882,#9883,#9884,
#9885,#9886,#9887,#9888,#9889,#9890,#9891,#9892,#9893,#9894,#9895,#9896,
#9897,#9898,#9899,#9900,#9901,#9902,#9903,#9904,#9905,#9906,#9907,#9908,
#9909,#9910,#9911,#9912,#9913,#9914,#9915,#9916,#9917,#9918,#9919,#9920,
#9921,#9922,#9923,#9924,#9925,#9926,#9927,#9928,#9929,#9930,#9931,#9932,
#9933,#9934,#9935,#9936,#9937,#9938,#9939,#9940,#9941,#9942,#9943,#9944,
#9945,#9946,#9947,#9948,#9949,#9950,#9951,#9952,#9953,#9954,#9955,#9956,
#9957,#9958,#9959,#9960,#9961,#9962,#9963,#9964,#9965,#9966,#9967,#9968,
#9969,#9970,#9971,#9972,#9973,#9974,#9975,#9976,#9977,#9978,#9979,#9980,
#9981,#9982,#9983,#9984,#9985,#9986,#9987,#9988,#9989,#9990,#9991,#9992,
#9993,#9994,#9995,#9996,#9997,#9998,#9999,#10000,#10001,#10002,#10003,#10004,
#10005,#10006,#10007,#10008,#10009,#10010,#10011,#10012,#10013,#10014,#10015,
#10016,#10017,#10018,#10019,#10020,#10021,#10022,#10023,#10024,#10025,#10026,
#10027,#10028,#10029,#10030,#10031,#10032,#10033,#10034,#10035,#10036,#10037,
#10038,#10039,#10040,#10041,#10042,#10043,#10044,#10045,#10046,#10047,#10048,
#10049,#10050,#10051,#10052,#10053,#10054,#10055,#10056,#10057,#10058,#10059,
#10060,#10061,#10062,#10063,#10064,#10065),.UNSPECIFIED.,.F.,.F.,(4,3,3,
3,3,3,3,3,3,3,3,3,3,3,3,3,3,3,3,3,3,3,3,3,3,3,3,3,3,3,3,3,3,3,3,3,3,3,3,
3,3,3,3,3,3,3,3,3,3,3,3,3,3,3,3,3,3,3,3,3,3,3,3,3,3,3,3,3,3,3,4),(57.8582309055934,
57.8683495406378,57.9552544117093,58.042141744008,58.1290322085361,58.2159174169424,
58.302824308488,58.3672146228846,58.4541194939581,58.5410068262592,58.6278972907892,
58.7147824991975,58.8016893907451,58.8660797051315,58.9529845762033,59.0398719085024,
59.1267623730308,59.2136475814373,59.3005544729832,59.3649447873784,59.4518496584542,
59.5387369907573,59.6256274552896,59.7125126637,59.7994195552498,59.8638098696252,
59.9507147406915,60.0376020729851,60.124492537508,60.2113777459091,60.2982846374498,
60.3626749518721,60.4495798229561,60.5364671552673,60.6233576198078,60.7102428282263,
60.7971497197841,60.861540034119,60.9484449051794,61.0353322374671,61.1222227019841,
61.2091079103795,61.2960148019144,61.3604051163659,61.4473099874394,61.53419731974,
61.6210877842698,61.7079729926777,61.7948798842248,61.8592701986127,61.9461750697315,
62.0330624020779,62.1199528666535,62.2068380751072,62.2937449666998,62.3581352808596,
62.4450401517717,62.5319274839105,62.6188179482788,62.7057031565261,62.7926100479151,
62.8570003631065,62.9439052345569,63.0307925672361,63.1176830321429,63.204568240926,
63.2914751328423,63.3558654453534,63.4427695286802,63.5296580199759,63.5596986986593),
 .UNSPECIFIED.);
#204=B_SPLINE_CURVE_WITH_KNOTS('',3,(#10067,#10068,#10069,#10070,#10071,
#10072,#10073,#10074,#10075,#10076,#10077,#10078,#10079,#10080,#10081),
 .UNSPECIFIED.,.F.,.F.,(4,1,1,1,1,1,1,1,1,1,1,1,4),(-59.8231584322936,-59.3649447873784,
-58.8660797051315,-58.3672146228846,-57.8683495406377,-57.3694844583909,
-56.870619376144,-56.3717542938971,-55.8728892116502,-55.3740241294033,
-54.8751590471565,-54.3762939649096,-54.1217120605348),.UNSPECIFIED.);
#205=B_SPLINE_CURVE_WITH_KNOTS('',3,(#10082,#10083,#10084,#10085,#10086,
#10087,#10088,#10089,#10090,#10091,#10092,#10093,#10094,#10095,#10096,#10097,
#10098,#10099,#10100,#10101,#10102,#10103),.UNSPECIFIED.,.F.,.F.,(4,3,3,
3,3,3,3,4),(-54.1217120605348,-54.03365517902,-53.9455686638589,-53.8774288826627,
-53.7905200232061,-53.7036306829589,-53.6167399703894,-53.5400003888938),
 .UNSPECIFIED.);
#206=B_SPLINE_CURVE_WITH_KNOTS('',3,(#10109,#10110,#10111,#10112,#10113,
#10114,#10115,#10116,#10117,#10118,#10119,#10120,#10121,#10122,#10123,#10124,
#10125,#10126,#10127,#10128,#10129,#10130,#10131,#10132,#10133),
 .UNSPECIFIED.,.F.,.F.,(4,3,3,3,3,3,3,3,4),(50.9933372706279,51.0802213852619,
51.1671097576151,51.253994887845,51.3409000108923,51.3831034714283,51.4723469196116,
51.561562638303,51.5750455984138),.UNSPECIFIED.);
#207=B_SPLINE_CURVE_WITH_KNOTS('',3,(#10134,#10135,#10136,#10137,#10138,
#10139,#10140,#10141,#10142,#10143,#10144,#10145,#10146,#10147,#10148),
 .UNSPECIFIED.,.F.,.F.,(4,1,1,1,1,1,1,1,1,1,1,1,4),(51.5750455984138,51.8819685536752,
52.3808336359221,52.879698718169,53.3785638004159,53.8774288826627,54.3762939649096,
54.8751590471565,55.3740241294034,55.8728892116502,56.3717542938971,56.870619376144,
57.2764810726534),.UNSPECIFIED.);
#208=B_SPLINE_CURVE_WITH_KNOTS('',3,(#10150,#10151,#10152,#10153,#10154,
#10155,#10156,#10157,#10158,#10159,#10160,#10161,#10162,#10163,#10164,#10165,
#10166,#10167,#10168,#10169,#10170,#10171,#10172,#10173,#10174,#10175,#10176,
#10177,#10178,#10179,#10180,#10181,#10182,#10183,#10184,#10185,#10186,#10187,
#10188,#10189,#10190,#10191,#10192,#10193,#10194,#10195,#10196,#10197,#10198,
#10199,#10200,#10201,#10202,#10203,#10204,#10205,#10206,#10207,#10208,#10209,
#10210,#10211,#10212,#10213,#10214,#10215,#10216,#10217,#10218,#10219,#10220,
#10221,#10222,#10223,#10224,#10225,#10226,#10227,#10228,#10229,#10230,#10231,
#10232,#10233,#10234,#10235,#10236,#10237,#10238,#10239,#10240,#10241,#10242,
#10243,#10244,#10245,#10246,#10247,#10248,#10249,#10250,#10251,#10252,#10253,
#10254,#10255,#10256,#10257,#10258,#10259,#10260,#10261,#10262,#10263,#10264,
#10265,#10266,#10267,#10268,#10269,#10270,#10271,#10272,#10273,#10274,#10275,
#10276,#10277,#10278,#10279,#10280,#10281,#10282,#10283,#10284,#10285,#10286,
#10287,#10288,#10289,#10290,#10291,#10292,#10293,#10294,#10295,#10296,#10297,
#10298,#10299,#10300,#10301,#10302,#10303,#10304,#10305,#10306,#10307,#10308,
#10309,#10310,#10311,#10312,#10313,#10314,#10315,#10316,#10317,#10318,#10319,
#10320,#10321,#10322,#10323,#10324,#10325,#10326,#10327,#10328,#10329,#10330,
#10331,#10332,#10333,#10334,#10335,#10336,#10337,#10338,#10339,#10340,#10341,
#10342,#10343,#10344,#10345,#10346,#10347,#10348,#10349,#10350,#10351,#10352,
#10353,#10354,#10355,#10356,#10357),.UNSPECIFIED.,.F.,.F.,(4,3,3,3,3,3,
3,3,3,3,3,3,3,3,3,3,3,3,3,3,3,3,3,3,3,3,3,3,3,3,3,3,3,3,3,3,3,3,3,3,3,3,
3,3,3,3,3,3,3,3,3,3,3,3,3,3,3,3,3,3,3,3,3,3,3,3,3,3,3,4),(-53.5400003888938,
-53.4530924137426,-53.3785638004158,-53.2916589293431,-53.2047715970428,
-53.1178811325135,-53.0309959241062,-52.9440890325594,-52.879698718169,
-52.7927938470961,-52.7059065147958,-52.6190160502663,-52.5321308418588,
-52.4452239503118,-52.3808336359221,-52.2939287648492,-52.2070414325489,
-52.1201509680195,-52.0332657596117,-51.9463588680647,-51.8819685536752,
-51.7950636826023,-51.708176350302,-51.6212858857725,-51.5344006773649,
-51.4474937858178,-51.3831034714283,-51.2961986003556,-51.2093112680556,
-51.1224208035263,-51.0355355951188,-50.948628703572,-50.8842383891815,
-50.7973335181086,-50.7104461858084,-50.6235557212789,-50.5366705128713,
-50.4497636213243,-50.3853733069346,-50.2984684358617,-50.2115811035614,
-50.124690639032,-50.0378054306243,-49.9508985390773,-49.8865082246877,
-49.7996033536149,-49.7127160213146,-49.6258255567852,-49.5389403483777,
-49.4520334568307,-49.3876431424408,-49.3007382713678,-49.2138509390675,
-49.126960474538,-49.0400752661303,-48.9531683745832,-48.8887780601939,
-48.8018731891212,-48.714985856821,-48.6280953922917,-48.5412101838842,
-48.4543032923373,-48.3899129779471,-48.3030081068742,-48.216120774574,
-48.1292303100445,-48.0423451016371,-47.9554382100901,-47.8910478957002,
-47.8385267533552),.UNSPECIFIED.);
#209=B_SPLINE_CURVE_WITH_KNOTS('',3,(#10358,#10359,#10360,#10361,#10362,
#10363,#10364,#10365,#10366,#10367,#10368,#10369),.UNSPECIFIED.,.F.,.F.,
(4,2,2,2,2,4),(-6.46678606976702,-6.36974609711427,-6.35327484653255,-6.24967349408771,
-6.22280337759775,-6.16735576612806),.UNSPECIFIED.);
#210=B_SPLINE_CURVE_WITH_KNOTS('',3,(#10375,#10376,#10377,#10378,#10379),
 .UNSPECIFIED.,.F.,.F.,(4,1,4),(44.710117486282,44.897857402219,45.2918602818348),
 .UNSPECIFIED.);
#211=B_SPLINE_CURVE_WITH_KNOTS('',3,(#10380,#10381,#10382,#10383,#10384,
#10385,#10386,#10387,#10388,#10389,#10390,#10391,#10392,#10393,#10394,#10395,
#10396,#10397,#10398,#10399,#10400,#10401,#10402,#10403,#10404,#10405,#10406,
#10407,#10408,#10409,#10410,#10411,#10412,#10413,#10414,#10415,#10416,#10417,
#10418,#10419,#10420,#10421,#10422,#10423,#10424,#10425,#10426,#10427,#10428,
#10429,#10430,#10431,#10432,#10433,#10434,#10435,#10436,#10437,#10438,#10439,
#10440,#10441,#10442,#10443,#10444,#10445,#10446,#10447,#10448,#10449,#10450,
#10451,#10452,#10453,#10454,#10455,#10456,#10457,#10458,#10459,#10460,#10461,
#10462,#10463,#10464,#10465,#10466,#10467,#10468,#10469,#10470,#10471,#10472,
#10473,#10474,#10475,#10476,#10477,#10478,#10479,#10480,#10481,#10482,#10483,
#10484,#10485,#10486,#10487,#10488,#10489,#10490,#10491,#10492,#10493,#10494,
#10495,#10496,#10497,#10498,#10499,#10500,#10501,#10502,#10503,#10504,#10505,
#10506,#10507,#10508,#10509,#10510,#10511,#10512,#10513,#10514,#10515,#10516,
#10517,#10518,#10519,#10520,#10521,#10522,#10523,#10524,#10525,#10526,#10527,
#10528,#10529,#10530,#10531,#10532,#10533,#10534,#10535,#10536,#10537,#10538,
#10539,#10540,#10541,#10542,#10543,#10544,#10545,#10546,#10547,#10548,#10549,
#10550,#10551,#10552,#10553,#10554,#10555,#10556,#10557,#10558,#10559,#10560,
#10561,#10562,#10563,#10564,#10565,#10566,#10567,#10568,#10569,#10570,#10571,
#10572,#10573,#10574,#10575,#10576,#10577,#10578,#10579,#10580,#10581,#10582,
#10583,#10584,#10585,#10586,#10587,#10588,#10589,#10590),.UNSPECIFIED.,
 .F.,.F.,(4,3,3,3,3,3,3,3,3,3,3,3,3,3,3,3,3,3,3,3,3,3,3,3,3,3,3,3,3,3,3,
3,3,3,3,3,3,3,3,3,3,3,3,3,3,3,3,3,3,3,3,3,3,3,3,3,3,3,3,3,3,3,3,3,3,3,3,
3,3,3,4),(45.2918602912342,45.3839897102111,45.3967224844658,45.4836273555394,
45.5705146878403,45.6574051523704,45.7442903607789,45.8311972523266,45.8955875667127,
45.9824924377854,46.0693797700853,46.1562702346145,46.2431554430219,46.3300623345686,
46.3944526489596,46.4813575200326,46.5682448523329,46.6551353168625,46.7420205252702,
46.8289274168173,46.8933177312065,46.9802226022792,47.0671099345793,47.1540003991085,
47.240885607516,47.3277924990628,47.3921828134533,47.4790876845262,47.5659750168264,
47.6528654813558,47.7397506897635,47.8266575813105,47.8910478957002,47.9779527667731,
48.0648400990734,48.1517305636029,48.2386157720106,48.3255226635576,48.3899129779471,
48.47681784902,48.5637051813202,48.6505956458497,48.7374808542574,48.8243877458044,
48.888778060194,48.9756829312668,49.0625702635668,49.1494607280961,49.2363459365036,
49.3232528280504,49.3876431424408,49.4745480135137,49.5614353458139,49.6483258103434,
49.7352110187511,49.8221179102981,49.8865082246877,49.9734130957606,50.0603004280608,
50.1471908925903,50.234076100998,50.320982992545,50.3853733069346,50.4722781780076,
50.5591655103079,50.6460559748374,50.732941183245,50.8198480747921,50.8842383891815,
50.9711426268903,50.9933372706279),.UNSPECIFIED.);
#212=B_SPLINE_CURVE_WITH_KNOTS('',3,(#10591,#10592,#10593,#10594,#10595,
#10596,#10597,#10598,#10599,#10600,#10601,#10602,#10603,#10604,#10605,#10606,
#10607,#10608,#10609,#10610,#10611,#10612,#10613,#10614,#10615,#10616,#10617,
#10618,#10619,#10620,#10621,#10622,#10623,#10624,#10625,#10626,#10627,#10628,
#10629,#10630,#10631,#10632,#10633,#10634,#10635,#10636,#10637,#10638,#10639,
#10640,#10641,#10642,#10643,#10644,#10645,#10646,#10647,#10648,#10649,#10650,
#10651,#10652,#10653,#10654,#10655,#10656,#10657,#10658,#10659,#10660,#10661,
#10662,#10663,#10664,#10665,#10666,#10667,#10668,#10669,#10670,#10671,#10672,
#10673,#10674,#10675,#10676,#10677,#10678,#10679,#10680,#10681,#10682,#10683,
#10684,#10685,#10686,#10687,#10688,#10689,#10690,#10691,#10692,#10693,#10694,
#10695,#10696,#10697,#10698,#10699,#10700,#10701,#10702),.UNSPECIFIED.,
 .F.,.F.,(4,2,2,2,2,2,2,2,2,2,2,2,2,2,2,2,2,2,2,2,2,2,2,2,2,2,2,2,2,2,2,
2,2,2,2,2,2,2,2,2,2,2,2,2,2,2,2,2,2,2,2,2,2,2,2,4),(-6.16735576612806,-6.15921345146165,
-6.11345500378577,-6.01807848390996,-5.97776732229564,-5.92133925481309,
-5.85507237955178,-5.76574269662213,-5.72193933189343,-5.66052737580998,
-5.59325028222066,-5.51873451616644,-5.46743249191829,-5.41027892343107,
-5.34388007609257,-5.24667547941811,-5.20730073602016,-5.15235443733306,
-5.0866278090815,-4.99107975420786,-4.95085991288905,-4.89457189350567,
-4.82967302269615,-4.73488188081266,-4.69426163275514,-4.63736534206582,
-4.57134972752306,-4.48254497888756,-4.43840929496829,-4.37651978835189,
-4.30958035640124,-4.23801488265242,-4.18284695730065,-4.12965507624722,
-4.09471677844922,-4.07038370453636,-4.01862976067098,-3.92717495748881,
-3.86986731003032,-3.8033950930707,-3.70182512452207,-3.66560106131781,
-3.60357428245561,-3.53882169825608,-3.45805550073204,-3.41189659075085,
-3.36164150274549,-3.30921114318311,-3.28606788502557,-3.23338728280752,
-3.17281530728171,-3.1431045953554,-3.07197166944413,-3.01772333034713,
-2.99411202495098,-2.93408130173726),.UNSPECIFIED.);
#213=B_SPLINE_CURVE_WITH_KNOTS('',3,(#10708,#10709,#10710,#10711,#10712,
#10713,#10714,#10715,#10716,#10717,#10718,#10719),.UNSPECIFIED.,.F.,.F.,
(4,2,2,2,2,4),(-0.29941706624709,-0.272624008446249,-0.193071594358554,
-0.14393047447416,-0.0491105809088329,-4.41492292512854E-5),
 .UNSPECIFIED.);
#214=B_SPLINE_CURVE_WITH_KNOTS('',3,(#10720,#10721,#10722,#10723,#10724,
#10725,#10726,#10727,#10728,#10729,#10730,#10731,#10732,#10733,#10734),
 .UNSPECIFIED.,.F.,.F.,(4,1,1,1,1,1,1,1,1,1,1,1,4),(39.0086749840546,39.4103414975033,
39.9092065797502,40.4080716619971,40.9069367442439,41.4058018264908,41.9046669087377,
42.4035319909846,42.9023970732314,43.4012621554783,43.9001272377252,44.3989923199721,
44.710117486282),.UNSPECIFIED.);
#215=B_SPLINE_CURVE_WITH_KNOTS('',3,(#10736,#10737,#10738,#10739,#10740,
#10741,#10742,#10743,#10744,#10745,#10746,#10747,#10748,#10749,#10750,#10751,
#10752,#10753,#10754,#10755,#10756,#10757,#10758,#10759,#10760,#10761,#10762,
#10763,#10764,#10765,#10766,#10767,#10768,#10769,#10770,#10771,#10772,#10773,
#10774,#10775,#10776,#10777,#10778,#10779,#10780,#10781,#10782,#10783,#10784,
#10785,#10786,#10787,#10788,#10789,#10790,#10791,#10792,#10793,#10794,#10795,
#10796,#10797,#10798,#10799,#10800,#10801,#10802,#10803,#10804,#10805,#10806,
#10807,#10808,#10809,#10810,#10811,#10812,#10813,#10814,#10815,#10816,#10817,
#10818,#10819,#10820,#10821,#10822,#10823,#10824,#10825,#10826,#10827,#10828,
#10829,#10830,#10831,#10832,#10833,#10834,#10835,#10836,#10837),
 .UNSPECIFIED.,.F.,.F.,(4,2,2,2,2,2,2,2,2,2,2,2,2,2,2,2,2,2,2,2,2,2,2,2,
2,2,2,2,2,2,2,2,2,2,2,2,2,2,2,2,2,2,2,2,2,2,2,2,2,2,4),(-2.93408130173726,
-2.93304885547358,-2.91194674280188,-2.88204922197342,-2.84302030640522,
-2.77352700671621,-2.70675002102001,-2.64463095528211,-2.60033769366457,
-2.51176973473058,-2.44586660880208,-2.38876135407395,-2.34799899037949,
-2.25346425894163,-2.18361280540833,-2.12995714258924,-2.03336695858138,
-1.98251129590212,-1.88096958966132,-1.84930159101389,-1.80041718264956,
-1.74516693890976,-1.67541237326298,-1.6186224109205,-1.57807059358303,
-1.48313964198103,-1.4134917643136,-1.3597162357856,-1.30826755598738,-1.23305628927718,
-1.16582344893134,-1.10434789521201,-1.06049846430573,-0.971231602678871,
-0.904997802848148,-0.848507296731753,-0.808152960198933,-0.712848230441378,
-0.646904496746172,-0.592135568633003,-0.552865968410389,-0.45543675033151,
-0.388883997280267,-0.332023636198457,-0.308123738779688,-0.257508419796942,
-0.198789885410597,-0.152986897520325,-0.0793248458577054,-0.0663949178379873,
-4.4182641542272E-5),.UNSPECIFIED.);
#216=B_SPLINE_CURVE_WITH_KNOTS('',3,(#10838,#10839,#10840,#10841,#10842),
 .UNSPECIFIED.,.F.,.F.,(4,1,4),(-35.272156138996,-34.9205557572814,-34.690424885304),
 .UNSPECIFIED.);
#217=B_SPLINE_CURVE_WITH_KNOTS('',3,(#10847,#10848,#10849,#10850,#10851,
#10852,#10853,#10854,#10855,#10856,#10857,#10858,#10859,#10860,#10861,#10862,
#10863,#10864,#10865,#10866,#10867,#10868,#10869,#10870,#10871,#10872,#10873,
#10874,#10875,#10876,#10877,#10878,#10879,#10880,#10881,#10882,#10883,#10884,
#10885,#10886,#10887,#10888,#10889,#10890,#10891,#10892,#10893,#10894,#10895,
#10896,#10897,#10898,#10899,#10900,#10901,#10902,#10903,#10904,#10905,#10906,
#10907,#10908,#10909,#10910,#10911,#10912,#10913,#10914,#10915,#10916,#10917,
#10918,#10919,#10920,#10921,#10922,#10923,#10924,#10925,#10926,#10927,#10928,
#10929,#10930,#10931,#10932,#10933,#10934,#10935,#10936,#10937,#10938,#10939,
#10940,#10941,#10942,#10943,#10944,#10945,#10946,#10947,#10948,#10949,#10950,
#10951,#10952,#10953,#10954,#10955,#10956,#10957,#10958,#10959,#10960,#10961,
#10962,#10963,#10964),.UNSPECIFIED.,.F.,.F.,(4,2,2,2,2,2,2,2,2,2,2,2,2,
2,2,2,2,2,2,2,2,2,2,2,2,2,2,2,2,2,2,2,2,2,2,2,2,2,2,2,2,2,2,2,2,2,2,2,2,
2,2,2,2,2,2,2,2,2,4),(-3.53273226990805,-3.51217029370589,-3.43143246081615,
-3.38602691469201,-3.33619900388063,-3.2836417674659,-3.2333912848074,-3.18011428936759,
-3.13269368376827,-3.09047605886201,-2.99852804850881,-2.93085259017726,
-2.8733208960313,-2.86123265038794,-2.79119116778289,-2.7362228838575,-2.71271252262557,
-2.65289371301879,-2.6270334813131,-2.59632911246521,-2.55229814685202,
-2.49081566908837,-2.42306295857898,-2.36232675411795,-2.31900273175731,
-2.22889487345454,-2.16223976266328,-2.10653972026565,-2.06669457195355,
-1.97040951439539,-1.90341780941698,-1.84665279589094,-1.79446397924416,
-1.72073312461513,-1.65346107052155,-1.59203976036453,-1.54822866909107,
-1.4588996007104,-1.39263551281092,-1.33620007127111,-1.2958819143125,-1.20050681071984,
-1.17730395962771,-1.12221644598454,-1.07691779399216,-0.985679253607082,
-0.933714695344074,-0.909482207307218,-0.875100002972594,-0.820236697278058,
-0.768907984868682,-0.693855037781347,-0.62660630905221,-0.565153519541634,
-0.521320313654361,-0.432027958888678,-0.365781987637995,-0.309414102241624,
-0.29941706624709),.UNSPECIFIED.);
#218=B_SPLINE_CURVE_WITH_KNOTS('',3,(#10966,#10967,#10968,#10969,#10970,
#10971,#10972,#10973,#10974,#10975,#10976,#10977,#10978,#10979,#10980),
 .UNSPECIFIED.,.F.,.F.,(4,1,1,1,1,1,1,1,1,1,1,1,4),(-34.690424885304,-34.4216906750345,
-33.9228255927876,-33.4239605105408,-32.9250954282939,-32.426230346047,
-31.9273652638001,-31.4285001815533,-30.9296350993064,-30.4307700170595,
-29.9319049348126,-29.4330398525657,-28.9889708747585),.UNSPECIFIED.);
#219=B_SPLINE_CURVE_WITH_KNOTS('',3,(#10981,#10982,#10983,#10984,#10985,
#10986,#10987,#10988,#10989,#10990,#10991,#10992,#10993,#10994,#10995,#10996,
#10997,#10998,#10999,#11000,#11001,#11002,#11003,#11004,#11005),
 .UNSPECIFIED.,.F.,.F.,(4,3,3,3,3,3,3,3,4),(-28.9889708318164,-28.9341747703189,
-28.8472698992443,-28.7603825669425,-28.6734921024112,-28.5866068940016,
-28.4997000024527,-28.435309688072,-28.4072371742117),.UNSPECIFIED.);
#220=B_SPLINE_CURVE_WITH_KNOTS('',3,(#11011,#11012,#11013,#11014,#11015,
#11016,#11017,#11018,#11019,#11020,#11021,#11022,#11023,#11024),
 .UNSPECIFIED.,.F.,.F.,(4,2,2,2,2,2,4),(-0.299389883818606,-0.261813445457985,
-0.235776114650808,-0.189442449010928,-0.130882530543728,-0.0850842402352701,
-4.4159677240208E-5),.UNSPECIFIED.);
#221=B_SPLINE_CURVE_WITH_KNOTS('',3,(#11025,#11026,#11027,#11028,#11029,
#11030,#11031,#11032,#11033,#11034,#11035,#11036,#11037,#11038,#11039,#11040,
#11041,#11042,#11043,#11044,#11045,#11046,#11047,#11048,#11049,#11050,#11051,
#11052,#11053,#11054,#11055,#11056,#11057,#11058,#11059,#11060,#11061,#11062,
#11063,#11064,#11065,#11066,#11067,#11068,#11069,#11070,#11071,#11072,#11073,
#11074,#11075,#11076,#11077,#11078,#11079,#11080,#11081,#11082,#11083,#11084,
#11085,#11086,#11087,#11088,#11089,#11090,#11091,#11092,#11093,#11094,#11095,
#11096,#11097,#11098,#11099,#11100,#11101,#11102,#11103,#11104,#11105,#11106,
#11107,#11108,#11109,#11110,#11111,#11112,#11113,#11114,#11115,#11116,#11117,
#11118,#11119,#11120,#11121,#11122,#11123,#11124),.UNSPECIFIED.,.F.,.F.,
(4,2,2,2,2,2,2,2,2,2,2,2,2,2,2,2,2,2,2,2,2,2,2,2,2,2,2,2,2,2,2,2,2,2,2,
2,2,2,2,2,2,2,2,2,2,2,2,2,2,4),(-6.46680925296249,-6.38442007318614,-6.33863123016491,
-6.28248089476868,-6.23448359497408,-6.21006599349175,-6.14608635288184,
-6.09823123559437,-6.04639873864054,-5.95477998639039,-5.90909496631497,
-5.85413175757243,-5.83093420372116,-5.73604918032842,-5.69547435977023,
-5.63864626091275,-5.57258925836412,-5.48369869485737,-5.43961270500058,
-5.37779513039796,-5.31079934616192,-5.23445340596768,-5.18506973985015,
-5.12779019417545,-5.0612833673779,-4.96469937036644,-4.9250099182995,-4.86955389952252,
-4.80413015425949,-4.70888429015701,-4.67968108286381,-4.64838581031007,
-4.55174482168042,-4.49656510528779,-4.42664142849673,-4.41462808513177,
-4.3583027779773,-4.29069171816555,-4.19532338116545,-4.15500509298302,
-4.09856603006887,-4.03230201601623,-3.94297927638577,-3.89916840051344,
-3.83774544887639,-3.77047264300654,-3.6957926407437,-3.64557402910458,
-3.57459764904799,-3.53273226990805),.UNSPECIFIED.);
#222=B_SPLINE_CURVE_WITH_KNOTS('',3,(#11126,#11127,#11128,#11129,#11130,
#11131,#11132,#11133,#11134,#11135,#11136,#11137,#11138,#11139,#11140,#11141,
#11142,#11143,#11144,#11145,#11146,#11147,#11148,#11149,#11150,#11151,#11152,
#11153,#11154,#11155,#11156,#11157,#11158,#11159,#11160,#11161,#11162,#11163,
#11164,#11165,#11166,#11167,#11168,#11169,#11170,#11171,#11172,#11173,#11174,
#11175,#11176,#11177,#11178,#11179,#11180,#11181,#11182,#11183,#11184,#11185,
#11186,#11187,#11188,#11189,#11190,#11191,#11192,#11193,#11194,#11195,#11196,
#11197,#11198,#11199,#11200,#11201,#11202,#11203,#11204,#11205,#11206,#11207,
#11208,#11209,#11210,#11211,#11212,#11213,#11214,#11215,#11216,#11217,#11218,
#11219,#11220,#11221,#11222,#11223,#11224,#11225,#11226,#11227,#11228,#11229,
#11230,#11231,#11232,#11233,#11234,#11235,#11236,#11237,#11238,#11239,#11240,
#11241,#11242,#11243,#11244,#11245,#11246,#11247,#11248,#11249,#11250,#11251,
#11252,#11253,#11254,#11255,#11256,#11257,#11258,#11259,#11260,#11261,#11262,
#11263,#11264,#11265,#11266,#11267,#11268,#11269,#11270,#11271,#11272,#11273,
#11274,#11275,#11276,#11277,#11278,#11279,#11280,#11281,#11282,#11283,#11284,
#11285,#11286,#11287,#11288,#11289,#11290,#11291,#11292,#11293,#11294,#11295,
#11296,#11297,#11298,#11299,#11300,#11301,#11302,#11303,#11304,#11305,#11306,
#11307,#11308,#11309,#11310,#11311,#11312,#11313,#11314,#11315,#11316,#11317,
#11318,#11319,#11320,#11321,#11322,#11323,#11324,#11325,#11326,#11327,#11328,
#11329,#11330,#11331,#11332,#11333),.UNSPECIFIED.,.F.,.F.,(4,3,3,3,3,3,
3,3,3,3,3,3,3,3,3,3,3,3,3,3,3,3,3,3,3,3,3,3,3,3,3,3,3,3,3,3,3,3,3,3,3,3,
3,3,3,3,3,3,3,3,3,3,3,3,3,3,3,3,3,3,3,3,3,3,3,3,3,3,3,4),(-28.4072371742117,
-28.3203388291425,-28.23345547998,-28.1465675751263,-28.0596823795464,-27.9727775859982,
-27.9364446058251,-27.849539734752,-27.7626524024515,-27.6757619379218,
-27.5888767295139,-27.5019698379666,-27.4375795235782,-27.3506746525055,
-27.2637873202054,-27.1768968556761,-27.0900116472686,-27.0031047557218,
-26.9387144413314,-26.8518095702586,-26.7649222379583,-26.6780317734289,
-26.5911465650213,-26.5042396734743,-26.4398493590845,-26.3529444880116,
-26.2660571557112,-26.1791666911817,-26.0922814827741,-26.005374591227,
-25.9409842768376,-25.8540794057648,-25.7671920734646,-25.6803016089352,
-25.5934164005277,-25.5065095089807,-25.4421191945907,-25.3552143235177,
-25.2683269912175,-25.181436526688,-25.0945513182803,-25.0076444267333,
-24.9432541123438,-24.8563492412711,-24.7694619089709,-24.6825714444416,
-24.5956862360341,-24.5087793444873,-24.444389030097,-24.3574841590241,
-24.2705968267238,-24.1837063621944,-24.0968211537868,-24.0099142622398,
-23.9455239478501,-23.8586190767772,-23.771731744477,-23.6848412799475,
-23.5979560715399,-23.5110491799929,-23.4466588656032,-23.3597539945303,
-23.2728666622302,-23.1859761977007,-23.0990909892933,-23.0121840977463,
-22.9477937833563,-22.8596658861628,-22.7715576075161,-22.7057855246368),
 .UNSPECIFIED.);
#223=B_SPLINE_CURVE_WITH_KNOTS('',3,(#11334,#11335,#11336,#11337,#11338,
#11339,#11340,#11341,#11342,#11343,#11344,#11345),.UNSPECIFIED.,.F.,.F.,
(4,2,2,2,2,4),(-6.46682447949202,-6.36050996356338,-6.3360943075336,-6.25630149105725,
-6.21056945448505,-6.16740264682167),.UNSPECIFIED.);
#224=B_SPLINE_CURVE_WITH_KNOTS('',3,(#11350,#11351,#11352,#11353,#11354,
#11355,#11356,#11357,#11358,#11359,#11360,#11361,#11362,#11363,#11364,#11365,
#11366,#11367,#11368,#11369,#11370,#11371,#11372,#11373,#11374,#11375,#11376,
#11377,#11378,#11379,#11380,#11381,#11382,#11383,#11384,#11385,#11386,#11387,
#11388,#11389,#11390,#11391,#11392,#11393,#11394,#11395,#11396,#11397,#11398,
#11399,#11400,#11401,#11402,#11403,#11404,#11405,#11406,#11407,#11408,#11409,
#11410,#11411,#11412,#11413,#11414,#11415,#11416,#11417,#11418,#11419,#11420,
#11421,#11422,#11423,#11424,#11425,#11426,#11427,#11428,#11429,#11430,#11431,
#11432,#11433,#11434,#11435,#11436,#11437,#11438,#11439,#11440,#11441,#11442,
#11443,#11444,#11445,#11446,#11447,#11448,#11449,#11450,#11451,#11452,#11453,
#11454,#11455,#11456,#11457,#11458,#11459,#11460,#11461,#11462,#11463),
 .UNSPECIFIED.,.F.,.F.,(4,2,2,2,2,2,2,2,2,2,2,2,2,2,2,2,2,2,2,2,2,2,2,2,
2,2,2,2,2,2,2,2,2,2,2,2,2,2,2,2,2,2,2,2,2,2,2,2,2,2,2,2,2,2,2,2,4),(-3.53204766679888,
-3.49982421516289,-3.47626775403068,-3.42173140785212,-3.36502956813804,
-3.34916018500265,-3.31900175765622,-3.25903249160735,-3.23286461982597,
-3.18258127700049,-3.12816194346365,-3.0808734759152,-2.9894913208945,-2.93774632455422,
-2.9134283703324,-2.8785335070882,-2.82527828015015,-2.77339179940797,-2.6985322974546,
-2.63129804283183,-2.56988945816759,-2.5260875802445,-2.43681108506132,
-2.37058223526934,-2.31415718165661,-2.27384726176553,-2.17852929410056,
-2.11277006943221,-2.05784330744651,-2.01848056986588,-1.92131214425873,
-1.85494144458653,-1.79780691309944,-1.7437811615371,-1.67161461307685,
-1.60238749597071,-1.54374644484518,-1.5019238525573,-1.40929374630339,
-1.34120370799465,-1.28446321322327,-1.23364780099984,-1.15854616594712,
-1.09130309820798,-1.02984437445668,-0.986007010959373,-0.896723369940915,
-0.830481941090336,-0.774008379874504,-0.733665362334244,-0.638341651544923,
-0.572859401100843,-0.517511704800658,-0.477887577999317,-0.382128516453115,
-0.313437902341981,-0.299389883818606),.UNSPECIFIED.);
#225=B_SPLINE_CURVE_WITH_KNOTS('',3,(#11464,#11465,#11466,#11467,#11468,
#11469,#11470,#11471,#11472,#11473,#11474,#11475,#11476,#11477,#11478,#11479,
#11480,#11481,#11482,#11483,#11484,#11485,#11486,#11487,#11488,#11489,#11490,
#11491,#11492,#11493,#11494,#11495,#11496,#11497,#11498,#11499,#11500,#11501,
#11502,#11503,#11504,#11505,#11506,#11507,#11508,#11509,#11510,#11511,#11512,
#11513,#11514,#11515,#11516,#11517,#11518,#11519,#11520,#11521,#11522,#11523,
#11524,#11525,#11526,#11527,#11528,#11529,#11530,#11531,#11532,#11533,#11534,
#11535,#11536,#11537,#11538,#11539,#11540,#11541,#11542,#11543,#11544,#11545,
#11546,#11547,#11548,#11549,#11550,#11551,#11552,#11553,#11554,#11555,#11556,
#11557,#11558,#11559,#11560,#11561,#11562,#11563,#11564,#11565,#11566,#11567,
#11568,#11569,#11570,#11571,#11572,#11573,#11574,#11575,#11576,#11577,#11578,
#11579),.UNSPECIFIED.,.F.,.F.,(4,2,2,2,2,2,2,2,2,2,2,2,2,2,2,2,2,2,2,2,
2,2,2,2,2,2,2,2,2,2,2,2,2,2,2,2,2,2,2,2,2,2,2,2,2,2,2,2,2,2,2,2,2,2,2,2,
2,4),(-6.16740264682167,-6.11563365794476,-6.07532444593123,-6.0188994362692,
-5.9526295528832,-5.86329436872957,-5.81949304354482,-5.75808399690235,
-5.69080327778159,-5.61641055390375,-5.56442438541974,-5.50967749272918,
-5.43531913424907,-5.37797403236362,-5.31542697489267,-5.28344297801199,
-5.187491173287,-5.13146699607826,-5.05785111294859,-5.02512521307028,-4.96672822773466,
-4.94166264026503,-4.89085619430738,-4.79412421453088,-4.73988129353064,
-4.67071491794505,-4.57533420650859,-4.53502488775429,-4.47859966065171,
-4.41233088639287,-4.32299749628851,-4.27919607150013,-4.21778687492078,
-4.15050739988328,-4.07645024969687,-4.02442447301068,-3.95504297002624,
-3.90807117489429,-3.85496196358606,-3.78258372534596,-3.76997422021965,
-3.73282142537731,-3.67247481912233,-3.6489218695235,-3.59427629725168,
-3.524052896448,-3.51184750374542,-3.44139495257376,-3.3944774964091,-3.34125289840925,
-3.26408027613105,-3.2335036593988,-3.19016415151798,-3.12768137039442,
-3.06040030541999,-2.99899320386999,-2.95519186805188,-2.93416253856114),
 .UNSPECIFIED.);
#226=B_SPLINE_CURVE_WITH_KNOTS('',3,(#11585,#11586,#11587,#11588,#11589,
#11590,#11591,#11592,#11593,#11594,#11595,#11596,#11597,#11598),
 .UNSPECIFIED.,.F.,.F.,(4,2,2,2,2,2,4),(-0.299449727543266,-0.287141748908116,
-0.223493924177034,-0.196628569872181,-0.0910589500302473,-0.0595876231948999,
-4.44166853382205E-5),.UNSPECIFIED.);
#227=B_SPLINE_CURVE_WITH_KNOTS('',3,(#11599,#11600,#11601,#11602,#11603,
#11604,#11605,#11606,#11607,#11608,#11609,#11610,#11611,#11612,#11613,#11614,
#11615,#11616,#11617,#11618,#11619,#11620,#11621,#11622,#11623,#11624,#11625,
#11626,#11627,#11628,#11629,#11630,#11631,#11632,#11633,#11634,#11635,#11636,
#11637,#11638,#11639,#11640,#11641,#11642,#11643,#11644,#11645,#11646,#11647,
#11648,#11649,#11650,#11651,#11652,#11653,#11654,#11655,#11656,#11657,#11658,
#11659,#11660,#11661,#11662,#11663,#11664,#11665,#11666,#11667,#11668,#11669,
#11670,#11671,#11672,#11673,#11674,#11675,#11676,#11677,#11678,#11679,#11680,
#11681,#11682,#11683,#11684,#11685,#11686,#11687,#11688,#11689,#11690,#11691,
#11692,#11693,#11694,#11695,#11696,#11697,#11698,#11699,#11700),
 .UNSPECIFIED.,.F.,.F.,(4,2,2,2,2,2,2,2,2,2,2,2,2,2,2,2,2,2,2,2,2,2,2,2,
2,2,2,2,2,2,2,2,2,2,2,2,2,2,2,2,2,2,2,2,2,2,2,2,2,2,4),(-6.46489889827727,
-6.41872330513384,-6.37412377088042,-6.29277358877099,-6.23367193274467,
-6.18453002104199,-6.16086699093738,-6.1070859069055,-6.07222718892308,
-6.04791497663975,-5.99615591714179,-5.90471723431846,-5.84788220120214,
-5.78135088156293,-5.68395911282417,-5.64470746758329,-5.5899603318361,
-5.52401238712714,-5.42883390716834,-5.38845088473501,-5.33191111691408,
-5.26573841136418,-5.17658551816971,-5.132706347603,-5.07118567603099,-5.00402471070972,
-4.92852970160446,-4.87769643036357,-4.82291086896213,-4.7551299024827,
-4.65684710934992,-4.6180311171497,-4.56401881018412,-4.4975433648843,-4.40222212718805,
-4.3619159629023,-4.30549331372222,-4.23925984243533,-4.14998075341933,
-4.10618318176873,-4.04477879324171,-3.97753798197369,-3.9028000877843,
-3.85143748823915,-3.78217319085083,-3.73521456109145,-3.68213522868841,
-3.6097860585557,-3.59717469579274,-3.5603009501235,-3.53204766679888),
 .UNSPECIFIED.);
#228=B_SPLINE_CURVE_WITH_KNOTS('',3,(#11702,#11703,#11704,#11705,#11706,
#11707,#11708,#11709,#11710,#11711,#11712,#11713,#11714,#11715,#11716,#11717,
#11718,#11719,#11720,#11721,#11722,#11723,#11724,#11725,#11726,#11727,#11728,
#11729,#11730,#11731,#11732,#11733,#11734,#11735,#11736,#11737,#11738,#11739,
#11740,#11741,#11742,#11743,#11744,#11745,#11746,#11747,#11748,#11749,#11750,
#11751,#11752,#11753,#11754,#11755,#11756,#11757,#11758,#11759,#11760,#11761,
#11762,#11763,#11764,#11765,#11766,#11767,#11768,#11769,#11770,#11771,#11772,
#11773,#11774,#11775,#11776,#11777,#11778,#11779,#11780,#11781,#11782,#11783,
#11784,#11785,#11786,#11787,#11788,#11789,#11790,#11791,#11792,#11793,#11794,
#11795,#11796,#11797,#11798,#11799),.UNSPECIFIED.,.F.,.F.,(4,2,2,2,2,2,
2,2,2,2,2,2,2,2,2,2,2,2,2,2,2,2,2,2,2,2,2,2,2,2,2,2,2,2,2,2,2,2,2,2,2,2,
2,2,2,2,2,2,4),(-2.93416253856114,-2.8658487605409,-2.7995778425485,-2.74315680984522,
-2.70284793186746,-2.60745671480959,-2.58425385749397,-2.52916228410746,
-2.48271237418502,-2.43431203632113,-2.35897151295802,-2.29623441308256,
-2.22702425643058,-2.2150594067632,-2.14520695210958,-2.08988541840876,
-2.03740229931192,-1.97158151274785,-1.9243935139356,-1.84252085959546,
-1.77221502501627,-1.71643224860532,-1.67653453813169,-1.58035272865833,
-1.51310228342344,-1.45663670399648,-1.40556004367395,-1.33064675499336,
-1.26338555679267,-1.20194942495713,-1.15812767395307,-1.0688161119025,
-1.00256045821056,-0.946109900161033,-0.905781699015191,-0.810426361879754,
-0.744510427396677,-0.689724658717433,-0.650444847521016,-0.553035219322984,
-0.486499385581561,-0.429607216311699,-0.37861337124737,-0.301545345367292,
-0.255833865889075,-0.176908182396489,-0.151053254639042,-0.0538737242154548,
-4.41474414227578E-5),.UNSPECIFIED.);
#229=B_SPLINE_CURVE_WITH_KNOTS('',3,(#11800,#11801,#11802,#11803,#11804),
 .UNSPECIFIED.,.F.,.F.,(4,1,4),(-10.1394149102777,-9.97730164493754,-9.55771221567013),
 .UNSPECIFIED.);
#230=B_SPLINE_CURVE_WITH_KNOTS('',3,(#11810,#11811,#11812,#11813,#11814,
#11815,#11816,#11817,#11818,#11819,#11820,#11821,#11822,#11823,#11824,#11825,
#11826,#11827,#11828,#11829,#11830,#11831,#11832,#11833,#11834,#11835,#11836,
#11837,#11838,#11839,#11840,#11841,#11842,#11843,#11844,#11845,#11846,#11847,
#11848,#11849,#11850,#11851,#11852,#11853,#11854,#11855,#11856,#11857,#11858,
#11859,#11860,#11861,#11862,#11863,#11864,#11865,#11866,#11867,#11868,#11869,
#11870,#11871,#11872,#11873,#11874,#11875,#11876,#11877,#11878,#11879,#11880,
#11881,#11882,#11883,#11884,#11885,#11886,#11887,#11888,#11889,#11890,#11891,
#11892,#11893,#11894,#11895,#11896,#11897,#11898,#11899,#11900,#11901,#11902,
#11903,#11904,#11905,#11906,#11907,#11908,#11909,#11910,#11911,#11912,#11913,
#11914,#11915,#11916,#11917,#11918,#11919,#11920,#11921,#11922,#11923,#11924,
#11925,#11926,#11927,#11928,#11929,#11930),.UNSPECIFIED.,.F.,.F.,(4,3,3,
3,3,3,3,3,3,3,3,3,3,3,3,3,3,3,3,3,3,3,3,3,3,3,3,3,3,3,3,3,3,3,3,3,3,3,3,
3,4),(-3.27449886892727,-3.18761614376122,-3.10073466380896,-3.01383445139677,
-2.99319049348126,-2.90628637831284,-2.81939983534294,-2.73251020278055,
-2.64562584817912,-2.55871983698197,-2.49432541123439,-2.40740187823325,
-2.32049576623348,-2.23358652858203,-2.14668259333812,-2.05975722263729,
-1.99546032898751,-1.90861705921206,-1.82179160018738,-1.73496281748211,
-1.64813904686475,-1.56129263759828,-1.49659524674063,-1.409546118953,-1.32251404603999,
-1.23547955077808,-1.14845104380955,-1.06140335733105,-0.997730164493756,
-0.911094995373688,-0.824477714185506,-0.737855241080792,-0.651236305870609,
-0.564590515016393,-0.498865082246876,-0.411426010329821,-0.324005451184797,
-0.23658882318787,-0.149182757533382,-0.0617684476840146,0.),
 .UNSPECIFIED.);
#231=B_SPLINE_CURVE_WITH_KNOTS('',3,(#11933,#11934,#11935,#11936,#11937,
#11938,#11939,#11940,#11941,#11942,#11943,#11944,#11945,#11946,#11947,#11948,
#11949,#11950,#11951,#11952,#11953,#11954,#11955,#11956,#11957,#11958,#11959,
#11960,#11961,#11962,#11963,#11964,#11965,#11966,#11967,#11968,#11969,#11970,
#11971,#11972,#11973,#11974,#11975,#11976,#11977,#11978,#11979,#11980,#11981,
#11982,#11983,#11984,#11985,#11986,#11987,#11988,#11989,#11990,#11991,#11992,
#11993,#11994,#11995,#11996,#11997,#11998,#11999,#12000,#12001,#12002,#12003,
#12004,#12005,#12006,#12007,#12008,#12009,#12010,#12011,#12012,#12013,#12014,
#12015,#12016,#12017,#12018),.UNSPECIFIED.,.F.,.F.,(4,2,2,2,2,2,2,2,2,2,
2,2,2,2,2,2,2,2,2,2,2,2,2,2,2,2,2,2,2,2,2,2,2,2,2,2,2,2,2,2,2,2,4),(-6.09872156040909,
-6.00749427805286,-5.95742926200475,-5.8822861453486,-5.85809857342036,
-5.78022624038386,-5.73447496159819,-5.63655125552659,-5.59754757665871,
-5.54254594849079,-5.47675567134605,-5.38173848350033,-5.34123963860053,
-5.2847878351896,-5.21852565229132,-5.12920756671915,-5.085388588857,-5.023881617872,
-4.95667908611682,-4.88197222379136,-4.82990297021068,-4.77657904741458,
-4.7416829481717,-4.7173559230713,-4.66557707226733,-4.57412938940594,-4.517139405479,
-4.45003936488945,-4.35464382778697,-4.31434369371454,-4.25790859518146,
-4.19164432464583,-4.10233620771383,-4.05851850179046,-3.99710349847546,
-3.92982829922061,-3.85557626231805,-3.80332580353464,-3.74888562478497,
-3.67415716796871,-3.61620401672537,-3.55429967198194,-3.53290494255096),
 .UNSPECIFIED.);
#232=B_SPLINE_CURVE_WITH_KNOTS('',3,(#12020,#12021,#12022,#12023,#12024,
#12025,#12026,#12027,#12028,#12029,#12030,#12031,#12032,#12033,#12034,#12035,
#12036,#12037,#12038,#12039,#12040,#12041,#12042,#12043,#12044,#12045,#12046,
#12047,#12048,#12049,#12050,#12051,#12052,#12053,#12054,#12055,#12056,#12057,
#12058,#12059,#12060,#12061,#12062,#12063,#12064,#12065,#12066,#12067,#12068,
#12069,#12070,#12071,#12072,#12073,#12074,#12075,#12076,#12077,#12078,#12079,
#12080,#12081,#12082,#12083,#12084,#12085,#12086,#12087,#12088,#12089,#12090,
#12091,#12092,#12093,#12094,#12095,#12096,#12097,#12098,#12099,#12100,#12101,
#12102,#12103,#12104,#12105,#12106,#12107,#12108,#12109,#12110,#12111,#12112,
#12113,#12114,#12115,#12116,#12117,#12118,#12119,#12120,#12121,#12122,#12123,
#12124,#12125,#12126,#12127,#12128,#12129,#12130,#12131),.UNSPECIFIED.,
 .F.,.F.,(4,2,2,2,2,2,2,2,2,2,2,2,2,2,2,2,2,2,2,2,2,2,2,2,2,2,2,2,2,2,2,
2,2,2,2,2,2,2,2,2,2,2,2,2,2,2,2,2,2,2,2,2,2,2,2,4),(-3.53290494255096,-3.52220028737842,
-3.42634731206105,-3.37017838496927,-3.29839478213502,-3.26691402455281,
-3.20007373282,-3.17593663231303,-3.12374653463165,-3.04965357055732,-3.01994343430044,
-2.94881420189061,-2.89456737670883,-2.87095448036624,-2.80988148046529,
-2.78713854085941,-2.75675827729302,-2.71452852641755,-2.65036372662648,
-2.58355717107225,-2.52147302895015,-2.47720377226936,-2.3885914938337,
-2.32266697315307,-2.26559363389747,-2.22485270583054,-2.13027050849742,
-2.06329937440856,-2.00582007712969,-1.95319927659059,-1.88007976087321,
-1.81284777182449,-1.75136827054773,-1.70751629794579,-1.61825068119185,
-1.55201726258365,-1.49552289407734,-1.45516613459724,-1.35986300161468,
-1.29371280701194,-1.23920424216273,-1.20009091465415,-1.10234083242336,
-1.03544008499539,-0.97917424594622,-0.926655501305632,-0.853133409595351,
-0.78587124449319,-0.72443292852784,-0.680609872629603,-0.591296775173454,
-0.525040040584877,-0.468587421209888,-0.428257965622739,-0.332901112037465,
-0.299449727543266),.UNSPECIFIED.);
#233=B_SPLINE_CURVE_WITH_KNOTS('',3,(#12133,#12134,#12135,#12136,#12137,
#12138,#12139,#12140,#12141,#12142,#12143,#12144,#12145,#12146,#12147,#12148),
 .UNSPECIFIED.,.F.,.F.,(4,1,1,1,1,1,1,1,1,1,1,1,1,4),(-9.55771221567013,
-9.47843656269067,-8.97957148044379,-8.48070639819691,-7.98184131595003,
-7.48297623370316,-6.98411115145628,-6.4852460692094,-5.98638098696252,
-5.48751590471565,-4.98865082246877,-4.48978574022189,-3.99092065797502,
-3.85622961843176),.UNSPECIFIED.);
#234=B_SPLINE_CURVE_WITH_KNOTS('',3,(#12149,#12150,#12151,#12152,#12153,
#12154,#12155,#12156,#12157,#12158,#12159,#12160,#12161,#12162,#12163,#12164,
#12165,#12166,#12167,#12168,#12169,#12170,#12171,#12172,#12173),
 .UNSPECIFIED.,.F.,.F.,(4,3,3,3,3,3,3,3,4),(-3.85622960309808,-3.76518609625559,
-3.67851407926643,-3.59184296748841,-3.50515277910997,-3.49205557572814,
-3.4051555060907,-3.31826970863097,-3.27449886892727),.UNSPECIFIED.);
#235=B_SPLINE_CURVE_WITH_KNOTS('',3,(#12176,#12177,#12178,#12179,#12180,
#12181,#12182,#12183,#12184,#12185,#12186,#12187,#12188,#12189,#12190,#12191,
#12192,#12193,#12194,#12195,#12196,#12197,#12198,#12199,#12200,#12201,#12202,
#12203,#12204,#12205,#12206,#12207,#12208,#12209,#12210,#12211,#12212,#12213,
#12214,#12215,#12216,#12217,#12218,#12219,#12220,#12221,#12222,#12223,#12224,
#12225,#12226,#12227,#12228,#12229,#12230,#12231,#12232,#12233,#12234,#12235,
#12236,#12237,#12238,#12239,#12240,#12241,#12242,#12243,#12244,#12245,#12246,
#12247,#12248,#12249,#12250,#12251,#12252,#12253,#12254,#12255,#12256,#12257,
#12258,#12259,#12260,#12261,#12262,#12263,#12264,#12265,#12266,#12267,#12268,
#12269,#12270,#12271,#12272,#12273,#12274,#12275,#12276,#12277,#12278,#12279,
#12280,#12281,#12282,#12283,#12284,#12285,#12286,#12287,#12288,#12289,#12290,
#12291,#12292,#12293,#12294,#12295,#12296,#12297,#12298,#12299,#12300,#12301,
#12302,#12303,#12304,#12305,#12306,#12307,#12308,#12309,#12310,#12311,#12312,
#12313,#12314,#12315,#12316,#12317,#12318,#12319,#12320,#12321,#12322,#12323),
 .UNSPECIFIED.,.F.,.F.,(4,3,3,3,3,3,3,3,3,3,3,3,3,3,3,3,3,3,3,3,3,3,3,3,
3,3,3,3,3,3,3,3,3,3,3,3,3,3,3,3,3,3,3,3,3,3,3,3,3,4),(17.9335664739021,
18.0167532469952,18.0999437848247,18.1831297542433,18.2663367453336,18.3369797340602,
18.4201844407613,18.5033729159824,18.5865646052947,18.6697507067779,18.7529589155841,
18.8358448163071,18.9190496178174,19.0022381892001,19.0854299758621,19.1686161751527,
19.2518244815942,19.334709898554,19.4179146417019,19.5011031539455,19.5842948808243,
19.6674810200974,19.7506892667057,19.8335749808009,19.9167797515611,19.9999682917609,
20.0831600468638,20.1663462144518,20.2495544892548,20.3324400630477,20.4156448242515,
20.4988333547888,20.5820251001567,20.6652112579893,20.7484195230966,20.8313051452946,
20.9145099078806,20.9976984398057,21.0808901865568,21.1640763457672,21.2472846122301,
21.3301702275415,21.4133749913722,21.4965635245643,21.5797552726057,21.6629414331165,
21.7461497008841,21.8290353097884,21.9152790381123,21.9911485749839),
 .UNSPECIFIED.);
#236=B_SPLINE_CURVE_WITH_KNOTS('',3,(#12324,#12325,#12326,#12327,#12328,
#12329,#12330,#12331,#12332,#12333,#12334,#12335,#12336,#12337,#12338,#12339,
#12340,#12341,#12342,#12343,#12344,#12345,#12346,#12347,#12348,#12349,#12350,
#12351,#12352,#12353,#12354,#12355,#12356,#12357,#12358,#12359,#12360,#12361,
#12362,#12363,#12364,#12365,#12366,#12367,#12368,#12369,#12370,#12371,#12372,
#12373,#12374,#12375,#12376,#12377,#12378,#12379,#12380,#12381,#12382,#12383,
#12384,#12385,#12386,#12387,#12388,#12389,#12390,#12391,#12392,#12393,#12394,
#12395,#12396,#12397,#12398,#12399,#12400,#12401,#12402,#12403,#12404,#12405),
 .UNSPECIFIED.,.F.,.F.,(4,3,3,3,3,3,3,3,3,3,3,3,3,3,3,3,3,3,3,3,3,3,3,3,
3,3,3,4),(21.9911485751285,22.0753365293552,22.1584867074775,22.2431935497563,
22.3279003920352,22.4111051553879,22.4942936880944,22.5774854356416,22.6606715956548,
22.743879862924,22.8267654742821,22.9099702371268,22.9931587693188,23.0763505163464,
23.1595366758383,23.242744942588,23.325630556529,23.4088353195699,23.4920238519602,
23.5752155991881,23.6584017588804,23.7416100258298,23.8244956387759,23.9076996034063,
23.9908936205378,24.0740760457086,24.157266075357,24.216717884951),
 .UNSPECIFIED.);
#237=B_SPLINE_CURVE_WITH_KNOTS('',3,(#12407,#12408,#12409,#12410,#12411,
#12412,#12413,#12414,#12415,#12416,#12417,#12418,#12419,#12420,#12421,#12422,
#12423,#12424,#12425,#12426,#12427,#12428,#12429,#12430,#12431,#12432,#12433,
#12434,#12435,#12436,#12437,#12438,#12439,#12440,#12441,#12442,#12443,#12444,
#12445,#12446,#12447,#12448,#12449,#12450,#12451,#12452,#12453,#12454,#12455,
#12456,#12457,#12458,#12459,#12460,#12461,#12462,#12463,#12464,#12465,#12466,
#12467,#12468,#12469,#12470,#12471,#12472,#12473,#12474,#12475,#12476,#12477,
#12478,#12479,#12480,#12481,#12482,#12483,#12484,#12485,#12486,#12487,#12488),
 .UNSPECIFIED.,.F.,.F.,(4,3,3,3,3,3,3,3,3,3,3,3,3,3,3,3,3,3,3,3,3,3,3,3,
3,3,3,4),(21.9911485751285,22.0740357535315,22.1569243101385,22.2398084002157,
22.3227130388891,22.3802414429218,22.4634462136298,22.5466347537768,22.6298265088266,
22.7130126763613,22.7962209511113,22.8791065251687,22.962311286388,23.0454998169407,
23.1286915623243,23.2118777201727,23.2950859852955,23.3779716074156,23.461176370002,
23.5443649019275,23.627556648679,23.7107428078902,23.7939510743537,23.8768366896625,
23.961807761079,24.0449981194178,24.1308595473731,24.2167209753283),
 .UNSPECIFIED.);
#238=B_SPLINE_CURVE_WITH_KNOTS('',3,(#12489,#12490,#12491,#12492,#12493,
#12494,#12495,#12496,#12497,#12498,#12499,#12500),.UNSPECIFIED.,.F.,.F.,
(4,1,1,1,1,1,1,1,1,4),(17.9335636647299,18.3893207849468,18.8881858671937,
19.3870509494406,19.8859160316874,20.3847811139343,20.8836461961812,21.3825112784281,
21.881376360675,21.9911485751285),.UNSPECIFIED.);
#239=B_SPLINE_CURVE_WITH_KNOTS('',3,(#13106,#13107,#13108,#13109,#13110,
#13111,#13112,#13113,#13114,#13115,#13116,#13117,#13118,#13119,#13120,#13121,
#13122,#13123,#13124,#13125,#13126,#13127,#13128,#13129,#13130,#13131,#13132,
#13133,#13134,#13135,#13136,#13137,#13138,#13139,#13140,#13141,#13142,#13143,
#13144,#13145,#13146,#13147,#13148,#13149,#13150,#13151,#13152,#13153,#13154,
#13155,#13156,#13157,#13158,#13159,#13160,#13161,#13162,#13163,#13164,#13165,
#13166,#13167,#13168,#13169,#13170,#13171,#13172,#13173,#13174,#13175,#13176,
#13177,#13178,#13179,#13180,#13181,#13182,#13183,#13184,#13185,#13186,#13187,
#13188,#13189,#13190,#13191,#13192,#13193,#13194,#13195,#13196,#13197,#13198,
#13199,#13200,#13201,#13202,#13203,#13204,#13205,#13206,#13207,#13208,#13209,
#13210,#13211,#13212,#13213,#13214),.UNSPECIFIED.,.F.,.F.,(4,3,3,3,3,3,
3,3,3,3,3,3,3,3,3,3,3,3,3,3,3,3,3,3,3,3,3,3,3,3,3,3,3,3,3,3,4),(0.,0.0504375942257773,
0.101438275560147,0.152274851141068,0.202297764828748,0.22690245747524,
0.234086631352025,0.240471303452472,0.290088861606672,0.300961710715322,
0.350777659556104,0.400503660438411,0.449535507751653,0.461532737431569,
0.467774024709387,0.516338001498774,0.564497803363664,0.590321666658535,
0.638741707992651,0.678586472467412,0.686372968117243,0.73377925644372,
0.781056303170048,0.827516437945467,0.867854641571887,0.88442683737737,
0.893641475723393,0.901004136370051,0.947492195713632,0.988132467775281,
1.00845260380611,1.02136292095409,1.02877273983693,1.07430587688627,1.11913723974879,
1.13300977445962,1.14791015664666),.UNSPECIFIED.);
#240=B_SPLINE_CURVE_WITH_KNOTS('',3,(#13215,#13216,#13217,#13218,#13219,
#13220,#13221,#13222,#13223,#13224,#13225,#13226,#13227,#13228,#13229,#13230,
#13231,#13232,#13233,#13234,#13235,#13236,#13237,#13238,#13239,#13240,#13241,
#13242,#13243,#13244,#13245,#13246,#13247,#13248,#13249,#13250,#13251,#13252,
#13253,#13254,#13255,#13256,#13257,#13258,#13259,#13260,#13261,#13262,#13263,
#13264,#13265,#13266,#13267,#13268,#13269,#13270,#13271,#13272,#13273,#13274,
#13275,#13276,#13277,#13278,#13279,#13280,#13281,#13282,#13283,#13284,#13285,
#13286,#13287,#13288,#13289,#13290,#13291,#13292,#13293,#13294,#13295,#13296,
#13297,#13298,#13299,#13300,#13301,#13302,#13303,#13304,#13305,#13306,#13307,
#13308,#13309,#13310,#13311,#13312,#13313,#13314,#13315,#13316,#13317),
 .UNSPECIFIED.,.F.,.F.,(4,3,3,3,3,3,3,3,3,3,3,3,3,3,3,3,3,3,3,3,3,3,3,3,
3,3,3,3,3,3,3,3,3,3,4),(0.,0.0441046329368436,0.0893560015723501,0.135009828313389,
0.180704033776388,0.193938392122172,0.203205013495769,0.210348094081718,
0.257081268324377,0.264009708387661,0.310275553315939,0.357011042681633,
0.403920433703055,0.412397541162293,0.418270821497181,0.465898848410438,
0.514060796055048,0.539889422154883,0.58787940607083,0.631052019999542,
0.637374575989874,0.686132719762263,0.735352712852578,0.78461919933138,
0.827437465561715,0.848796759809365,0.857479630116978,0.869246119150075,
0.918875449822967,0.969139233393724,0.998311819542916,1.02159545864218,
1.07387015547638,1.12614485231058,1.14369440702988),.UNSPECIFIED.);
#241=B_SPLINE_CURVE_WITH_KNOTS('',3,(#13318,#13319,#13320,#13321),
 .UNSPECIFIED.,.F.,.F.,(4,4),(-0.000845053830584482,0.),.UNSPECIFIED.);
#242=B_SPLINE_CURVE_WITH_KNOTS('',3,(#13926,#13927,#13928,#13929,#13930,
#13931,#13932,#13933,#13934,#13935,#13936,#13937,#13938,#13939,#13940,#13941,
#13942,#13943,#13944,#13945,#13946,#13947,#13948,#13949,#13950,#13951,#13952,
#13953,#13954,#13955,#13956,#13957,#13958,#13959,#13960,#13961,#13962,#13963,
#13964,#13965,#13966,#13967,#13968,#13969,#13970,#13971,#13972,#13973,#13974,
#13975,#13976,#13977,#13978,#13979,#13980,#13981,#13982,#13983,#13984,#13985,
#13986,#13987,#13988,#13989,#13990,#13991,#13992,#13993,#13994,#13995,#13996,
#13997,#13998,#13999,#14000,#14001,#14002,#14003,#14004,#14005,#14006,#14007,
#14008,#14009,#14010,#14011,#14012,#14013,#14014,#14015,#14016,#14017,#14018,
#14019,#14020,#14021,#14022,#14023,#14024,#14025,#14026,#14027,#14028,#14029,
#14030,#14031),.UNSPECIFIED.,.F.,.F.,(4,3,3,3,3,3,3,3,3,3,3,3,3,3,3,3,3,
3,3,3,3,3,3,3,3,3,3,3,3,3,3,3,3,3,3,4),(0.,0.0441046059006624,0.0893559560019204,
0.135009773091842,0.180703983785403,0.193938306952095,0.20186334331925,
0.20763014540964,0.254347571323218,0.264009708387664,0.310275573079556,
0.357011074596214,0.40392046597413,0.412397589145282,0.418270878708949,
0.465898922469038,0.514060873473489,0.539889422154889,0.587879400706368,
0.63105191632105,0.63737455243671,0.686132686358541,0.735352674476775,0.784619161308775,
0.827437465561743,0.846106677233546,0.854394315893421,0.861034178817951,
0.910558531735202,0.960799533634331,0.998311819663738,1.00642292873682,
1.05734275824645,1.10836149070654,1.12614485231059,1.14369440711896),
 .UNSPECIFIED.);
#243=B_SPLINE_CURVE_WITH_KNOTS('',3,(#14033,#14034,#14035,#14036),
 .UNSPECIFIED.,.F.,.F.,(4,4),(0.,0.000845029145043154),.UNSPECIFIED.);
#244=B_SPLINE_CURVE_WITH_KNOTS('',3,(#14037,#14038,#14039,#14040,#14041,
#14042,#14043,#14044,#14045,#14046,#14047,#14048,#14049,#14050,#14051,#14052,
#14053,#14054,#14055,#14056,#14057,#14058,#14059,#14060,#14061,#14062,#14063,
#14064,#14065,#14066,#14067,#14068,#14069,#14070,#14071,#14072,#14073,#14074,
#14075,#14076,#14077,#14078,#14079,#14080,#14081,#14082,#14083,#14084,#14085,
#14086,#14087,#14088,#14089,#14090,#14091,#14092,#14093,#14094,#14095,#14096,
#14097,#14098,#14099,#14100,#14101,#14102,#14103,#14104,#14105,#14106,#14107,
#14108,#14109,#14110,#14111,#14112,#14113,#14114,#14115,#14116,#14117,#14118,
#14119,#14120,#14121,#14122,#14123,#14124,#14125,#14126,#14127,#14128,#14129,
#14130,#14131,#14132,#14133,#14134,#14135,#14136,#14137,#14138,#14139,#14140,
#14141,#14142),.UNSPECIFIED.,.F.,.F.,(4,3,3,3,3,3,3,3,3,3,3,3,3,3,3,3,3,
3,3,3,3,3,3,3,3,3,3,3,3,3,3,3,3,3,3,4),(0.,0.0504375760143521,0.101438257257583,
0.152274841648771,0.202297771586617,0.226902464456934,0.234086657304898,
0.24047130670072,0.290088872824462,0.300961710715323,0.350765609901174,
0.400474445038685,0.447936250443642,0.461532739091791,0.473284706306216,
0.521843710447206,0.569966130302076,0.590321666658515,0.638741707119349,
0.678586470967118,0.686372967853733,0.733779255798812,0.781056301894992,
0.827516432241143,0.867854641571862,0.894324374113917,0.901004135934422,
0.947484960275739,0.993866163821704,1.01125911515144,1.02227210782131,1.03199949352102,
1.07751008814374,1.12231103370646,1.1330097744596,1.14791015664664),
 .UNSPECIFIED.);
#245=B_SPLINE_CURVE_WITH_KNOTS('',3,(#14172,#14173,#14174,#14175,#14176,
#14177,#14178,#14179,#14180,#14181,#14182,#14183,#14184,#14185,#14186,#14187,
#14188,#14189,#14190,#14191,#14192,#14193,#14194,#14195,#14196,#14197,#14198,
#14199,#14200,#14201,#14202,#14203,#14204,#14205,#14206,#14207,#14208,#14209,
#14210,#14211,#14212,#14213,#14214,#14215,#14216,#14217,#14218,#14219,#14220,
#14221,#14222,#14223,#14224,#14225,#14226,#14227,#14228,#14229,#14230,#14231,
#14232,#14233,#14234,#14235,#14236,#14237,#14238,#14239,#14240,#14241,#14242,
#14243,#14244,#14245,#14246,#14247),.UNSPECIFIED.,.F.,.F.,(4,3,3,3,3,3,
3,3,3,3,3,3,3,3,3,3,3,3,3,3,3,3,3,3,3,4),(-4.0925417488383,-4.00338655469883,
-3.99308979752421,-3.90920016748237,-3.82532702077677,-3.74145069821191,
-3.65757994399786,-3.57368718421055,-3.49395357283368,-3.4100720147821,
-3.32620694997733,-3.24233864749926,-3.15847586347122,-3.07459091498262,
-2.99481734814316,-2.91093267105568,-2.82706451995705,-2.74319321087022,
-2.65932746977074,-2.57543967428308,-2.49568112345263,-2.41211430491665,
-2.32654186004125,-2.24299415390576,-2.1564093396604,-2.06982452541504),
 .UNSPECIFIED.);
#246=B_SPLINE_CURVE_WITH_KNOTS('',3,(#14250,#14251,#14252,#14253,#14254,
#14255),.UNSPECIFIED.,.F.,.F.,(4,1,1,4),(0.,0.498871935148122,0.997743870296246,
1.11885509353771),.UNSPECIFIED.);
#247=B_SPLINE_CURVE_WITH_KNOTS('',3,(#14260,#14261,#14262,#14263,#14264,
#14265,#14266,#14267,#14268,#14269,#14270,#14271,#14272,#14273,#14274,#14275,
#14276,#14277,#14278,#14279,#14280,#14281,#14282,#14283,#14284,#14285,#14286,
#14287,#14288,#14289,#14290,#14291,#14292,#14293,#14294,#14295,#14296,#14297,
#14298,#14299,#14300,#14301,#14302,#14303,#14304,#14305,#14306,#14307,#14308,
#14309,#14310,#14311,#14312,#14313,#14314,#14315,#14316,#14317,#14318,#14319,
#14320,#14321,#14322,#14323,#14324,#14325,#14326,#14327,#14328,#14329,#14330,
#14331,#14332,#14333,#14334,#14335,#14336,#14337,#14338,#14339,#14340,#14341,
#14342,#14343,#14344,#14345,#14346,#14347,#14348,#14349,#14350,#14351,#14352,
#14353,#14354,#14355,#14356,#14357,#14358,#14359,#14360,#14361,#14362,#14363,
#14364,#14365,#14366,#14367,#14368,#14369,#14370,#14371,#14372,#14373,#14374,
#14375,#14376,#14377,#14378,#14379,#14380,#14381,#14382,#14383,#14384,#14385,
#14386,#14387,#14388,#14389,#14390,#14391,#14392,#14393,#14394,#14395,#14396,
#14397,#14398,#14399,#14400,#14401,#14402,#14403,#14404,#14405,#14406,#14407,
#14408,#14409,#14410,#14411,#14412,#14413,#14414,#14415,#14416,#14417,#14418,
#14419,#14420,#14421,#14422,#14423,#14424,#14425,#14426,#14427,#14428,#14429,
#14430,#14431,#14432,#14433,#14434,#14435,#14436,#14437,#14438,#14439,#14440,
#14441,#14442,#14443,#14444,#14445,#14446,#14447,#14448,#14449,#14450,#14451,
#14452,#14453,#14454,#14455,#14456,#14457,#14458,#14459,#14460,#14461,#14462,
#14463,#14464,#14465,#14466,#14467,#14468,#14469,#14470,#14471,#14472,#14473,
#14474,#14475,#14476,#14477,#14478,#14479,#14480,#14481,#14482,#14483,#14484,
#14485,#14486,#14487,#14488),.UNSPECIFIED.,.F.,.F.,(4,3,3,3,3,3,3,3,3,3,
3,3,3,3,3,3,3,3,3,3,3,3,3,3,3,3,3,3,3,3,3,3,3,3,3,3,3,3,3,3,3,3,3,3,3,3,
3,3,3,3,3,3,3,3,3,3,3,3,3,3,3,3,3,3,3,3,3,3,3,3,3,3,3,3,3,3,4),(-10.3757270560179,
-10.2921698941946,-10.2086117681573,-10.1250584922855,-10.0414843439998,
-9.98272449381053,-9.8988388229379,-9.81496964470574,-9.73109726706072,
-9.64723043695178,-9.56334152922015,-9.48358826912,-9.39970259968953,-9.31583342289778,
-9.23196104667645,-9.14809421797911,-9.06420531162583,-8.98445204442947,
-8.90056637659468,-8.81669720141806,-8.73282482682699,-8.64895799976509,
-8.56506909503931,-8.48531581973895,-8.40143014094074,-8.31756095474053,
-8.23368856913816,-8.14982173109376,-8.06593281553891,-7.98617959504842,
-7.90229394774752,-7.81842479317629,-7.73455243910345,-7.65068563247056,
-7.56679674783129,-7.4870433703579,-7.40315765686906,-7.31928843588881,
-7.23541601570045,-7.15154914324569,-7.06766019390088,-6.98790714566737,
-6.90402153903721,-6.82015242517192,-6.73628011147098,-6.6524133449469,
-6.56852449959617,-6.48877092097684,-6.40488520025293,-6.32101597225773,
-6.23714354545871,-6.1532766666274,-6.06938771135321,-5.98963469628632,
-5.9057489595102,-5.82187971461069,-5.73800726976125,-5.65414037229036,
-5.57025139758467,-5.49049847159579,-5.4066132244952,-5.32274447232866,
-5.23887252021098,-5.15500611447788,-5.07111762514282,-4.99136224690526,
-4.90747538257756,-4.82360500594776,-4.73973143373954,-4.65586341356851,
-4.57197333463933,-4.49222602221474,-4.40866870611299,-4.32512134153701,
-4.24158525877463,-4.15803693785589,-4.09254174894968),.UNSPECIFIED.);
#248=B_SPLINE_CURVE_WITH_KNOTS('',3,(#14489,#14490,#14491,#14492,#14493,
#14494,#14495,#14496,#14497,#14498,#14499,#14500,#14501,#14502,#14503,#14504),
 .UNSPECIFIED.,.F.,.F.,(4,1,1,1,1,1,1,1,1,1,1,1,1,4),(1.11885509353771,
1.49661580544437,1.9954877405925,2.49435967574062,2.99323161088875,3.49210354603688,
3.990975481185,4.48984741633313,4.98871935148126,5.48759128662938,5.98646322177751,
6.48533515692564,6.98420709207376,7.4020404007173),.UNSPECIFIED.);
#249=B_SPLINE_CURVE_WITH_KNOTS('',3,(#14509,#14510,#14511,#14512,#14513,
#14514,#14515,#14516,#14517,#14518,#14519,#14520,#14521,#14522,#14523,#14524,
#14525),.UNSPECIFIED.,.F.,.F.,(4,1,1,1,1,1,1,1,1,1,1,1,1,1,4),(-16.6589123270017,
-16.4714954147874,-15.9723591900968,-15.4732229654063,-14.9740867407158,
-14.4749505160253,-13.9758142913347,-13.4766780666442,-12.9775418419537,
-12.4784056172632,-11.9792693925726,-11.4801331678821,-10.9809969431916,
-10.4818607185011,-10.3757270560179),.UNSPECIFIED.);
#250=B_SPLINE_CURVE_WITH_KNOTS('',3,(#14526,#14527,#14528,#14529,#14530,
#14531,#14532,#14533,#14534,#14535,#14536,#14537,#14538,#14539,#14540,#14541,
#14542),.UNSPECIFIED.,.F.,.F.,(4,1,1,1,1,1,1,1,1,1,1,1,1,1,4),(7.4020404007173,
7.48307902722189,7.98195096237001,8.48082289751813,8.97969483266625,9.47856676781438,
9.9774387029625,10.4763106381106,10.9751825732587,11.4740545084069,11.972926443555,
12.4717983787031,12.9706703138512,13.4695422489993,13.6852256829822),
 .UNSPECIFIED.);
#251=B_SPLINE_CURVE_WITH_KNOTS('',3,(#14547,#14548,#14549,#14550,#14551,
#14552,#14553,#14554,#14555,#14556,#14557,#14558,#14559,#14560,#14561,#14562,
#14563,#14564,#14565,#14566,#14567,#14568,#14569,#14570,#14571,#14572,#14573,
#14574,#14575,#14576,#14577,#14578,#14579,#14580,#14581,#14582,#14583,#14584,
#14585,#14586,#14587,#14588,#14589,#14590,#14591,#14592,#14593,#14594,#14595,
#14596,#14597,#14598,#14599,#14600,#14601,#14602,#14603,#14604,#14605,#14606,
#14607,#14608,#14609,#14610,#14611,#14612,#14613,#14614,#14615,#14616,#14617,
#14618,#14619,#14620,#14621,#14622,#14623,#14624,#14625,#14626,#14627,#14628,
#14629,#14630,#14631,#14632,#14633,#14634,#14635,#14636,#14637,#14638,#14639,
#14640,#14641,#14642,#14643,#14644,#14645,#14646,#14647,#14648,#14649,#14650,
#14651,#14652,#14653,#14654,#14655,#14656,#14657,#14658,#14659,#14660,#14661,
#14662,#14663,#14664,#14665,#14666,#14667,#14668,#14669,#14670,#14671,#14672,
#14673,#14674,#14675,#14676,#14677,#14678,#14679,#14680,#14681,#14682,#14683,
#14684,#14685,#14686,#14687,#14688,#14689,#14690,#14691,#14692,#14693,#14694,
#14695,#14696,#14697,#14698,#14699,#14700,#14701,#14702,#14703,#14704,#14705,
#14706,#14707,#14708,#14709,#14710,#14711,#14712,#14713,#14714,#14715,#14716,
#14717,#14718,#14719,#14720,#14721,#14722,#14723,#14724,#14725,#14726,#14727,
#14728,#14729,#14730,#14731,#14732,#14733,#14734,#14735,#14736,#14737,#14738,
#14739,#14740,#14741,#14742,#14743,#14744,#14745,#14746,#14747,#14748,#14749,
#14750,#14751,#14752,#14753,#14754,#14755,#14756,#14757,#14758,#14759,#14760,
#14761,#14762,#14763,#14764,#14765,#14766,#14767,#14768,#14769,#14770,#14771,
#14772,#14773,#14774,#14775),.UNSPECIFIED.,.F.,.F.,(4,3,3,3,3,3,3,3,3,3,
3,3,3,3,3,3,3,3,3,3,3,3,3,3,3,3,3,3,3,3,3,3,3,3,3,3,3,3,3,3,3,3,3,3,3,3,
3,3,3,3,3,3,3,3,3,3,3,3,3,3,3,3,3,3,3,3,3,3,3,3,3,3,3,3,3,3,4),(-22.9420976702851,
-22.8583444588836,-22.7746078996228,-22.6908686933099,-22.6071340014371,
-22.5233784473718,-22.4611301110737,-22.37724444117,-22.2933752639082,-22.2095028872263,
-22.1256360580747,-22.0417471512818,-21.9619938863832,-21.8781082164793,
-21.7942390392172,-21.7103666625351,-21.6264998333833,-21.54261092659,-21.4628576616926,
-21.3789719917889,-21.2951028145268,-21.2112304378449,-21.1273636086934,
-21.0434747019003,-20.9637214370021,-20.8798357670984,-20.7959665898365,
-20.7120942131547,-20.6282273840031,-20.5443384772101,-20.4645852123116,
-20.3806995424079,-20.2968303651459,-20.2129579884638,-20.1290911593122,
-20.045202252519,-19.9654489876211,-19.8815633177171,-19.797694140455,-19.713821763773,
-19.6299549346209,-19.5460660278276,-19.4663127629305,-19.3824270930267,
-19.2985579157645,-19.2146855390827,-19.1308187099311,-19.0469298031378,
-18.96717653824,-18.8832908683363,-18.7994216910748,-18.7155493143931,-18.6316824852416,
-18.5477935784487,-18.4680403135495,-18.3841546436457,-18.300285466383,
-18.2164130897008,-18.1325462605488,-18.0486573537555,-17.9689040888589,
-17.8850184189553,-17.801149241693,-17.717276865011,-17.6334100358592,-17.5495211290661,
-17.4697678641684,-17.3858821942648,-17.3020130170031,-17.2181406403213,
-17.1342738111701,-17.0503849043771,-16.9706316394779,-16.8865508561898,
-16.8024890596186,-16.7184321798819,-16.6589123631975),.UNSPECIFIED.);
#252=B_SPLINE_CURVE_WITH_KNOTS('',3,(#14776,#14777,#14778,#14779,#14780,
#14781,#14782,#14783,#14784,#14785,#14786,#14787,#14788,#14789,#14790,#14791,
#14792,#14793,#14794,#14795,#14796,#14797,#14798,#14799,#14800,#14801,#14802,
#14803,#14804,#14805,#14806,#14807,#14808,#14809,#14810,#14811,#14812,#14813,
#14814,#14815,#14816,#14817,#14818,#14819,#14820,#14821,#14822,#14823,#14824,
#14825,#14826,#14827,#14828,#14829,#14830,#14831,#14832,#14833,#14834,#14835,
#14836,#14837,#14838,#14839,#14840,#14841,#14842,#14843,#14844,#14845,#14846,
#14847,#14848,#14849,#14850,#14851,#14852,#14853,#14854,#14855,#14856,#14857,
#14858,#14859,#14860,#14861,#14862,#14863,#14864,#14865,#14866,#14867,#14868,
#14869,#14870,#14871,#14872,#14873,#14874,#14875,#14876,#14877,#14878,#14879,
#14880,#14881,#14882,#14883,#14884,#14885,#14886,#14887,#14888,#14889,#14890,
#14891,#14892,#14893,#14894,#14895,#14896,#14897,#14898,#14899,#14900,#14901,
#14902,#14903,#14904,#14905,#14906,#14907,#14908,#14909,#14910,#14911,#14912,
#14913,#14914,#14915,#14916,#14917,#14918,#14919,#14920,#14921,#14922,#14923,
#14924,#14925,#14926,#14927,#14928,#14929,#14930,#14931,#14932,#14933,#14934,
#14935,#14936,#14937,#14938,#14939,#14940,#14941,#14942,#14943,#14944,#14945,
#14946,#14947,#14948,#14949,#14950,#14951,#14952,#14953,#14954,#14955,#14956,
#14957,#14958,#14959,#14960,#14961,#14962,#14963,#14964,#14965,#14966,#14967,
#14968,#14969,#14970,#14971,#14972,#14973,#14974,#14975,#14976,#14977,#14978,
#14979,#14980,#14981,#14982,#14983,#14984,#14985,#14986,#14987,#14988,#14989,
#14990,#14991,#14992,#14993,#14994,#14995,#14996,#14997,#14998,#14999,#15000,
#15001,#15002,#15003,#15004,#15005,#15006,#15007),.UNSPECIFIED.,.F.,.F.,
(4,3,3,3,3,3,3,3,3,3,3,3,3,3,3,3,3,3,3,3,3,3,3,3,3,3,3,3,3,3,3,3,3,3,3,
3,3,3,3,3,3,3,3,3,3,3,3,3,3,3,3,3,3,3,3,3,3,3,3,3,3,3,3,3,3,3,3,3,3,3,3,
3,3,3,3,3,3,4),(13.6852257078969,13.7696192421721,13.8540154419322,13.9384321835534,
13.9684141841475,14.0523012934223,14.1361719329257,14.2200457703978,14.3039140722452,
14.3878043962055,14.4672861192956,14.5511732285658,14.6350438680643,14.7189177055317,
14.8027860073745,14.8866763313302,14.9661580544437,15.0500451637151,15.1339158032148,
15.2177896406835,15.3016579425272,15.3855482664841,15.4650299895918,15.5489170988635,
15.632787738364,15.716661575833,15.8005298776769,15.8844202016341,15.96390192474,
16.0477890340111,16.1316596735105,16.2155335109788,16.2994018128224,16.3832921367788,
16.4627738598881,16.5466609691597,16.6305316086596,16.7144054461283,16.7982737479722,
16.8821640719291,16.9616457950362,17.0455329043074,17.1294035438071,17.2132773812757,
17.2971456831196,17.3810360070764,17.4605177301843,17.5444048394559,17.6282754789555,
17.7121493164243,17.7960176182683,17.8799079422252,17.9593896653325,18.0432767746037,
18.1271474141036,18.2110212515721,18.2948895534159,18.3787798773727,18.4582616004806,
18.5421487097518,18.6260193492519,18.7098931867206,18.793761488564,18.8776518125207,
18.9571335356287,19.0410206449002,19.1248912844002,19.2087651218687,19.2926334237124,
19.3765237476693,19.4560054707768,19.5398925800482,19.6237632195474,19.7076370570163,
19.7915053588603,19.8753956828172,19.954877405925,19.9684110150765),
 .UNSPECIFIED.);
#253=B_SPLINE_CURVE_WITH_KNOTS('',3,(#15012,#15013,#15014,#15015,#15016,
#15017,#15018,#15019,#15020,#15021,#15022,#15023,#15024,#15025,#15026,#15027,
#15028,#15029,#15030,#15031,#15032,#15033,#15034,#15035,#15036,#15037,#15038,
#15039,#15040,#15041,#15042,#15043,#15044,#15045,#15046,#15047,#15048,#15049,
#15050,#15051,#15052,#15053,#15054,#15055,#15056,#15057,#15058,#15059,#15060,
#15061,#15062,#15063,#15064,#15065,#15066,#15067,#15068,#15069,#15070,#15071,
#15072,#15073,#15074,#15075,#15076,#15077,#15078,#15079,#15080,#15081,#15082,
#15083,#15084,#15085,#15086,#15087,#15088,#15089,#15090,#15091,#15092,#15093,
#15094,#15095,#15096,#15097,#15098,#15099,#15100,#15101,#15102,#15103,#15104,
#15105,#15106,#15107,#15108,#15109,#15110,#15111,#15112,#15113,#15114,#15115,
#15116,#15117,#15118,#15119,#15120,#15121,#15122,#15123,#15124,#15125,#15126,
#15127,#15128,#15129,#15130,#15131,#15132,#15133,#15134,#15135,#15136,#15137,
#15138,#15139,#15140,#15141,#15142,#15143,#15144,#15145,#15146,#15147,#15148,
#15149,#15150,#15151,#15152,#15153,#15154,#15155,#15156,#15157,#15158,#15159,
#15160,#15161,#15162,#15163,#15164,#15165,#15166,#15167,#15168,#15169,#15170,
#15171,#15172,#15173,#15174,#15175,#15176,#15177,#15178,#15179,#15180,#15181,
#15182,#15183,#15184,#15185,#15186,#15187,#15188,#15189,#15190,#15191,#15192,
#15193,#15194,#15195,#15196,#15197,#15198,#15199,#15200,#15201,#15202,#15203,
#15204,#15205,#15206,#15207,#15208,#15209,#15210,#15211,#15212,#15213,#15214,
#15215,#15216,#15217,#15218,#15219,#15220,#15221,#15222,#15223,#15224,#15225,
#15226,#15227,#15228,#15229,#15230,#15231,#15232,#15233,#15234,#15235,#15236,
#15237,#15238,#15239,#15240,#15241,#15242,#15243),.UNSPECIFIED.,.F.,.F.,
(4,3,3,3,3,3,3,3,3,3,3,3,3,3,3,3,3,3,3,3,3,3,3,3,3,3,3,3,3,3,3,3,3,3,3,
3,3,3,3,3,3,3,3,3,3,3,3,3,3,3,3,3,3,3,3,3,3,3,3,3,3,3,3,3,3,3,3,3,3,3,3,
3,3,3,3,3,3,4),(-29.2252829775567,-29.1407809000066,-29.0562748594698,-28.9717485871814,
-28.9499010320505,-28.8660153621469,-28.7821461848854,-28.6982738082037,
-28.6144069790521,-28.5305180722592,-28.45076480736,-28.3668791374562,-28.2830099601946,
-28.1991375835126,-28.115270754361,-28.0313818475678,-27.9516285826695,
-27.8677429127658,-27.7838737355038,-27.7000013588219,-27.6161345296702,
-27.5322456228771,-27.452492357979,-27.3686066880751,-27.2847375108129,
-27.2008651341309,-27.1169983049791,-27.0331093981858,-26.9533561332884,
-26.8694704633847,-26.7856012861231,-26.7017289094412,-26.6178620802896,
-26.5339731734966,-26.4542199085979,-26.3703342386943,-26.2864650614322,
-26.2025926847503,-26.1187258555989,-26.0348369488059,-25.9550836839074,
-25.8711980140034,-25.7873288367412,-25.7034564600591,-25.6195896309072,
-25.5357007241138,-25.4559474592168,-25.3720617893132,-25.2881926120514,
-25.2043202353694,-25.1204534062176,-25.0365644994246,-24.9568112345263,
-24.8729255646225,-24.7890563873604,-24.7051840106786,-24.6213171815268,
-24.5374282747336,-24.4576750098358,-24.3737893399322,-24.2899201626703,
-24.2060477859883,-24.1221809568366,-24.0382920500434,-23.9585387851453,
-23.8746531152411,-23.7907839379782,-23.706911561296,-23.6230447321438,
-23.5391558253504,-23.4594025604547,-23.3755168905508,-23.2916477132885,
-23.2077753366064,-23.1239085074543,-23.040019600661,-22.9602663357642,
-22.9420976703771),.UNSPECIFIED.);
#254=B_SPLINE_CURVE_WITH_KNOTS('',3,(#15244,#15245,#15246,#15247,#15248,
#15249,#15250,#15251,#15252,#15253,#15254,#15255,#15256,#15257,#15258,#15259,
#15260,#15261,#15262,#15263,#15264,#15265,#15266,#15267,#15268,#15269,#15270,
#15271,#15272,#15273,#15274,#15275,#15276,#15277,#15278,#15279,#15280,#15281,
#15282,#15283,#15284,#15285,#15286,#15287,#15288,#15289,#15290,#15291,#15292,
#15293,#15294,#15295,#15296,#15297,#15298,#15299,#15300,#15301,#15302,#15303,
#15304,#15305,#15306,#15307,#15308,#15309,#15310,#15311,#15312,#15313,#15314,
#15315,#15316,#15317,#15318,#15319,#15320,#15321,#15322,#15323,#15324,#15325,
#15326,#15327,#15328,#15329,#15330,#15331,#15332,#15333,#15334,#15335,#15336,
#15337,#15338,#15339,#15340,#15341,#15342,#15343,#15344,#15345,#15346,#15347,
#15348,#15349,#15350,#15351,#15352,#15353,#15354,#15355,#15356,#15357,#15358,
#15359,#15360,#15361,#15362,#15363,#15364,#15365,#15366,#15367,#15368,#15369,
#15370,#15371,#15372,#15373,#15374,#15375,#15376,#15377,#15378,#15379,#15380,
#15381,#15382,#15383,#15384,#15385,#15386,#15387,#15388,#15389,#15390,#15391,
#15392,#15393,#15394,#15395,#15396,#15397,#15398,#15399,#15400,#15401,#15402,
#15403,#15404,#15405,#15406,#15407,#15408,#15409,#15410,#15411,#15412,#15413,
#15414,#15415,#15416,#15417,#15418,#15419,#15420,#15421,#15422,#15423,#15424,
#15425,#15426,#15427,#15428,#15429,#15430,#15431,#15432,#15433,#15434,#15435,
#15436,#15437,#15438,#15439,#15440,#15441,#15442,#15443,#15444,#15445,#15446,
#15447,#15448,#15449,#15450,#15451,#15452,#15453,#15454,#15455,#15456,#15457,
#15458,#15459,#15460,#15461,#15462,#15463,#15464,#15465,#15466,#15467,#15468,
#15469,#15470,#15471,#15472),.UNSPECIFIED.,.F.,.F.,(4,3,3,3,3,3,3,3,3,3,
3,3,3,3,3,3,3,3,3,3,3,3,3,3,3,3,3,3,3,3,3,3,3,3,3,3,3,3,3,3,3,3,3,3,3,3,
3,3,3,3,3,3,3,3,3,3,3,3,3,3,3,3,3,3,3,3,3,3,3,3,3,3,3,3,3,3,4),(19.9684110152191,
20.0521965060799,20.1359653468292,20.2197369128689,20.3035036871813,20.3872915667496,
20.4537493410731,20.5376364503445,20.6215070898444,20.705380927313,20.7892492291569,
20.8731395531138,20.9526212762212,21.0365083854925,21.1203790249926,21.2042528624611,
21.288121164305,21.3720114882618,21.4514932113693,21.5353803206406,21.6192509601403,
21.7031247976089,21.7869930994529,21.8708834234096,21.9503651465174,22.0342522557888,
22.1181228952888,22.2019967327576,22.2858650346016,22.3697553585586,22.4492370816656,
22.5331241909368,22.6169948304367,22.7008686679053,22.7847369697493,22.8686272937061,
22.9481090168137,23.031996126085,23.1158667655848,23.1997406030536,23.2836089048974,
23.3674992288542,23.4469809519618,23.5308680612332,23.6147387007327,23.6986125382014,
23.7824808400452,23.8663711640021,23.9458528871099,24.0297399963815,24.1136106358812,
24.1974844733501,24.2813527751942,24.3652430991513,24.4447248222581,24.5286119315294,
24.612482571029,24.6963564084977,24.7802247103415,24.8641150342984,24.9435967574062,
25.0274838666776,25.1113545061777,25.1952283436463,25.2790966454902,25.3629869694469,
25.4424686925543,25.5263558018254,25.6102264413247,25.6941002787931,25.777968580637,
25.8618589045937,25.9413406277024,26.0254361266215,26.1095126610158,26.1935839844518,
26.2515963222561),.UNSPECIFIED.);
#255=B_SPLINE_CURVE_WITH_KNOTS('',3,(#15477,#15478,#15479,#15480,#15481,
#15482,#15483,#15484,#15485,#15486,#15487,#15488,#15489,#15490,#15491,#15492,
#15493,#15494,#15495,#15496,#15497,#15498,#15499,#15500,#15501,#15502,#15503,
#15504,#15505,#15506,#15507,#15508,#15509,#15510,#15511,#15512,#15513,#15514,
#15515,#15516,#15517,#15518,#15519,#15520,#15521,#15522,#15523,#15524,#15525,
#15526,#15527,#15528,#15529,#15530,#15531,#15532,#15533,#15534,#15535,#15536,
#15537,#15538,#15539,#15540,#15541,#15542,#15543,#15544,#15545,#15546,#15547,
#15548,#15549,#15550,#15551,#15552,#15553,#15554,#15555,#15556,#15557,#15558,
#15559,#15560,#15561,#15562,#15563,#15564,#15565,#15566,#15567,#15568,#15569,
#15570,#15571,#15572,#15573,#15574,#15575,#15576,#15577,#15578,#15579,#15580,
#15581,#15582,#15583,#15584,#15585,#15586,#15587,#15588,#15589,#15590,#15591,
#15592,#15593,#15594,#15595,#15596,#15597,#15598,#15599,#15600,#15601,#15602,
#15603,#15604,#15605,#15606,#15607,#15608,#15609,#15610,#15611,#15612,#15613,
#15614,#15615,#15616,#15617,#15618,#15619,#15620,#15621,#15622,#15623,#15624,
#15625,#15626,#15627,#15628,#15629,#15630,#15631,#15632,#15633,#15634,#15635,
#15636,#15637,#15638,#15639,#15640,#15641,#15642,#15643,#15644,#15645,#15646,
#15647,#15648,#15649,#15650,#15651,#15652,#15653,#15654,#15655,#15656,#15657,
#15658,#15659,#15660,#15661,#15662,#15663,#15664,#15665,#15666,#15667,#15668,
#15669,#15670,#15671,#15672,#15673,#15674,#15675,#15676,#15677,#15678,#15679,
#15680,#15681,#15682,#15683,#15684,#15685,#15686,#15687,#15688,#15689,#15690,
#15691,#15692,#15693,#15694,#15695,#15696,#15697,#15698,#15699,#15700,#15701,
#15702,#15703,#15704,#15705),.UNSPECIFIED.,.F.,.F.,(4,3,3,3,3,3,3,3,3,3,
3,3,3,3,3,3,3,3,3,3,3,3,3,3,3,3,3,3,3,3,3,3,3,3,3,3,3,3,3,3,3,3,3,3,3,3,
3,3,3,3,3,3,3,3,3,3,3,3,3,3,3,3,3,3,3,3,3,3,3,3,3,3,3,3,3,3,4),(-35.5084682847362,
-35.4386719530274,-35.3547862831221,-35.2709171058588,-35.1870447291753,
-35.103177900022,-35.0192889932272,-34.9395357283368,-34.8556500584337,
-34.7717808811724,-34.687908504491,-34.60404167534,-34.5201527685474,-34.4403995036463,
-34.3565138337424,-34.2726446564803,-34.1887722797983,-34.1049054506465,
-34.0210165438532,-33.9412632789558,-33.8573776090521,-33.7735084317902,
-33.6896360551083,-33.6057692259566,-33.5218803191635,-33.4421270542653,
-33.3582413843614,-33.2743722070994,-33.1904998304174,-33.1066330012656,
-33.0227440944724,-32.9429908295747,-32.8591051596709,-32.775235982409,
-32.6913636057271,-32.6074967765754,-32.5236078697822,-32.4438546048842,
-32.3599689349805,-32.2760997577186,-32.1922273810368,-32.1083605518851,
-32.024471645092,-31.9447183801937,-31.86083271029,-31.7769635330281,-31.6930911563462,
-31.6092243271946,-31.5253354204015,-31.4455821555032,-31.3616964855993,
-31.2778273083373,-31.1939549316552,-31.1100881025034,-31.0261991957101,
-30.9464459308126,-30.8625602609089,-30.778691083647,-30.6948187069651,
-30.6109518778135,-30.5270629710203,-30.4473097061221,-30.3634240362183,
-30.2795548589565,-30.1956824822747,-30.1118156531231,-30.0279267463299,
-29.9481734814316,-29.8642878115278,-29.7804186342659,-29.696546257584,
-29.6126794284323,-29.5287905216391,-29.4490372567411,-29.363612783768,
-29.278209766101,-29.2252829777188),.UNSPECIFIED.);
#256=B_SPLINE_CURVE_WITH_KNOTS('',3,(#15706,#15707,#15708,#15709,#15710,
#15711,#15712,#15713,#15714,#15715,#15716,#15717,#15718,#15719,#15720,#15721,
#15722),.UNSPECIFIED.,.F.,.F.,(4,1,1,1,1,1,1,1,1,1,1,1,1,1,4),(26.2515963581132,
26.4402125628506,26.9390844979987,27.4379564331468,27.9368283682949,28.4357003034431,
28.9345722385912,29.4334441737393,29.9323161088874,30.4311880440356,30.9300599791837,
31.4289319143318,31.9278038494799,32.4266757846281,32.5347816294356),
 .UNSPECIFIED.);
#257=B_SPLINE_CURVE_WITH_KNOTS('',3,(#15727,#15728,#15729,#15730,#15731,
#15732,#15733,#15734,#15735,#15736,#15737,#15738,#15739,#15740,#15741,#15742),
 .UNSPECIFIED.,.F.,.F.,(4,1,1,1,1,1,1,1,1,1,1,1,1,4),(-41.7916535919158,
-41.4283066493137,-40.9291704246232,-40.4300341999326,-39.9308979752421,
-39.4317617505516,-38.9326255258611,-38.4334893011705,-37.93435307648,-37.4352168517895,
-36.9360806270989,-36.4369444024084,-35.9378081777179,-35.5084683183979),
 .UNSPECIFIED.);
#258=B_SPLINE_CURVE_WITH_KNOTS('',3,(#15743,#15744,#15745,#15746,#15747,
#15748,#15749,#15750,#15751,#15752,#15753,#15754,#15755,#15756,#15757,#15758,
#15759,#15760,#15761,#15762,#15763,#15764,#15765,#15766,#15767,#15768,#15769,
#15770,#15771,#15772,#15773,#15774,#15775,#15776,#15777,#15778,#15779,#15780,
#15781,#15782,#15783,#15784,#15785,#15786,#15787,#15788,#15789,#15790,#15791,
#15792,#15793,#15794,#15795,#15796,#15797,#15798,#15799,#15800,#15801,#15802,
#15803,#15804,#15805,#15806,#15807,#15808,#15809,#15810,#15811,#15812,#15813,
#15814,#15815,#15816,#15817,#15818,#15819,#15820,#15821,#15822,#15823,#15824,
#15825,#15826,#15827,#15828,#15829,#15830,#15831,#15832,#15833,#15834,#15835,
#15836,#15837,#15838,#15839,#15840,#15841,#15842,#15843,#15844,#15845,#15846,
#15847,#15848,#15849,#15850,#15851,#15852,#15853,#15854,#15855,#15856,#15857,
#15858,#15859,#15860,#15861,#15862,#15863,#15864,#15865,#15866,#15867,#15868,
#15869,#15870,#15871,#15872,#15873,#15874,#15875,#15876,#15877,#15878,#15879,
#15880,#15881,#15882,#15883,#15884,#15885,#15886,#15887,#15888,#15889,#15890,
#15891,#15892,#15893,#15894,#15895,#15896,#15897,#15898,#15899,#15900,#15901,
#15902,#15903,#15904,#15905,#15906,#15907,#15908,#15909,#15910,#15911,#15912,
#15913,#15914,#15915,#15916,#15917,#15918,#15919,#15920,#15921,#15922,#15923,
#15924,#15925,#15926,#15927,#15928,#15929,#15930,#15931,#15932,#15933,#15934,
#15935,#15936,#15937,#15938,#15939,#15940,#15941,#15942,#15943,#15944,#15945,
#15946,#15947,#15948,#15949,#15950,#15951,#15952,#15953,#15954,#15955,#15956,
#15957,#15958,#15959,#15960,#15961,#15962,#15963,#15964,#15965,#15966,#15967,
#15968,#15969,#15970,#15971),.UNSPECIFIED.,.F.,.F.,(4,3,3,3,3,3,3,3,3,3,
3,3,3,3,3,3,3,3,3,3,3,3,3,3,3,3,3,3,3,3,3,3,3,3,3,3,3,3,3,3,3,3,3,3,3,3,
3,3,3,3,3,3,3,3,3,3,3,3,3,3,3,3,3,3,3,3,3,3,3,3,3,3,3,3,3,3,4),(32.5347816294356,
32.618344792917,32.7019091144161,32.7854688123165,32.8690491961098,32.9255477197762,
33.0094348290475,33.0933054685473,33.177179306016,33.2610476078598,33.3449379318165,
33.4244196549243,33.5083067641954,33.5921774036951,33.6760512411636,33.7599195430073,
33.8438098669641,33.9232915900724,34.0071786993439,34.0910493388438,34.1749231763126,
34.2587914781565,34.3426818021134,34.4221635252206,34.5060506344918,34.5899212739919,
34.6737951114604,34.7576634133044,34.8415537372611,34.9210354603687,35.0049225696402,
35.0887932091399,35.1726670466086,35.2565353484524,35.3404256724092,35.4199073955168,
35.5037945047881,35.587665144288,35.6715389817566,35.7554072836003,35.8392976075571,
35.9187793306649,36.0026664399364,36.0865370794367,36.1704109169056,36.2542792187495,
36.3381695427065,36.4176512658131,36.5015383750845,36.5854090145842,36.6692828520528,
36.7531511538964,36.8370414778532,36.9165232009612,37.0004103102327,37.0842809497323,
37.1681547872009,37.2520230890448,37.3359134130015,37.4153951361093,37.4992822453806,
37.5831528848803,37.667026722349,37.7508950241926,37.8347853481493,37.9142670712574,
37.9981541805289,38.0820248200289,38.1658986574978,38.2497669593422,38.3336572832991,
38.4131390064056,38.4966936713022,38.5802388631689,38.663772774134,38.7473200173164,
38.8179669364678),.UNSPECIFIED.);
#259=B_SPLINE_CURVE_WITH_KNOTS('',3,(#15976,#15977,#15978,#15979,#15980,
#15981,#15982,#15983,#15984,#15985,#15986,#15987,#15988,#15989,#15990,#15991,
#15992),.UNSPECIFIED.,.F.,.F.,(4,1,1,1,1,1,1,1,1,1,1,1,1,1,4),(-48.0748388990954,
-47.9170775702905,-47.4179413456,-46.9188051209095,-46.419668896219,-45.9205326715284,
-45.4213964468379,-44.9222602221474,-44.4231239974569,-43.9239877727663,
-43.4248515480758,-42.9257153233853,-42.4265790986947,-41.9274428740042,
-41.7916535919158),.UNSPECIFIED.);
#260=B_SPLINE_CURVE_WITH_KNOTS('',3,(#15993,#15994,#15995,#15996,#15997,
#15998,#15999,#16000,#16001,#16002,#16003,#16004,#16005,#16006,#16007,#16008,
#16009,#16010,#16011,#16012,#16013,#16014,#16015,#16016,#16017,#16018,#16019,
#16020,#16021,#16022,#16023,#16024,#16025,#16026,#16027,#16028,#16029,#16030,
#16031,#16032,#16033,#16034,#16035,#16036,#16037,#16038,#16039,#16040,#16041,
#16042,#16043,#16044,#16045,#16046,#16047,#16048,#16049,#16050,#16051,#16052,
#16053,#16054,#16055,#16056,#16057,#16058,#16059,#16060,#16061,#16062,#16063,
#16064,#16065,#16066,#16067,#16068,#16069,#16070,#16071,#16072,#16073,#16074,
#16075,#16076,#16077,#16078,#16079,#16080,#16081,#16082,#16083,#16084,#16085,
#16086,#16087,#16088,#16089,#16090,#16091,#16092,#16093,#16094,#16095,#16096,
#16097,#16098,#16099,#16100,#16101,#16102,#16103,#16104,#16105,#16106,#16107,
#16108,#16109,#16110,#16111,#16112,#16113,#16114,#16115,#16116,#16117,#16118,
#16119,#16120,#16121,#16122,#16123,#16124,#16125,#16126,#16127,#16128,#16129,
#16130,#16131,#16132,#16133,#16134,#16135,#16136,#16137,#16138,#16139,#16140,
#16141,#16142,#16143,#16144,#16145,#16146,#16147,#16148,#16149,#16150,#16151,
#16152,#16153,#16154,#16155,#16156,#16157,#16158,#16159,#16160,#16161,#16162,
#16163,#16164,#16165,#16166,#16167,#16168,#16169,#16170,#16171,#16172,#16173,
#16174,#16175,#16176,#16177,#16178,#16179,#16180,#16181,#16182,#16183,#16184,
#16185,#16186,#16187,#16188,#16189,#16190,#16191,#16192,#16193,#16194,#16195,
#16196,#16197,#16198,#16199,#16200,#16201,#16202,#16203,#16204,#16205,#16206,
#16207,#16208,#16209,#16210,#16211,#16212,#16213,#16214,#16215,#16216,#16217,
#16218,#16219,#16220,#16221),.UNSPECIFIED.,.F.,.F.,(4,3,3,3,3,3,3,3,3,3,
3,3,3,3,3,3,3,3,3,3,3,3,3,3,3,3,3,3,3,3,3,3,3,3,3,3,3,3,3,3,3,3,3,3,3,3,
3,3,3,3,3,3,3,3,3,3,3,3,3,3,3,3,3,3,3,3,3,3,3,3,3,3,3,3,3,3,4),(38.8179669366152,
38.9120109415537,38.9958980508245,39.0797686903237,39.1636425277917,39.2475108296349,
39.3314011535911,39.4108828767018,39.4947699859733,39.5786406254735,39.6625144629423,
39.7463827647863,39.8302730887433,39.9097548118499,39.9936419211213,40.0775125606213,
40.16138639809,40.245254699934,40.3291450238909,40.4086267469981,40.4925138562694,
40.5763844957693,40.6602583332379,40.7441266350817,40.8280169590385,40.9074986821462,
40.9913857914176,41.0752564309173,41.159130268386,41.2429985702298,41.3268888941867,
41.4063706172943,41.4902577265657,41.5741283660655,41.6580022035341,41.741870505378,
41.8257608293349,41.9052425524424,41.9891296617137,42.0730003012134,42.1568741386819,
42.2407424405257,42.3246327644825,42.4041144875905,42.488001596862,42.571872236362,
42.6557460738308,42.7396143756748,42.8235046996318,42.9029864227387,42.98687353201,
43.0707441715098,43.1546180089784,43.2384863108222,43.322376634779,43.4018583578868,
43.4857454671581,43.5696161066578,43.6534899441264,43.7373582459703,43.8212485699271,
43.9007302930349,43.9846174023063,44.0684880418061,44.1523618792748,44.2362301811186,
44.3201205050754,44.399602228183,44.4834893374546,44.5673599769545,44.6512338144233,
44.7351021162673,44.8189924402242,44.8984741633312,44.984359198492,45.0702196443385,
45.1011522436613),.UNSPECIFIED.);
#261=B_SPLINE_CURVE_WITH_KNOTS('',3,(#16226,#16227,#16228,#16229,#16230,
#16231,#16232,#16233,#16234,#16235,#16236,#16237,#16238,#16239,#16240,#16241),
 .UNSPECIFIED.,.F.,.F.,(4,1,1,1,1,1,1,1,1,1,1,1,1,4),(-54.358024206275,
-53.9067122665769,-53.4075760418863,-52.9084398171958,-52.4093035925053,
-51.9101673678147,-51.4110311431242,-50.9118949184337,-50.4127586937432,
-49.9136224690526,-49.4144862443621,-48.9153500196716,-48.4162137949811,
-48.0748388990954),.UNSPECIFIED.);
#262=B_SPLINE_CURVE_WITH_KNOTS('',3,(#16242,#16243,#16244,#16245,#16246,
#16247,#16248,#16249,#16250,#16251,#16252,#16253,#16254,#16255,#16256,#16257,
#16258,#16259,#16260,#16261,#16262,#16263,#16264,#16265,#16266,#16267,#16268,
#16269,#16270,#16271,#16272,#16273,#16274,#16275,#16276,#16277,#16278,#16279,
#16280,#16281,#16282,#16283,#16284,#16285,#16286,#16287,#16288,#16289,#16290,
#16291,#16292,#16293,#16294,#16295,#16296,#16297,#16298,#16299,#16300,#16301,
#16302,#16303,#16304,#16305,#16306,#16307,#16308,#16309,#16310,#16311,#16312,
#16313,#16314,#16315,#16316,#16317,#16318,#16319,#16320,#16321,#16322,#16323,
#16324,#16325,#16326,#16327,#16328,#16329,#16330,#16331,#16332,#16333,#16334,
#16335,#16336,#16337,#16338,#16339,#16340,#16341,#16342,#16343,#16344,#16345,
#16346,#16347,#16348,#16349,#16350,#16351,#16352,#16353,#16354,#16355,#16356,
#16357,#16358,#16359,#16360,#16361,#16362,#16363,#16364,#16365,#16366,#16367,
#16368,#16369,#16370,#16371,#16372,#16373,#16374,#16375,#16376,#16377,#16378,
#16379,#16380,#16381,#16382,#16383,#16384,#16385,#16386,#16387,#16388,#16389,
#16390,#16391,#16392,#16393,#16394,#16395,#16396,#16397,#16398,#16399,#16400,
#16401,#16402,#16403,#16404,#16405,#16406,#16407,#16408,#16409,#16410,#16411,
#16412,#16413,#16414,#16415,#16416,#16417,#16418,#16419,#16420,#16421,#16422,
#16423,#16424,#16425,#16426,#16427,#16428,#16429,#16430,#16431,#16432,#16433,
#16434,#16435,#16436,#16437,#16438,#16439,#16440,#16441,#16442,#16443,#16444,
#16445,#16446,#16447,#16448,#16449,#16450,#16451,#16452,#16453,#16454,#16455,
#16456,#16457,#16458,#16459,#16460,#16461,#16462,#16463,#16464,#16465,#16466,
#16467,#16468,#16469,#16470),.UNSPECIFIED.,.F.,.F.,(4,3,3,3,3,3,3,3,3,3,
3,3,3,3,3,3,3,3,3,3,3,3,3,3,3,3,3,3,3,3,3,3,3,3,3,3,3,3,3,3,3,3,3,3,3,3,
3,3,3,3,3,3,3,3,3,3,3,3,3,3,3,3,3,3,3,3,3,3,3,3,3,3,3,3,3,3,4),(45.1011522437948,
45.1853822629713,45.2696128695901,45.3538646416685,45.3973460984793,45.4812332077506,
45.5651038472503,45.6489776847188,45.7328459865627,45.8167363105194,45.8962180336274,
45.9801051428987,46.0639757823986,46.1478496198672,46.231717921711,46.3156082456678,
46.3950899687755,46.4789770780471,46.5628477175468,46.6467215550156,46.7305898568594,
46.8144801808164,46.8939619039237,46.9778490131949,47.0617196526949,47.1455934901634,
47.2294617920072,47.313352115964,47.3928338390718,47.4767209483433,47.5605915878429,
47.6444654253115,47.7283337271555,47.8122240511123,47.8917057742199,47.9755928834914,
48.0594635229913,48.1433373604599,48.2272056623041,48.3110959862609,48.390577709368,
48.4744648186397,48.5583354581401,48.6422092956089,48.7260775974526,48.8099679214096,
48.8894496445162,48.9733367537875,49.0572073932872,49.1410812307558,49.2249495325996,
49.3088398565565,49.3883215796643,49.4722086889355,49.5560793284352,49.6399531659037,
49.7238214677474,49.8077117917041,49.8871935148124,49.9710806240838,50.0549512635837,
50.1388251010524,50.2226934028966,50.3065837268537,50.3860654499606,50.4699525592319,
50.5538231987315,50.6376970362001,50.7215653380443,50.8054556620009,50.8849373851087,
50.9688288180462,51.0527037957669,51.1365819974282,51.220454637499,51.3043493368271,
51.3843375509714),.UNSPECIFIED.);
#263=B_SPLINE_CURVE_WITH_KNOTS('',3,(#16475,#16476,#16477,#16478,#16479,
#16480,#16481,#16482,#16483,#16484,#16485,#16486,#16487,#16488,#16489,#16490,
#16491),.UNSPECIFIED.,.F.,.F.,(4,1,1,1,1,1,1,1,1,1,1,1,1,1,4),(-60.6412095134546,
-60.3954831875537,-59.8963469628632,-59.3972107381726,-58.8980745134821,
-58.3989382887916,-57.8998020641011,-57.4006658394105,-56.90152961472,-56.4023933900295,
-55.903257165339,-55.4041209406484,-54.9049847159579,-54.4058484912674,
-54.358024206275),.UNSPECIFIED.);
#264=B_SPLINE_CURVE_WITH_KNOTS('',3,(#16492,#16493,#16494,#16495,#16496,
#16497,#16498,#16499,#16500,#16501,#16502,#16503,#16504,#16505,#16506,#16507,
#16508,#16509,#16510,#16511,#16512,#16513,#16514,#16515,#16516,#16517,#16518,
#16519,#16520,#16521,#16522,#16523,#16524,#16525,#16526,#16527,#16528,#16529,
#16530,#16531,#16532,#16533,#16534,#16535,#16536,#16537,#16538,#16539,#16540,
#16541,#16542,#16543,#16544,#16545,#16546,#16547,#16548,#16549,#16550,#16551,
#16552,#16553,#16554,#16555,#16556,#16557,#16558,#16559,#16560,#16561,#16562,
#16563,#16564,#16565,#16566,#16567,#16568,#16569,#16570,#16571,#16572,#16573,
#16574,#16575,#16576,#16577,#16578,#16579,#16580,#16581,#16582,#16583,#16584,
#16585,#16586,#16587,#16588,#16589,#16590,#16591,#16592,#16593,#16594,#16595,
#16596,#16597,#16598,#16599,#16600,#16601,#16602,#16603,#16604,#16605,#16606,
#16607,#16608,#16609,#16610,#16611,#16612,#16613,#16614,#16615,#16616,#16617,
#16618,#16619,#16620,#16621,#16622,#16623,#16624,#16625,#16626,#16627,#16628,
#16629,#16630,#16631,#16632,#16633,#16634,#16635,#16636,#16637,#16638,#16639,
#16640,#16641,#16642,#16643,#16644,#16645,#16646,#16647,#16648,#16649,#16650,
#16651,#16652,#16653,#16654,#16655,#16656,#16657,#16658,#16659,#16660,#16661,
#16662,#16663,#16664,#16665,#16666,#16667,#16668,#16669,#16670,#16671,#16672,
#16673,#16674,#16675,#16676,#16677,#16678,#16679,#16680,#16681,#16682,#16683,
#16684,#16685,#16686,#16687,#16688,#16689,#16690,#16691,#16692,#16693,#16694,
#16695,#16696,#16697,#16698,#16699,#16700,#16701,#16702,#16703,#16704,#16705,
#16706,#16707,#16708,#16709,#16710,#16711,#16712,#16713,#16714,#16715,#16716,
#16717,#16718,#16719,#16720),.UNSPECIFIED.,.F.,.F.,(4,3,3,3,3,3,3,3,3,3,
3,3,3,3,3,3,3,3,3,3,3,3,3,3,3,3,3,3,3,3,3,3,3,3,3,3,3,3,3,3,3,3,3,3,3,3,
3,3,3,3,3,3,3,3,3,3,3,3,3,3,3,3,3,3,3,3,3,3,3,3,3,3,3,3,3,3,4),(51.3843375509763,
51.4682203639788,51.5520866930172,51.6359561942946,51.7198201859624,51.8037061623815,
51.8826812554049,51.9665683646764,52.0504390041763,52.134312841645,52.218181143489,
52.3020714674459,52.3815531905531,52.4654402998244,52.5493109393242,52.6331847767927,
52.7170530786366,52.8009434025933,52.8804251257012,52.9643122349725,53.0481828744723,
53.1320567119409,53.2159250137848,53.2998153377415,53.3792970608493,53.4631841701207,
53.5470548096206,53.6309286470893,53.7147969489332,53.79868727289,53.8781689959974,
53.9620561052687,54.0459267447684,54.129800582237,54.2136688840808,54.2975592080375,
54.3770409311455,54.460928040417,54.544798679917,54.6286725173858,54.7125408192299,
54.7964311431868,54.8759128662937,54.959799975565,55.0436706150647,55.1275444525333,
55.2114127543771,55.2953030783338,55.3747848014418,55.4586719107132,55.542542550213,
55.6264163876816,55.7102846895255,55.7941750134823,55.8736567365899,55.9575438458613,
56.0414144853612,56.1252883228298,56.2091566246738,56.2930469486307,56.372528671738,
56.4564157810092,56.5402864205089,56.6241602579774,56.7080285598212,56.7919188837779,
56.8714006068861,56.9552877161577,57.0391583556578,57.1230321931266,57.2069004949706,
57.2907908189276,57.3702725420343,57.4545129399576,57.53873434292,57.6229476551049,
57.667522858154),.UNSPECIFIED.);
#265=B_SPLINE_CURVE_WITH_KNOTS('',3,(#16725,#16726,#16727,#16728,#16729,
#16730,#16731,#16732,#16733,#16734,#16735,#16736,#16737,#16738,#16739,#16740,
#16741,#16742,#16743,#16744,#16745,#16746,#16747,#16748,#16749,#16750,#16751,
#16752,#16753,#16754,#16755,#16756,#16757,#16758,#16759,#16760,#16761,#16762,
#16763,#16764,#16765,#16766,#16767,#16768,#16769,#16770,#16771,#16772,#16773,
#16774,#16775,#16776,#16777,#16778,#16779,#16780,#16781,#16782,#16783,#16784,
#16785,#16786,#16787,#16788,#16789,#16790,#16791,#16792,#16793,#16794,#16795,
#16796,#16797,#16798,#16799,#16800,#16801,#16802,#16803,#16804,#16805,#16806,
#16807,#16808,#16809,#16810,#16811,#16812,#16813,#16814,#16815,#16816,#16817,
#16818,#16819,#16820,#16821,#16822,#16823,#16824,#16825,#16826,#16827,#16828,
#16829,#16830,#16831,#16832,#16833,#16834,#16835,#16836,#16837,#16838,#16839,
#16840,#16841,#16842,#16843,#16844,#16845,#16846,#16847,#16848,#16849,#16850,
#16851,#16852,#16853,#16854,#16855,#16856,#16857,#16858,#16859,#16860,#16861,
#16862,#16863,#16864,#16865,#16866,#16867,#16868,#16869,#16870,#16871,#16872,
#16873,#16874,#16875,#16876,#16877,#16878,#16879,#16880,#16881,#16882,#16883,
#16884,#16885,#16886,#16887,#16888,#16889,#16890,#16891,#16892,#16893,#16894,
#16895,#16896,#16897,#16898,#16899,#16900,#16901,#16902,#16903,#16904,#16905,
#16906,#16907,#16908,#16909,#16910,#16911,#16912,#16913,#16914,#16915,#16916,
#16917,#16918,#16919,#16920,#16921,#16922,#16923,#16924,#16925,#16926,#16927,
#16928,#16929,#16930,#16931,#16932,#16933,#16934,#16935,#16936,#16937,#16938,
#16939,#16940,#16941,#16942,#16943,#16944,#16945,#16946,#16947,#16948,#16949,
#16950,#16951,#16952,#16953),.UNSPECIFIED.,.F.,.F.,(4,3,3,3,3,3,3,3,3,3,
3,3,3,3,3,3,3,3,3,3,3,3,3,3,3,3,3,3,3,3,3,3,3,3,3,3,3,3,3,3,3,3,3,3,3,3,
3,3,3,3,3,3,3,3,3,3,3,3,3,3,3,3,3,3,3,3,3,3,3,3,3,3,3,3,3,3,4),(-66.9243948206342,
-66.8842541085305,-66.8003684386284,-66.7164992613681,-66.6326268846879,
-66.5487600555379,-66.4648711487464,-66.38511788384,-66.3012322139357,-66.2173630366733,
-66.1334906599908,-66.0496238308386,-65.9657349240449,-65.8859816591495,
-65.8020959892458,-65.718226811984,-65.6343544353021,-65.5504876061504,
-65.4665986993573,-65.3868454344589,-65.3029597645552,-65.2190905872933,
-65.1352182106114,-65.0513513814597,-64.9674624746665,-64.8877092097684,
-64.8038235398646,-64.7199543626027,-64.6360819859208,-64.552215156769,
-64.4683262499758,-64.3885729850779,-64.3046873151741,-64.2208181379122,
-64.1369457612303,-64.0530789320785,-63.9691900252854,-63.8894367603874,
-63.8055510904837,-63.7216819132219,-63.6378095365401,-63.5539427073885,
-63.4700538005955,-63.3903005356969,-63.306414865793,-63.2225456885309,
-63.1386733118488,-63.0548064826969,-62.9709175759036,-62.8911643110063,
-62.8072786411026,-62.7234094638407,-62.6395370871588,-62.5556702580072,
-62.4717813512141,-62.3920280863158,-62.308142416412,-62.2242732391502,
-62.1404008624683,-62.0565340333166,-61.9726451265235,-61.8928918616253,
-61.8090061917216,-61.7251370144597,-61.6412646377777,-61.5573978086262,
-61.4735089018331,-61.3937556369348,-61.309869967031,-61.2260007897689,
-61.1421284130868,-61.058261583935,-60.9743726771418,-60.8946194122442,
-60.8097498638457,-60.7248961180713,-60.6412095136835),.UNSPECIFIED.);
#266=B_SPLINE_CURVE_WITH_KNOTS('',3,(#16954,#16955,#16956,#16957,#16958,
#16959,#16960,#16961,#16962,#16963,#16964,#16965,#16966,#16967,#16968,#16969,
#16970,#16971,#16972,#16973,#16974,#16975,#16976,#16977,#16978,#16979,#16980,
#16981,#16982,#16983,#16984,#16985,#16986,#16987,#16988,#16989,#16990,#16991,
#16992,#16993,#16994,#16995,#16996,#16997,#16998,#16999,#17000,#17001,#17002,
#17003,#17004,#17005,#17006,#17007,#17008,#17009,#17010,#17011,#17012,#17013,
#17014,#17015,#17016,#17017,#17018,#17019,#17020,#17021,#17022,#17023,#17024,
#17025,#17026,#17027,#17028,#17029,#17030,#17031,#17032,#17033,#17034,#17035,
#17036,#17037,#17038,#17039,#17040,#17041,#17042,#17043,#17044,#17045,#17046,
#17047,#17048,#17049,#17050,#17051,#17052,#17053,#17054,#17055,#17056,#17057,
#17058,#17059,#17060,#17061,#17062,#17063,#17064,#17065,#17066,#17067,#17068,
#17069,#17070,#17071,#17072,#17073,#17074,#17075,#17076,#17077,#17078,#17079,
#17080,#17081,#17082,#17083,#17084,#17085,#17086,#17087,#17088,#17089,#17090,
#17091,#17092,#17093,#17094,#17095,#17096,#17097,#17098,#17099,#17100,#17101,
#17102,#17103,#17104,#17105,#17106,#17107,#17108,#17109,#17110,#17111,#17112,
#17113,#17114,#17115,#17116,#17117,#17118,#17119,#17120,#17121,#17122,#17123,
#17124,#17125,#17126,#17127,#17128,#17129,#17130,#17131,#17132,#17133,#17134,
#17135,#17136,#17137,#17138,#17139,#17140,#17141,#17142,#17143,#17144,#17145,
#17146,#17147,#17148,#17149,#17150,#17151,#17152,#17153,#17154,#17155,#17156,
#17157,#17158,#17159,#17160,#17161,#17162,#17163,#17164,#17165,#17166,#17167,
#17168,#17169,#17170,#17171,#17172,#17173,#17174,#17175,#17176,#17177,#17178,
#17179,#17180,#17181,#17182,#17183,#17184,#17185),.UNSPECIFIED.,.F.,.F.,
(4,3,3,3,3,3,3,3,3,3,3,3,3,3,3,3,3,3,3,3,3,3,3,3,3,3,3,3,3,3,3,3,3,3,3,
3,3,3,3,3,3,3,3,3,3,3,3,3,3,3,3,3,3,3,3,3,3,3,3,3,3,3,3,3,3,3,3,3,3,3,3,
3,3,3,3,3,3,4),(57.6675228582893,57.7534041072256,57.8393136045471,57.8691444771824,
57.9530315864536,58.0369022259531,58.1207760634215,58.2046443652652,58.2885346892219,
58.3680164123305,58.4519035216018,58.5357741611016,58.6196479985702,58.703516300414,
58.7874066243708,58.8668883474786,58.9507754567501,59.0346460962501,59.1185199337189,
59.2023882355629,59.2862785595198,59.3657602826268,59.4496473918981,59.5335180313978,
59.6173918688663,59.7012601707101,59.7851504946669,59.8646322177749,59.9485193270462,
60.032389966546,60.1162638040146,60.2001321058585,60.2840224298153,60.363504152923,
60.4473912621943,60.5312619016941,60.6151357391627,60.6990040410066,60.7828943649633,
60.8623760880711,60.9462631973426,61.0301338368426,61.1140076743113,61.1978759761554,
61.2817663001124,61.3612480232193,61.4451351324906,61.5290057719904,61.612879609459,
61.6967479113029,61.7806382352596,61.8601199583674,61.9440070676387,62.0278777071385,
62.1117515446071,62.1956198464509,62.2795101704077,62.3589918935155,62.4428790027869,
62.5267496422866,62.6106234797552,62.6944917815991,62.7783821055559,62.8578638286636,
62.9417509379351,63.0256215774348,63.1094954149035,63.1933637167476,63.2772540407045,
63.3567357638118,63.4406228730832,63.524493512583,63.6083673500517,63.6922356518955,
63.7761259758523,63.8556076989599,63.9449408103947,63.9507081653336),
 .UNSPECIFIED.);
#267=B_SPLINE_CURVE_WITH_KNOTS('',3,(#17190,#17191,#17192,#17193,#17194,
#17195,#17196,#17197,#17198,#17199,#17200,#17201,#17202,#17203,#17204,#17205,
#17206,#17207,#17208,#17209,#17210,#17211,#17212,#17213,#17214,#17215,#17216,
#17217,#17218,#17219,#17220,#17221,#17222,#17223,#17224,#17225,#17226,#17227,
#17228,#17229,#17230,#17231,#17232,#17233,#17234,#17235,#17236,#17237,#17238,
#17239,#17240,#17241,#17242,#17243,#17244,#17245,#17246,#17247,#17248,#17249,
#17250,#17251,#17252,#17253,#17254,#17255,#17256,#17257,#17258,#17259,#17260,
#17261,#17262,#17263,#17264,#17265,#17266,#17267,#17268,#17269,#17270,#17271,
#17272,#17273,#17274,#17275,#17276,#17277,#17278,#17279,#17280,#17281,#17282,
#17283,#17284,#17285,#17286,#17287,#17288,#17289,#17290,#17291,#17292,#17293,
#17294,#17295,#17296,#17297,#17298,#17299,#17300,#17301,#17302,#17303,#17304,
#17305,#17306,#17307,#17308,#17309,#17310,#17311,#17312,#17313,#17314,#17315,
#17316,#17317,#17318,#17319,#17320,#17321,#17322,#17323,#17324,#17325,#17326,
#17327,#17328,#17329,#17330,#17331,#17332,#17333,#17334,#17335,#17336,#17337,
#17338,#17339,#17340,#17341,#17342,#17343,#17344,#17345,#17346,#17347,#17348,
#17349,#17350,#17351,#17352,#17353,#17354,#17355,#17356,#17357,#17358,#17359,
#17360,#17361,#17362,#17363,#17364,#17365,#17366,#17367,#17368,#17369,#17370,
#17371,#17372,#17373,#17374,#17375,#17376,#17377,#17378,#17379,#17380,#17381,
#17382,#17383,#17384,#17385,#17386,#17387,#17388,#17389,#17390,#17391,#17392,
#17393,#17394,#17395,#17396,#17397,#17398,#17399,#17400,#17401,#17402,#17403,
#17404,#17405,#17406,#17407,#17408,#17409,#17410,#17411,#17412,#17413,#17414,
#17415,#17416,#17417,#17418),.UNSPECIFIED.,.F.,.F.,(4,3,3,3,3,3,3,3,3,3,
3,3,3,3,3,3,3,3,3,3,3,3,3,3,3,3,3,3,3,3,3,3,3,3,3,3,3,3,3,3,3,3,3,3,3,3,
3,3,3,3,3,3,3,3,3,3,3,3,3,3,3,3,3,3,3,3,3,3,3,3,3,3,3,3,3,3,4),(-73.2075801278138,
-73.1237189665367,-73.0398629051662,-72.9559834080525,-72.8738888048169,
-72.7900031349128,-72.7061339576504,-72.6222615809683,-72.5383947518164,
-72.454505845023,-72.3747525801263,-72.2908669102225,-72.2069977329604,
-72.1231253562785,-72.0392585271269,-71.9553696203339,-71.8756163554358,
-71.791730685532,-71.7078615082704,-71.6239891315887,-71.5401223024372,
-71.4562333956442,-71.3764801307453,-71.2925944608413,-71.208725283579,
-71.1248529068969,-71.0409860777452,-70.9570971709518,-70.8773439060547,
-70.7934582361511,-70.7095890588888,-70.6257166822069,-70.5418498530552,
-70.4579609462621,-70.3782076813642,-70.2943220114605,-70.2104528341989,
-70.1265804575169,-70.0427136283652,-69.958824721572,-69.8790714566737,
-69.79518578677,-69.7113166095082,-69.6274442328262,-69.5435774036746,-69.4596884968814,
-69.3799352319832,-69.2960495620793,-69.2121803848174,-69.1283080081353,
-69.0444411789833,-68.96055227219,-68.8807990072926,-68.7969133373889,-68.7130441601271,
-68.6291717834451,-68.5453049542936,-68.4614160475006,-68.3816627826021,
-68.2977771126984,-68.2139079354367,-68.1300355587546,-68.0461687296027,
-67.9622798228095,-67.8825265579116,-67.798640888008,-67.7147717107465,
-67.6308993340648,-67.547032504913,-67.4631435981197,-67.3833903332211,
-67.299752204125,-67.2161313803661,-67.1325096836612,-67.0488920048269,
-66.9652563514555,-66.9243948207875),.UNSPECIFIED.);
#268=B_SPLINE_CURVE_WITH_KNOTS('',3,(#17419,#17420,#17421,#17422,#17423,
#17424,#17425,#17426,#17427,#17428,#17429,#17430,#17431,#17432,#17433,#17434,
#17435,#17436,#17437,#17438,#17439,#17440,#17441,#17442,#17443,#17444,#17445,
#17446,#17447,#17448,#17449,#17450,#17451,#17452,#17453,#17454,#17455,#17456,
#17457,#17458,#17459,#17460,#17461,#17462,#17463,#17464,#17465,#17466,#17467,
#17468,#17469,#17470,#17471,#17472,#17473,#17474,#17475,#17476,#17477,#17478,
#17479,#17480,#17481,#17482,#17483,#17484,#17485,#17486,#17487,#17488,#17489,
#17490,#17491,#17492,#17493,#17494,#17495,#17496,#17497,#17498,#17499,#17500,
#17501,#17502,#17503,#17504,#17505,#17506,#17507,#17508,#17509,#17510,#17511,
#17512,#17513,#17514,#17515,#17516,#17517,#17518,#17519,#17520,#17521,#17522,
#17523,#17524,#17525,#17526,#17527,#17528,#17529,#17530,#17531,#17532,#17533,
#17534,#17535,#17536,#17537,#17538,#17539,#17540,#17541,#17542,#17543,#17544,
#17545,#17546,#17547,#17548,#17549,#17550,#17551,#17552,#17553,#17554,#17555,
#17556,#17557,#17558,#17559,#17560,#17561,#17562,#17563,#17564,#17565,#17566,
#17567,#17568,#17569,#17570,#17571,#17572,#17573,#17574,#17575,#17576,#17577,
#17578,#17579,#17580,#17581,#17582,#17583,#17584,#17585,#17586,#17587,#17588,
#17589,#17590,#17591,#17592,#17593,#17594,#17595,#17596,#17597,#17598,#17599,
#17600,#17601,#17602,#17603,#17604,#17605,#17606,#17607,#17608,#17609,#17610,
#17611,#17612,#17613,#17614,#17615,#17616,#17617,#17618,#17619,#17620,#17621,
#17622,#17623,#17624,#17625,#17626,#17627,#17628,#17629,#17630,#17631,#17632,
#17633,#17634,#17635,#17636,#17637,#17638,#17639,#17640,#17641,#17642,#17643,
#17644,#17645,#17646,#17647),.UNSPECIFIED.,.F.,.F.,(4,3,3,3,3,3,3,3,3,3,
3,3,3,3,3,3,3,3,3,3,3,3,3,3,3,3,3,3,3,3,3,3,3,3,3,3,3,3,3,3,3,3,3,3,3,3,
3,3,3,3,3,3,3,3,3,3,3,3,3,3,3,3,3,3,3,3,3,3,3,3,3,3,3,3,3,3,4),(63.9507081654737,
64.0342511929075,64.1177942057486,64.2013312260194,64.2848898688643,64.354479634108,
64.4383667433793,64.5222373828791,64.6061112203477,64.6899795221913,64.7738698461479,
64.8533515692561,64.9372386785277,65.0211093180277,65.1049831554964,65.1888514573402,
65.2727417812972,65.3522235044043,65.4361106136757,65.5199812531758,65.6038550906444,
65.6877233924882,65.771613716445,65.8510954395524,65.9349825488237,66.0188531883232,
66.1027270257919,66.1865953276358,66.2704856515926,66.3499673747005,66.4338544839719,
66.5177251234716,66.6015989609404,66.6854672627844,66.7693575867413,66.8488393098486,
66.93272641912,67.0165970586195,67.100470896088,67.1843391979319,67.2682295218888,
67.3477112449967,67.4315983542682,67.5154689937682,67.5993428312371,67.6832111330812,
67.7671014570381,67.8465831801449,67.9304702894162,68.0143409289157,68.0982147663844,
68.1820830682279,68.2659733921847,68.345455115293,68.4293422245644,68.5132128640643,
68.597086701533,68.6809550033769,68.7648453273338,68.8443270504411,68.9282141597127,
69.0120847992117,69.0959586366804,69.1798269385242,69.2637172624809,69.3431989855892,
69.4270860948607,69.5109567343604,69.594830571829,69.6786988736732,69.7625891976302,
69.8420709207374,69.9256471339678,70.0092127771835,70.0927671613274,70.1763321069992,
70.2338934725132),.UNSPECIFIED.);
#269=B_SPLINE_CURVE_WITH_KNOTS('',3,(#17652,#17653,#17654,#17655,#17656,
#17657,#17658,#17659,#17660,#17661,#17662,#17663,#17664,#17665,#17666,#17667,
#17668,#17669,#17670,#17671,#17672,#17673,#17674,#17675,#17676,#17677,#17678,
#17679,#17680,#17681,#17682,#17683,#17684,#17685,#17686,#17687,#17688,#17689,
#17690,#17691,#17692,#17693,#17694,#17695,#17696,#17697,#17698,#17699,#17700,
#17701,#17702,#17703,#17704,#17705,#17706,#17707,#17708,#17709,#17710,#17711,
#17712,#17713,#17714,#17715,#17716,#17717,#17718,#17719,#17720,#17721,#17722,
#17723,#17724,#17725,#17726,#17727,#17728,#17729,#17730,#17731,#17732,#17733,
#17734,#17735,#17736,#17737,#17738,#17739,#17740,#17741,#17742,#17743,#17744,
#17745,#17746,#17747,#17748,#17749,#17750,#17751,#17752,#17753,#17754,#17755,
#17756,#17757,#17758,#17759,#17760,#17761,#17762,#17763,#17764,#17765,#17766,
#17767,#17768,#17769,#17770,#17771,#17772,#17773,#17774,#17775,#17776,#17777,
#17778,#17779,#17780,#17781,#17782,#17783,#17784,#17785,#17786,#17787,#17788,
#17789,#17790,#17791,#17792,#17793,#17794,#17795,#17796,#17797,#17798,#17799,
#17800,#17801,#17802,#17803,#17804,#17805,#17806,#17807,#17808,#17809,#17810,
#17811,#17812,#17813,#17814,#17815,#17816,#17817,#17818,#17819,#17820,#17821,
#17822,#17823,#17824,#17825,#17826,#17827,#17828,#17829,#17830,#17831,#17832,
#17833,#17834,#17835,#17836,#17837,#17838,#17839,#17840,#17841,#17842,#17843,
#17844,#17845,#17846,#17847,#17848,#17849,#17850,#17851,#17852,#17853,#17854,
#17855,#17856,#17857,#17858,#17859,#17860,#17861,#17862,#17863,#17864,#17865,
#17866,#17867,#17868,#17869,#17870,#17871,#17872,#17873,#17874,#17875,#17876,
#17877,#17878,#17879,#17880),.UNSPECIFIED.,.F.,.F.,(4,3,3,3,3,3,3,3,3,3,
3,3,3,3,3,3,3,3,3,3,3,3,3,3,3,3,3,3,3,3,3,3,3,3,3,3,3,3,3,3,3,3,3,3,3,3,
3,3,3,3,3,3,3,3,3,3,3,3,3,3,3,3,3,3,3,3,3,3,3,3,3,3,3,3,3,3,4),(-79.4907654337011,
-79.4027074760698,-79.3626597257937,-79.2787740558902,-79.1949048786287,
-79.1110325019471,-79.0271656727957,-78.9432767660027,-78.8635235011032,
-78.7796378311995,-78.6957686539375,-78.6118962772556,-78.5280294481038,
-78.4441405413106,-78.3643872764127,-78.2805016065089,-78.1966324292469,
-78.1127600525649,-78.0288932234132,-77.9450043166199,-77.8652510517221,
-77.7813653818183,-77.6974962045565,-77.6136238278745,-77.5297569987229,
-77.4458680919298,-77.3661148270316,-77.2822291571279,-77.1983599798659,
-77.114487603184,-77.0306207740324,-76.9467318672392,-76.8669786023411,
-76.7830929324374,-76.6992237551755,-76.6153513784937,-76.531484549342,
-76.4475956425489,-76.3678423776506,-76.2839567077467,-76.2000875304846,
-76.1162151538024,-76.0323483246506,-75.9484594178572,-75.86870615296,-75.7848204830563,
-75.7009513057945,-75.6170789291127,-75.5332120999611,-75.449323193168,
-75.3695699282695,-75.2856842583658,-75.201815081104,-75.1179427044221,
-75.0340758752705,-74.9501869684774,-74.870433703579,-74.786548033675,-74.7026788564129,
-74.6188064797308,-74.5349396505789,-74.4510507437856,-74.3712974788884,
-74.2874118089847,-74.2035426317232,-74.1196702550413,-74.0358034258898,
-73.9519145190967,-73.8721612541979,-73.7882755842942,-73.7044064070323,
-73.6205340303503,-73.5366672011987,-73.4527782944055,-73.3730250295074,
-73.2861666536806,-73.2075801279635),.UNSPECIFIED.);
#270=B_SPLINE_CURVE_WITH_KNOTS('',3,(#17881,#17882,#17883,#17884,#17885,
#17886,#17887,#17888,#17889,#17890,#17891,#17892,#17893,#17894,#17895,#17896,
#17897),.UNSPECIFIED.,.F.,.F.,(4,1,1,1,1,1,1,1,1,1,1,1,1,1,4),(70.2338934725132,
70.3409428558855,70.8398147910336,71.3386867261817,71.8375586613299,72.336430596478,
72.8353025316261,73.3341744667742,73.8330464019223,74.3319183370705,74.8307902722186,
75.3296622073667,75.8285341425149,76.327406077663,76.517078744021),
 .UNSPECIFIED.);
#271=B_SPLINE_CURVE_WITH_KNOTS('',3,(#17902,#17903,#17904,#17905,#17906,
#17907,#17908,#17909,#17910,#17911,#17912,#17913,#17914,#17915,#17916,#17917),
 .UNSPECIFIED.,.F.,.F.,(4,1,1,1,1,1,1,1,1,1,1,1,1,4),(-85.7739507126178,
-85.35229442208,-84.8531581973895,-84.354021972699,-83.8548857480084,-83.3557495233179,
-82.8566132986274,-82.3574770739369,-81.8583408492463,-81.3592046245558,
-80.8600683998653,-80.3609321751748,-79.8617959504842,-79.4907654349934),
 .UNSPECIFIED.);
#272=B_SPLINE_CURVE_WITH_KNOTS('',3,(#17918,#17919,#17920,#17921,#17922,
#17923,#17924,#17925,#17926,#17927,#17928,#17929,#17930,#17931,#17932,#17933,
#17934,#17935,#17936,#17937,#17938,#17939,#17940,#17941,#17942,#17943,#17944,
#17945,#17946,#17947,#17948,#17949,#17950,#17951,#17952,#17953,#17954,#17955,
#17956,#17957,#17958,#17959,#17960,#17961,#17962,#17963,#17964,#17965,#17966,
#17967,#17968,#17969,#17970,#17971,#17972,#17973,#17974,#17975,#17976,#17977,
#17978,#17979,#17980,#17981,#17982,#17983,#17984,#17985,#17986,#17987,#17988,
#17989,#17990,#17991,#17992,#17993,#17994,#17995,#17996,#17997,#17998,#17999,
#18000,#18001,#18002,#18003,#18004,#18005,#18006,#18007,#18008,#18009,#18010,
#18011,#18012,#18013,#18014,#18015,#18016,#18017,#18018,#18019,#18020,#18021,
#18022,#18023,#18024,#18025,#18026,#18027,#18028,#18029,#18030,#18031,#18032,
#18033,#18034,#18035,#18036,#18037,#18038,#18039,#18040,#18041,#18042,#18043,
#18044,#18045,#18046,#18047,#18048,#18049,#18050,#18051,#18052,#18053,#18054,
#18055,#18056,#18057,#18058,#18059,#18060,#18061,#18062,#18063,#18064,#18065,
#18066,#18067,#18068,#18069,#18070,#18071,#18072,#18073,#18074,#18075,#18076,
#18077,#18078,#18079,#18080,#18081,#18082,#18083,#18084,#18085,#18086,#18087,
#18088,#18089,#18090,#18091,#18092,#18093,#18094,#18095,#18096,#18097,#18098,
#18099,#18100,#18101,#18102,#18103,#18104,#18105,#18106,#18107,#18108,#18109,
#18110,#18111,#18112,#18113,#18114,#18115,#18116,#18117,#18118,#18119,#18120,
#18121,#18122,#18123,#18124,#18125,#18126,#18127,#18128,#18129,#18130,#18131,
#18132,#18133,#18134,#18135,#18136,#18137,#18138,#18139,#18140,#18141,#18142,
#18143,#18144,#18145,#18146),.UNSPECIFIED.,.F.,.F.,(4,3,3,3,3,3,3,3,3,3,
3,3,3,3,3,3,3,3,3,3,3,3,3,3,3,3,3,3,3,3,3,3,3,3,3,3,3,3,3,3,3,3,3,3,3,3,
3,3,3,3,3,3,3,3,3,3,3,3,3,3,3,3,3,3,3,3,3,3,3,3,3,3,3,3,3,3,4),(76.5170787796928,
76.6011639019145,76.6852475777892,76.7693531117986,76.8262780128111,76.9101651220824,
76.9940357615821,77.0779095990506,77.1617779008945,77.2456682248513,77.3251499479592,
77.4090370572304,77.4929076967303,77.5767815341989,77.6606498360427,77.7445401599995,
77.8240218831073,77.9079089923787,77.9917796318787,78.0756534693475,78.1595217711914,
78.2434120951483,78.3228938182555,78.4067809275269,78.4906515670271,78.5745254044957,
78.6583937063397,78.7422840302966,78.8217657534036,78.905652862675,78.9895235021748,
79.0733973396434,79.1572656414872,79.241155965444,79.3206376885517,79.4045247978231,
79.4883954373227,79.5722692747913,79.6561375766353,79.740027900592,79.8195096236998,
79.9033967329711,79.9872673724711,80.07114120994,80.1550095117838,80.2388998357408,
80.318381558848,80.4022686681195,80.4861393076195,80.5700131450882,80.653881446932,
80.7377717708888,80.8172534939961,80.9011406032674,80.9850112427667,81.0688850802354,
81.1527533820793,81.236643706036,81.3161254291442,81.4000125384156,81.4838831779163,
81.5677570153852,81.6516253172292,81.735515641186,81.8149973642924,81.8988844735638,
81.9827551130635,82.0666289505322,82.1504972523764,82.2343875763332,82.3138692994405,
82.397662418436,82.4814387563788,82.5652176399422,82.6489915553591,82.7327864637313,
82.8002640868724),.UNSPECIFIED.);
#273=B_SPLINE_CURVE_WITH_KNOTS('',3,(#18151,#18152,#18153,#18154,#18155,
#18156,#18157,#18158,#18159,#18160,#18161,#18162,#18163,#18164,#18165,#18166,
#18167,#18168,#18169,#18170,#18171,#18172,#18173,#18174,#18175,#18176,#18177,
#18178,#18179,#18180,#18181,#18182,#18183,#18184,#18185,#18186,#18187,#18188,
#18189,#18190,#18191,#18192,#18193,#18194,#18195,#18196,#18197,#18198,#18199,
#18200,#18201,#18202,#18203,#18204,#18205,#18206,#18207,#18208,#18209,#18210,
#18211,#18212,#18213,#18214,#18215,#18216,#18217,#18218,#18219,#18220,#18221,
#18222,#18223,#18224,#18225,#18226,#18227,#18228,#18229,#18230,#18231,#18232,
#18233,#18234,#18235,#18236,#18237,#18238,#18239,#18240,#18241,#18242,#18243,
#18244,#18245,#18246,#18247,#18248,#18249,#18250,#18251,#18252,#18253,#18254,
#18255,#18256,#18257,#18258,#18259,#18260,#18261,#18262,#18263,#18264,#18265,
#18266,#18267,#18268,#18269,#18270,#18271,#18272,#18273,#18274,#18275,#18276,
#18277,#18278,#18279,#18280,#18281,#18282,#18283,#18284,#18285,#18286,#18287,
#18288,#18289,#18290,#18291,#18292,#18293,#18294,#18295,#18296,#18297,#18298,
#18299,#18300,#18301,#18302,#18303,#18304,#18305,#18306,#18307,#18308,#18309,
#18310,#18311,#18312,#18313,#18314,#18315,#18316,#18317,#18318,#18319,#18320,
#18321,#18322,#18323,#18324,#18325,#18326,#18327,#18328,#18329,#18330,#18331,
#18332,#18333,#18334,#18335,#18336,#18337,#18338,#18339,#18340,#18341,#18342,
#18343,#18344,#18345,#18346,#18347,#18348,#18349,#18350,#18351,#18352,#18353,
#18354,#18355,#18356,#18357,#18358,#18359,#18360,#18361,#18362,#18363,#18364,
#18365,#18366,#18367,#18368,#18369,#18370,#18371,#18372,#18373,#18374,#18375,
#18376,#18377,#18378,#18379),.UNSPECIFIED.,.F.,.F.,(4,3,3,3,3,3,3,3,3,3,
3,3,3,3,3,3,3,3,3,3,3,3,3,3,3,3,3,3,3,3,3,3,3,3,3,3,3,3,3,3,3,3,3,3,3,3,
3,3,3,3,3,3,3,3,3,3,3,3,3,3,3,3,3,3,3,3,3,3,3,3,3,3,3,3,3,3,4),(-92.0571360463357,
-91.9715779609207,-91.8859914371021,-91.8410653430568,-91.7571796731532,
-91.6733104958916,-91.5894381192099,-91.5055712900585,-91.4216823832656,
-91.3419291183663,-91.2580434484625,-91.1741742712005,-91.0903018945185,
-91.0064350653667,-90.9225461585735,-90.8427928936758,-90.7589072237721,
-90.6750380465103,-90.5911656698284,-90.5072988406768,-90.4234099338837,
-90.3436566689853,-90.2597709990815,-90.1759018218195,-90.0920294451375,
-90.0081626159857,-89.9242737091924,-89.8445204442947,-89.7606347743909,
-89.676765597129,-89.5928932204471,-89.5090263912954,-89.4251374845022,
-89.3453842196042,-89.2614985497005,-89.1776293724386,-89.0937569957567,
-89.009890166605,-88.9260012598119,-88.8462479949137,-88.7623623250099,
-88.678493147748,-88.5946207710661,-88.5107539419144,-88.4268650351213,
-88.3471117702232,-88.2632261003193,-88.1793569230573,-88.0954845463753,
-88.0116177172235,-87.9277288104303,-87.8479755455326,-87.7640898756289,
-87.680220698367,-87.5963483216851,-87.5124814925333,-87.4285925857402,
-87.3488393208421,-87.2649536509384,-87.1810844736765,-87.0972120969946,
-87.013345267843,-86.9294563610499,-86.8497030961516,-86.7658174262477,
-86.6819482489858,-86.5980758723037,-86.514209043152,-86.4303201363587,
-86.350566871461,-86.2666812015572,-86.1828120242953,-86.0989396476133,
-86.0150728184617,-85.9311839116685,-85.8514306467705,-85.773950742173),
 .UNSPECIFIED.);
#274=B_SPLINE_CURVE_WITH_KNOTS('',3,(#18380,#18381,#18382,#18383,#18384,
#18385,#18386,#18387,#18388,#18389,#18390,#18391,#18392,#18393,#18394,#18395,
#18396,#18397),.UNSPECIFIED.,.F.,.F.,(4,2,1,1,1,1,1,1,1,1,1,1,1,1,4),(82.8002640868724,
82.8127412345886,83.3116131697367,83.8104851048849,84.309357040033,84.8082289751811,
85.3071009103292,85.8059728454774,86.3048447806255,86.8037167157736,87.3025886509217,
87.8014605860699,88.300332521218,88.7992044563661,89.083449394052),
 .UNSPECIFIED.);
#275=B_SPLINE_CURVE_WITH_KNOTS('',3,(#18402,#18403,#18404,#18405,#18406,
#18407,#18408,#18409,#18410,#18411,#18412,#18413,#18414,#18415,#18416,#18417,
#18418,#18419),.UNSPECIFIED.,.F.,.F.,(4,2,1,1,1,1,1,1,1,1,1,1,1,1,4),(-98.3403213565322,
-98.3298362640337,-97.8307000393432,-97.3315638146527,-96.8324275899621,
-96.3332913652716,-95.8341551405811,-95.3350189158905,-94.8358826912,-94.3367464665095,
-93.837610241819,-93.3384740171284,-92.8393377924379,-92.3402015677474,
-92.0571360493526),.UNSPECIFIED.);
#276=B_SPLINE_CURVE_WITH_KNOTS('',3,(#18420,#18421,#18422,#18423,#18424,
#18425,#18426,#18427,#18428,#18429,#18430,#18431,#18432,#18433,#18434,#18435,
#18436),.UNSPECIFIED.,.F.,.F.,(4,1,1,1,1,1,1,1,1,1,1,1,1,1,4),(89.083449394052,
89.2980763915142,89.7969483266623,90.2958202618104,90.7946921969586,91.2935641321067,
91.7924360672548,92.2913080024029,92.7901799375511,93.2890518726992,93.7879238078473,
94.2867957429954,94.7856676781436,95.2845396132917,95.3666347012316),
 .UNSPECIFIED.);
#277=B_SPLINE_CURVE_WITH_KNOTS('',3,(#18441,#18442,#18443,#18444,#18445,
#18446,#18447,#18448,#18449,#18450,#18451,#18452,#18453,#18454,#18455,#18456,
#18457,#18458,#18459,#18460,#18461,#18462,#18463,#18464,#18465,#18466,#18467,
#18468,#18469,#18470,#18471,#18472,#18473,#18474,#18475,#18476,#18477,#18478,
#18479,#18480,#18481,#18482,#18483,#18484,#18485,#18486,#18487,#18488,#18489,
#18490,#18491,#18492,#18493,#18494,#18495,#18496,#18497,#18498,#18499,#18500,
#18501,#18502,#18503,#18504,#18505,#18506,#18507,#18508,#18509,#18510,#18511,
#18512,#18513,#18514,#18515,#18516,#18517,#18518,#18519,#18520,#18521,#18522,
#18523,#18524,#18525,#18526,#18527,#18528,#18529,#18530,#18531,#18532,#18533,
#18534,#18535,#18536,#18537,#18538,#18539,#18540,#18541,#18542,#18543,#18544,
#18545,#18546,#18547,#18548,#18549,#18550,#18551,#18552,#18553,#18554,#18555,
#18556,#18557,#18558,#18559,#18560,#18561,#18562,#18563,#18564,#18565,#18566,
#18567,#18568,#18569,#18570,#18571,#18572,#18573,#18574,#18575,#18576,#18577,
#18578,#18579,#18580,#18581,#18582,#18583,#18584,#18585,#18586,#18587,#18588,
#18589,#18590,#18591,#18592,#18593,#18594,#18595,#18596,#18597,#18598,#18599,
#18600,#18601,#18602,#18603,#18604,#18605,#18606,#18607,#18608,#18609,#18610,
#18611,#18612,#18613,#18614,#18615,#18616,#18617,#18618,#18619,#18620,#18621,
#18622,#18623,#18624,#18625,#18626,#18627,#18628,#18629,#18630,#18631,#18632,
#18633,#18634,#18635,#18636,#18637,#18638,#18639,#18640,#18641,#18642,#18643,
#18644,#18645,#18646,#18647,#18648,#18649,#18650,#18651,#18652,#18653,#18654,
#18655,#18656,#18657,#18658,#18659,#18660,#18661,#18662,#18663,#18664,#18665,
#18666,#18667,#18668,#18669),.UNSPECIFIED.,.F.,.F.,(4,3,3,3,3,3,3,3,3,3,
3,3,3,3,3,3,3,3,3,3,3,3,3,3,3,3,3,3,3,3,3,3,3,3,3,3,3,3,3,3,3,3,3,3,3,3,
3,3,3,3,3,3,3,3,3,3,3,3,3,3,3,3,3,3,3,3,3,3,3,3,3,3,3,3,3,3,4),(-104.623506663712,
-104.539365643134,-104.455225239483,-104.371063224086,-104.31947096032,
-104.235585290418,-104.151716113158,-104.067843736478,-103.983976907328,
-103.900088000536,-103.82033473563,-103.736449065725,-103.652579888463,
-103.56870751178,-103.484840682628,-103.400951775834,-103.321198510939,
-103.237312841034,-103.153443663771,-103.069571287088,-102.985704457936,
-102.901815551142,-102.822062286248,-102.738176616346,-102.654307439086,
-102.570435062405,-102.486568233255,-102.402679326464,-102.322926061558,
-102.239040391653,-102.15517121439,-102.071298837707,-101.987432008554,
-101.903543101759,-101.823789836867,-101.739904166964,-101.656034989703,
-101.572162613023,-101.488295783872,-101.40440687708,-101.324653612177,
-101.240767942272,-101.156898765009,-101.073026388326,-100.989159559174,
-100.90527065238,-100.825517387486,-100.741631717583,-100.657762540321,
-100.57389016364,-100.490023334489,-100.406134427696,-100.326381162796,
-100.242495492892,-100.15862631563,-100.074753938948,-99.9908871097962,
-99.9069982030031,-99.8272449381053,-99.7433592682012,-99.6594900909393,
-99.575617714257,-99.4917508851051,-99.4078619783115,-99.3281087134148,
-99.2442230435111,-99.1603538662499,-99.0764814895682,-98.9926146604168,
-98.9087257536239,-98.8289724887242,-98.7451668881793,-98.6613780460848,
-98.5775865485867,-98.4938001160868,-98.4099924549528,-98.3403213565322),
 .UNSPECIFIED.);
#278=B_SPLINE_CURVE_WITH_KNOTS('',3,(#18670,#18671,#18672,#18673,#18674,
#18675,#18676,#18677,#18678,#18679,#18680,#18681,#18682,#18683,#18684,#18685),
 .UNSPECIFIED.,.F.,.F.,(4,1,1,1,1,1,1,1,1,1,1,1,1,4),(95.3666347012316,
95.7834115484398,96.2822834835879,96.781155418736,97.2800273538842,97.7788992890323,
98.2777712241804,98.7766431593285,99.2755150944767,99.7743870296248,100.273258964773,
100.772130899921,101.271002835069,101.649820008411),.UNSPECIFIED.);
#279=B_SPLINE_CURVE_WITH_KNOTS('',3,(#18690,#18691,#18692,#18693,#18694,
#18695,#18696,#18697,#18698,#18699,#18700,#18701,#18702,#18703,#18704,#18705,
#18706),.UNSPECIFIED.,.F.,.F.,(4,1,1,1,1,1,1,1,1,1,1,1,1,1,4),(-110.906691970891,
-110.808241881297,-110.309105656606,-109.809969431916,-109.310833207225,
-108.811696982535,-108.312560757844,-107.813424533154,-107.314288308463,
-106.815152083773,-106.316015859082,-105.816879634392,-105.317743409701,
-104.818607185011,-104.623506698272),.UNSPECIFIED.);
#280=B_SPLINE_CURVE_WITH_KNOTS('',3,(#18707,#18708,#18709,#18710,#18711,
#18712,#18713,#18714,#18715,#18716,#18717,#18718,#18719,#18720,#18721,#18722,
#18723,#18724,#18725,#18726,#18727,#18728,#18729,#18730,#18731,#18732,#18733,
#18734,#18735,#18736,#18737,#18738,#18739,#18740,#18741,#18742,#18743,#18744,
#18745,#18746,#18747,#18748,#18749,#18750,#18751,#18752,#18753,#18754,#18755,
#18756,#18757,#18758,#18759,#18760,#18761,#18762,#18763,#18764,#18765,#18766,
#18767,#18768,#18769,#18770,#18771,#18772,#18773,#18774,#18775,#18776,#18777,
#18778,#18779,#18780,#18781,#18782,#18783,#18784,#18785,#18786,#18787,#18788,
#18789,#18790,#18791,#18792,#18793,#18794,#18795,#18796,#18797,#18798,#18799,
#18800,#18801,#18802,#18803,#18804,#18805,#18806,#18807,#18808,#18809,#18810,
#18811,#18812,#18813,#18814,#18815,#18816,#18817,#18818,#18819,#18820,#18821,
#18822,#18823,#18824,#18825,#18826,#18827,#18828,#18829,#18830,#18831,#18832,
#18833,#18834,#18835,#18836,#18837,#18838,#18839,#18840,#18841,#18842,#18843,
#18844,#18845,#18846,#18847,#18848,#18849,#18850,#18851,#18852,#18853,#18854,
#18855,#18856,#18857,#18858,#18859,#18860,#18861,#18862,#18863,#18864,#18865,
#18866,#18867,#18868,#18869,#18870,#18871,#18872,#18873,#18874,#18875,#18876,
#18877,#18878,#18879,#18880,#18881,#18882,#18883,#18884,#18885,#18886,#18887,
#18888,#18889,#18890,#18891,#18892,#18893,#18894,#18895,#18896,#18897,#18898,
#18899,#18900,#18901,#18902,#18903,#18904,#18905,#18906,#18907,#18908,#18909,
#18910,#18911,#18912,#18913,#18914,#18915,#18916,#18917,#18918,#18919,#18920,
#18921,#18922,#18923,#18924,#18925,#18926,#18927,#18928,#18929,#18930,#18931,
#18932,#18933,#18934,#18935),.UNSPECIFIED.,.F.,.F.,(4,3,3,3,3,3,3,3,3,3,
3,3,3,3,3,3,3,3,3,3,3,3,3,3,3,3,3,3,3,3,3,3,3,3,3,3,3,3,3,3,3,3,3,3,3,3,
3,3,3,3,3,3,3,3,3,3,3,3,3,3,3,3,3,3,3,3,3,3,3,3,3,3,3,3,3,3,4),(101.649820008525,
101.738164112558,101.769874770217,101.853761879489,101.937632518989,102.021506356458,
102.105374658302,102.189264982259,102.268746705365,102.352633814637,102.436504454139,
102.520378291608,102.604246593453,102.688136917411,102.767618640514,102.851505749785,
102.935376389285,103.019250226753,103.103118528596,103.187008852553,103.266490575662,
103.350377684933,103.434248324432,103.5181221619,103.601990463744,103.6858807877,
103.76536251081,103.849249620082,103.933120259582,104.016994097051,104.100862398895,
104.184752722852,104.264234445958,104.348121555229,104.431992194729,104.515866032197,
104.599734334041,104.683624657998,104.763106381106,104.846993490377,104.930864129877,
105.014737967346,105.09860626919,105.182496593147,105.261978316254,105.345865425525,
105.429736065025,105.513609902494,105.597478204337,105.681368528294,105.760850251402,
105.844737360673,105.928608000172,106.01248183764,106.096350139483,106.180240463439,
106.25972218655,106.343609295823,106.427479935324,106.511353772795,106.59522207464,
106.679112398598,106.758594121699,106.84248123097,106.926351870469,107.010225707938,
107.094094009781,107.177984333737,107.257466056847,107.341353166118,107.425223805617,
107.509097643085,107.592965944928,107.676856268884,107.756337991995,107.844671651442,
107.933005310889),.UNSPECIFIED.);
#281=B_SPLINE_CURVE_WITH_KNOTS('',3,(#18940,#18941,#18942,#18943,#18944,
#18945,#18946,#18947,#18948,#18949,#18950,#18951,#18952,#18953,#18954,#18955,
#18956,#18957,#18958,#18959,#18960,#18961,#18962,#18963,#18964,#18965,#18966,
#18967,#18968,#18969,#18970,#18971,#18972,#18973,#18974,#18975,#18976,#18977,
#18978,#18979,#18980,#18981,#18982,#18983,#18984,#18985,#18986,#18987,#18988,
#18989,#18990,#18991,#18992,#18993,#18994,#18995,#18996,#18997,#18998,#18999,
#19000,#19001,#19002,#19003,#19004,#19005,#19006,#19007,#19008,#19009,#19010,
#19011,#19012,#19013,#19014,#19015,#19016,#19017,#19018,#19019,#19020,#19021,
#19022,#19023,#19024,#19025,#19026,#19027,#19028,#19029,#19030,#19031,#19032,
#19033,#19034,#19035,#19036,#19037,#19038,#19039,#19040,#19041,#19042,#19043,
#19044,#19045,#19046,#19047,#19048,#19049,#19050,#19051,#19052,#19053,#19054,
#19055,#19056,#19057,#19058,#19059,#19060,#19061,#19062,#19063,#19064,#19065,
#19066,#19067,#19068,#19069,#19070,#19071,#19072,#19073,#19074,#19075,#19076,
#19077,#19078,#19079,#19080,#19081,#19082,#19083,#19084,#19085,#19086,#19087,
#19088,#19089,#19090,#19091,#19092,#19093,#19094,#19095,#19096,#19097,#19098,
#19099,#19100,#19101,#19102,#19103,#19104,#19105,#19106,#19107,#19108,#19109,
#19110,#19111,#19112,#19113,#19114,#19115,#19116,#19117,#19118,#19119,#19120,
#19121,#19122,#19123,#19124,#19125,#19126,#19127,#19128,#19129,#19130,#19131,
#19132,#19133,#19134,#19135,#19136,#19137,#19138,#19139,#19140,#19141,#19142,
#19143,#19144,#19145,#19146,#19147,#19148,#19149,#19150,#19151,#19152,#19153,
#19154,#19155,#19156,#19157,#19158,#19159,#19160,#19161,#19162,#19163,#19164,
#19165,#19166,#19167,#19168),.UNSPECIFIED.,.F.,.F.,(4,3,3,3,3,3,3,3,3,3,
3,3,3,3,3,3,3,3,3,3,3,3,3,3,3,3,3,3,3,3,3,3,3,3,3,3,3,3,3,3,3,3,3,3,3,3,
3,3,3,3,3,3,3,3,3,3,3,3,3,3,3,3,3,3,3,3,3,3,3,3,3,3,3,3,3,3,4),(-117.189877278071,
-117.106318081834,-117.022757825786,-116.939202312273,-116.855625995822,
-116.797876577583,-116.713990907681,-116.63012173042,-116.54624935374,-116.46238252459,
-116.378493617798,-116.298740352893,-116.214854682988,-116.130985505724,
-116.047113129041,-115.963246299888,-115.879357393093,-115.799604128202,
-115.715718458299,-115.631849281039,-115.547976904358,-115.464110075207,
-115.380221168415,-115.300467903512,-115.216582233607,-115.132713056344,
-115.048840679661,-114.964973850509,-114.881084943714,-114.801331678821,
-114.717446008918,-114.633576831657,-114.549704454976,-114.465837625825,
-114.381948719033,-114.302195454131,-114.218309784227,-114.134440606965,
-114.050568230283,-113.966701401131,-113.882812494337,-113.80305922944,
-113.719173559535,-113.635304382272,-113.551432005589,-113.467565176436,
-113.383676269642,-113.303923004749,-113.220037334847,-113.136168157587,
-113.052295780907,-112.968428951757,-112.884540044965,-112.804786780059,
-112.720901110154,-112.63703193289,-112.553159556207,-112.469292727054,
-112.385403820259,-112.305650555368,-112.221764885466,-112.137895708205,
-112.054023331524,-111.970156502374,-111.886267595581,-111.806514330678,
-111.722628660774,-111.638759483511,-111.554887106828,-111.471020277677,
-111.387131370883,-111.307378105987,-111.223819822338,-111.140271399509,
-111.056734262025,-110.973184693901,-110.906691970891),.UNSPECIFIED.);
#282=B_SPLINE_CURVE_WITH_KNOTS('',3,(#19169,#19170,#19171,#19172,#19173,
#19174,#19175,#19176,#19177,#19178,#19179,#19180,#19181,#19182,#19183,#19184),
 .UNSPECIFIED.,.F.,.F.,(4,1,1,1,1,1,1,1,1,1,1,1,1,4),(107.933005315591,
108.255209927143,108.754081862291,109.252953797439,109.751825732587,110.250697667735,
110.749569602884,111.248441538032,111.74731347318,112.246185408328,112.745057343476,
113.243929278624,113.742801213772,114.21619062277),.UNSPECIFIED.);
#283=B_SPLINE_CURVE_WITH_KNOTS('',3,(#19189,#19190,#19191,#19192,#19193,
#19194,#19195,#19196,#19197,#19198,#19199,#19200,#19201,#19202,#19203,#19204,
#19205),.UNSPECIFIED.,.F.,.F.,(4,1,1,1,1,1,1,1,1,1,1,1,1,1,4),(-123.473062548923,
-123.28664749856,-122.78751127387,-122.288375049179,-121.789238824488,-121.290102599798,
-120.790966375107,-120.291830150417,-119.792693925726,-119.293557701036,
-118.794421476345,-118.295285251655,-117.796149026964,-117.297012802274,
-117.189877278071),.UNSPECIFIED.);
#284=B_SPLINE_CURVE_WITH_KNOTS('',3,(#19206,#19207,#19208,#19209,#19210,
#19211,#19212,#19213,#19214,#19215,#19216,#19217,#19218,#19219,#19220,#19221,
#19222),.UNSPECIFIED.,.F.,.F.,(4,1,1,1,1,1,1,1,1,1,1,1,1,1,4),(114.21619062277,
114.24167314892,114.740545084069,115.239417019217,115.738288954365,116.237160889513,
116.736032824661,117.234904759809,117.733776694957,118.232648630105,118.731520565254,
119.230392500402,119.72926443555,120.228136370698,120.49937592995),
 .UNSPECIFIED.);
#285=B_SPLINE_CURVE_WITH_KNOTS('',3,(#19227,#19228,#19229,#19230,#19231,
#19232,#19233,#19234,#19235,#19236,#19237,#19238,#19239,#19240,#19241,#19242,
#19243,#19244,#19245,#19246,#19247,#19248,#19249,#19250,#19251,#19252,#19253,
#19254,#19255,#19256,#19257,#19258,#19259,#19260,#19261,#19262,#19263,#19264,
#19265,#19266,#19267,#19268,#19269,#19270,#19271,#19272,#19273,#19274,#19275,
#19276,#19277,#19278,#19279,#19280,#19281,#19282,#19283,#19284,#19285,#19286,
#19287,#19288,#19289,#19290,#19291,#19292,#19293,#19294,#19295,#19296,#19297,
#19298,#19299,#19300,#19301,#19302,#19303,#19304,#19305,#19306,#19307,#19308,
#19309,#19310,#19311,#19312,#19313,#19314,#19315,#19316,#19317,#19318,#19319,
#19320,#19321,#19322,#19323,#19324,#19325,#19326,#19327,#19328,#19329,#19330,
#19331,#19332,#19333,#19334,#19335,#19336,#19337,#19338,#19339,#19340,#19341,
#19342,#19343,#19344,#19345,#19346,#19347,#19348,#19349,#19350,#19351,#19352,
#19353,#19354,#19355,#19356,#19357,#19358,#19359,#19360,#19361,#19362,#19363,
#19364,#19365,#19366,#19367,#19368,#19369,#19370,#19371,#19372,#19373,#19374,
#19375,#19376,#19377,#19378,#19379,#19380,#19381,#19382,#19383,#19384,#19385,
#19386,#19387,#19388,#19389,#19390,#19391,#19392,#19393,#19394,#19395,#19396,
#19397,#19398,#19399,#19400,#19401,#19402,#19403,#19404,#19405,#19406,#19407,
#19408,#19409,#19410,#19411,#19412,#19413,#19414,#19415,#19416,#19417,#19418,
#19419,#19420,#19421,#19422,#19423,#19424,#19425,#19426,#19427,#19428,#19429,
#19430,#19431,#19432,#19433,#19434,#19435,#19436,#19437,#19438,#19439,#19440,
#19441,#19442,#19443,#19444,#19445,#19446,#19447,#19448,#19449,#19450,#19451,
#19452,#19453,#19454,#19455),.UNSPECIFIED.,.F.,.F.,(4,3,3,3,3,3,3,3,3,3,
3,3,3,3,3,3,3,3,3,3,3,3,3,3,3,3,3,3,3,3,3,3,3,3,3,3,3,3,3,3,3,3,3,3,3,3,
3,3,3,3,3,3,3,3,3,3,3,3,3,3,3,3,3,3,3,3,3,3,3,3,3,3,3,3,3,3,4),(-129.756247892334,
-129.672501065347,-129.588770880719,-129.505038060992,-129.421309691022,
-129.337560521526,-129.276282194846,-129.192396524943,-129.108527347683,
-129.024654971003,-128.940788141852,-128.85689923506,-128.777145970156,
-128.693260300251,-128.609391122988,-128.525518746304,-128.441651917152,
-128.357763010357,-128.278009745465,-128.194124075562,-128.110254898301,
-128.02638252162,-127.942515692469,-127.858626785677,-127.778873520775,
-127.69498785087,-127.611118673607,-127.527246296924,-127.443379467772,
-127.359490560978,-127.279737296084,-127.195851626181,-127.11198244892,
-127.028110072239,-126.944243243089,-126.860354336296,-126.780601071394,
-126.696715401489,-126.612846224226,-126.528973847544,-126.445107018391,
-126.361218111597,-126.281464846703,-126.1975791768,-126.113709999539,-126.029837622858,
-125.945970793707,-125.862081886915,-125.782328622013,-125.698442952108,
-125.614573774845,-125.530701398162,-125.44683456901,-125.362945662216,
-125.283192397322,-125.199306727419,-125.115437550158,-125.031565173477,
-124.947698344326,-124.863809437534,-124.784056172632,-124.700170502727,
-124.616301325465,-124.532428948782,-124.448562119629,-124.364673212835,
-124.284919947941,-124.201034278038,-124.117165100776,-124.033292724094,
-123.949425894943,-123.86553698815,-123.785783723251,-123.70171321643,-123.617661695445,
-123.533614860638,-123.473062585251),.UNSPECIFIED.);
#286=B_SPLINE_CURVE_WITH_KNOTS('',3,(#19456,#19457,#19458,#19459,#19460,
#19461,#19462,#19463,#19464,#19465,#19466,#19467,#19468,#19469,#19470,#19471,
#19472,#19473,#19474,#19475,#19476,#19477,#19478,#19479,#19480,#19481,#19482,
#19483,#19484,#19485,#19486,#19487,#19488,#19489,#19490,#19491,#19492,#19493,
#19494,#19495,#19496,#19497,#19498,#19499,#19500,#19501,#19502,#19503,#19504,
#19505,#19506,#19507,#19508,#19509,#19510,#19511,#19512,#19513,#19514,#19515,
#19516,#19517,#19518,#19519,#19520,#19521,#19522,#19523,#19524,#19525,#19526,
#19527,#19528,#19529,#19530,#19531,#19532,#19533,#19534,#19535,#19536,#19537,
#19538,#19539,#19540,#19541,#19542,#19543,#19544,#19545,#19546,#19547,#19548,
#19549,#19550,#19551,#19552,#19553,#19554,#19555,#19556,#19557,#19558,#19559,
#19560,#19561,#19562,#19563,#19564,#19565,#19566,#19567,#19568,#19569,#19570,
#19571,#19572,#19573,#19574,#19575,#19576,#19577,#19578,#19579,#19580,#19581,
#19582,#19583,#19584,#19585,#19586,#19587,#19588,#19589,#19590,#19591,#19592,
#19593,#19594,#19595,#19596,#19597,#19598,#19599,#19600,#19601,#19602,#19603,
#19604,#19605,#19606,#19607,#19608,#19609,#19610,#19611,#19612,#19613,#19614,
#19615,#19616,#19617,#19618,#19619,#19620,#19621,#19622,#19623,#19624,#19625,
#19626,#19627,#19628,#19629,#19630,#19631,#19632,#19633,#19634,#19635,#19636,
#19637,#19638,#19639,#19640,#19641,#19642,#19643,#19644,#19645,#19646,#19647,
#19648,#19649,#19650,#19651,#19652,#19653,#19654,#19655,#19656,#19657,#19658,
#19659,#19660,#19661,#19662,#19663,#19664,#19665,#19666,#19667,#19668,#19669,
#19670,#19671,#19672,#19673,#19674,#19675,#19676,#19677,#19678,#19679,#19680,
#19681,#19682,#19683,#19684),.UNSPECIFIED.,.F.,.F.,(4,3,3,3,3,3,3,3,3,3,
3,3,3,3,3,3,3,3,3,3,3,3,3,3,3,3,3,3,3,3,3,3,3,3,3,3,3,3,3,3,3,3,3,3,3,3,
3,3,3,3,3,3,3,3,3,3,3,3,3,3,3,3,3,3,3,3,3,3,3,3,3,3,3,3,3,3,4),(120.499375931658,
120.584690836811,120.670034253282,120.727008305846,120.810895415117,120.894766054617,
120.978639892086,121.06250819393,121.146398517887,121.225880240994,121.309767350265,
121.393637989765,121.477511827234,121.561380129077,121.645270453034,121.724752176142,
121.808639285413,121.892509924912,121.97638376238,122.060252064223,122.144142388179,
122.22362411129,122.307511220563,122.391381860064,122.475255697534,122.559123999379,
122.643014323338,122.722496046439,122.80638315571,122.890253795209,122.974127632677,
123.057995934521,123.141886258477,123.221367981587,123.305255090858,123.389125730358,
123.472999567826,123.556867869669,123.640758193626,123.720239916735,123.804127026007,
123.887997665507,123.971871502975,124.05573980482,124.139630128777,124.219111851883,
124.302998961154,124.386869600654,124.470743438122,124.554611739966,124.638502063923,
124.717983787031,124.801870896302,124.885741535802,124.969615373271,125.053483675115,
125.137373999072,125.216855722179,125.30074283145,125.38461347095,125.468487308419,
125.552355610263,125.636245934219,125.715727657327,125.799614766598,125.883485406097,
125.967359243565,126.051227545408,126.135117869364,126.214599592475,126.298486701747,
126.382357341248,126.466231178718,126.550099480562,126.63398980452,126.713471527624,
126.78256123713),.UNSPECIFIED.);
#287=B_SPLINE_CURVE_WITH_KNOTS('',3,(#19689,#19690,#19691,#19692,#19693,
#19694,#19695,#19696,#19697,#19698,#19699,#19700,#19701,#19702,#19703,#19704,
#19705,#19706,#19707,#19708,#19709,#19710,#19711,#19712,#19713,#19714,#19715,
#19716,#19717,#19718,#19719,#19720,#19721,#19722,#19723,#19724,#19725,#19726,
#19727,#19728,#19729,#19730,#19731,#19732,#19733,#19734,#19735,#19736,#19737,
#19738,#19739,#19740,#19741,#19742,#19743,#19744,#19745,#19746,#19747,#19748,
#19749,#19750,#19751,#19752,#19753,#19754,#19755,#19756,#19757,#19758,#19759,
#19760,#19761,#19762,#19763,#19764,#19765,#19766,#19767,#19768,#19769,#19770,
#19771,#19772,#19773,#19774,#19775,#19776,#19777,#19778,#19779,#19780,#19781,
#19782,#19783,#19784,#19785,#19786,#19787,#19788,#19789,#19790,#19791,#19792,
#19793,#19794,#19795,#19796,#19797,#19798,#19799,#19800,#19801,#19802,#19803,
#19804,#19805,#19806,#19807,#19808,#19809,#19810,#19811,#19812,#19813,#19814,
#19815,#19816,#19817,#19818,#19819,#19820,#19821,#19822,#19823,#19824,#19825,
#19826,#19827,#19828,#19829,#19830,#19831,#19832,#19833,#19834,#19835,#19836,
#19837,#19838,#19839,#19840,#19841,#19842,#19843,#19844,#19845,#19846,#19847,
#19848,#19849,#19850,#19851,#19852,#19853,#19854,#19855,#19856,#19857,#19858,
#19859,#19860,#19861,#19862,#19863,#19864,#19865,#19866,#19867,#19868,#19869,
#19870,#19871,#19872,#19873,#19874,#19875,#19876,#19877,#19878,#19879,#19880,
#19881,#19882,#19883,#19884,#19885,#19886,#19887,#19888,#19889,#19890,#19891,
#19892,#19893,#19894,#19895,#19896,#19897,#19898,#19899,#19900,#19901,#19902,
#19903,#19904,#19905,#19906,#19907,#19908,#19909,#19910,#19911,#19912,#19913,
#19914,#19915,#19916,#19917,#19918,#19919,#19920),.UNSPECIFIED.,.F.,.F.,
(4,3,3,3,3,3,3,3,3,3,3,3,3,3,3,3,3,3,3,3,3,3,3,3,3,3,3,3,3,3,3,3,3,3,3,
3,3,3,3,3,3,3,3,3,3,3,3,3,3,3,3,3,3,3,3,3,3,3,3,3,3,3,3,3,3,3,3,3,3,3,3,
3,3,3,3,3,3,4),(-136.03943319961,-135.954916822178,-135.870396318605,-135.785855626795,
-135.765053115823,-135.681167445922,-135.597298268663,-135.513425891983,
-135.429559062834,-135.345670156044,-135.265916891133,-135.182031221228,
-135.098162043964,-135.01428966728,-134.930422838127,-134.846533931332,
-134.766780666442,-134.682894996539,-134.599025819279,-134.515153442598,
-134.431286613447,-134.347397706655,-134.267644441752,-134.183758771847,
-134.099889594585,-134.016017217902,-133.932150388749,-133.848261481955,
-133.768508217061,-133.684622547158,-133.600753369897,-133.516880993216,
-133.433014164065,-133.349125257273,-133.269371992371,-133.185486322466,
-133.101617145203,-133.017744768521,-132.933877939368,-132.849989032574,
-132.77023576768,-132.686350097777,-132.602480920516,-132.518608543835,
-132.434741714684,-132.350852807892,-132.27109954299,-132.187213873086,
-132.103344695825,-132.019472319143,-131.935605489991,-131.851716583198,
-131.771963318299,-131.688077648394,-131.604208471131,-131.520336094447,
-131.436469265294,-131.3525803585,-131.272827093608,-131.188941423706,-131.105072246446,
-131.021199869766,-130.937333040617,-130.853444133825,-130.773690868918,
-130.689805199013,-130.605936021749,-130.522063645066,-130.438196815913,
-130.354307909119,-130.274554644227,-130.190668974324,-130.106799797063,
-130.022927420382,-129.939060591231,-129.855171684438,-129.775418419537,
-129.75624789243),.UNSPECIFIED.);
#288=B_SPLINE_CURVE_WITH_KNOTS('',3,(#19921,#19922,#19923,#19924,#19925,
#19926,#19927,#19928,#19929,#19930,#19931,#19932,#19933,#19934,#19935,#19936),
 .UNSPECIFIED.,.F.,.F.,(4,1,1,1,1,1,1,1,1,1,1,1,1,4),(126.782561270967,
127.212343462772,127.71121539792,128.210087333068,128.708959268216,129.207831203364,
129.706703138512,130.20557507366,130.704447008809,131.203318943957,131.702190879105,
132.201062814253,132.699934749401,133.065746544309),.UNSPECIFIED.);
#289=B_SPLINE_CURVE_WITH_KNOTS('',3,(#19941,#19942,#19943,#19944,#19945,
#19946,#19947,#19948,#19949,#19950,#19951,#19952,#19953,#19954,#19955,#19956,
#19957,#19958,#19959,#19960,#19961,#19962,#19963,#19964,#19965,#19966,#19967,
#19968,#19969,#19970,#19971,#19972,#19973,#19974,#19975,#19976,#19977,#19978,
#19979,#19980,#19981,#19982,#19983,#19984,#19985,#19986,#19987,#19988,#19989,
#19990,#19991,#19992,#19993,#19994,#19995,#19996,#19997,#19998,#19999,#20000,
#20001,#20002,#20003,#20004,#20005,#20006,#20007,#20008,#20009,#20010,#20011,
#20012,#20013,#20014,#20015,#20016,#20017,#20018,#20019,#20020,#20021,#20022,
#20023,#20024,#20025,#20026,#20027,#20028,#20029,#20030,#20031,#20032,#20033,
#20034,#20035,#20036,#20037,#20038,#20039,#20040,#20041,#20042,#20043,#20044,
#20045,#20046,#20047,#20048,#20049,#20050,#20051,#20052,#20053,#20054,#20055,
#20056,#20057,#20058,#20059,#20060,#20061,#20062,#20063,#20064,#20065,#20066,
#20067,#20068,#20069,#20070,#20071,#20072,#20073,#20074,#20075,#20076,#20077,
#20078,#20079,#20080,#20081,#20082,#20083,#20084,#20085,#20086,#20087,#20088,
#20089,#20090,#20091,#20092,#20093,#20094,#20095,#20096,#20097,#20098,#20099,
#20100,#20101,#20102,#20103,#20104,#20105,#20106,#20107,#20108,#20109,#20110,
#20111,#20112,#20113,#20114,#20115,#20116,#20117,#20118,#20119,#20120,#20121,
#20122,#20123,#20124,#20125,#20126,#20127,#20128,#20129,#20130,#20131,#20132,
#20133,#20134,#20135,#20136,#20137,#20138,#20139,#20140,#20141,#20142,#20143,
#20144,#20145,#20146,#20147,#20148,#20149,#20150,#20151,#20152,#20153,#20154,
#20155,#20156,#20157,#20158,#20159,#20160,#20161,#20162,#20163,#20164,#20165,
#20166,#20167,#20168,#20169),.UNSPECIFIED.,.F.,.F.,(4,3,3,3,3,3,3,3,3,3,
3,3,3,3,3,3,3,3,3,3,3,3,3,3,3,3,3,3,3,3,3,3,3,3,3,3,3,3,3,3,3,3,3,3,3,3,
3,3,3,3,3,3,3,3,3,3,3,3,3,3,3,3,3,3,3,3,3,3,3,3,3,3,3,3,3,3,4),(-142.322618506789,
-142.2538240368,-142.169938366889,-142.08606918962,-142.002196812931,-141.918329983772,
-141.834441076971,-141.754687812109,-141.670802142209,-141.586932964951,
-141.503060588272,-141.419193759124,-141.335304852334,-141.255551587419,
-141.171665917514,-141.08779674025,-141.003924363566,-140.920057534413,
-140.836168627618,-140.756415362728,-140.672529692825,-140.588660515564,
-140.504788138883,-140.420921309732,-140.33703240294,-140.257279138038,
-140.173393468133,-140.089524290871,-140.005651914188,-139.921785085036,
-139.837896178242,-139.758142913347,-139.674257243444,-139.590388066183,
-139.506515689502,-139.422648860351,-139.338759953558,-139.259006688657,
-139.175121018752,-139.09125184149,-139.007379464807,-138.923512635655,
-138.839623728861,-138.759870463966,-138.675984794063,-138.592115616802,
-138.508243240121,-138.42437641097,-138.340487504177,-138.260734239276,
-138.176848569371,-138.092979392109,-138.009107015426,-137.925240186274,
-137.84135127948,-137.761598014585,-137.677712344682,-137.593843167421,
-137.50997079074,-137.426103961589,-137.342215054797,-137.262461789895,
-137.17857611999,-137.094706942727,-137.010834566045,-136.926967736892,
-136.843078830098,-136.763325565204,-136.679439895301,-136.595570718039,
-136.511698341357,-136.427831512206,-136.343942605413,-136.264189340514,
-136.178785436816,-136.09340281952,-136.039433199766),.UNSPECIFIED.);
#290=B_SPLINE_CURVE_WITH_KNOTS('',3,(#20170,#20171,#20172,#20173,#20174,
#20175,#20176,#20177,#20178,#20179,#20180,#20181,#20182,#20183,#20184,#20185,
#20186,#20187,#20188,#20189,#20190,#20191,#20192,#20193,#20194,#20195,#20196,
#20197,#20198,#20199,#20200,#20201,#20202,#20203,#20204,#20205,#20206,#20207,
#20208,#20209,#20210,#20211,#20212,#20213,#20214,#20215,#20216,#20217,#20218,
#20219,#20220,#20221,#20222,#20223,#20224,#20225,#20226,#20227,#20228,#20229,
#20230,#20231,#20232,#20233,#20234,#20235,#20236,#20237,#20238,#20239,#20240,
#20241,#20242,#20243,#20244,#20245,#20246,#20247,#20248,#20249,#20250,#20251,
#20252,#20253,#20254,#20255,#20256,#20257,#20258,#20259,#20260,#20261,#20262,
#20263,#20264,#20265,#20266,#20267,#20268,#20269,#20270,#20271,#20272,#20273,
#20274,#20275,#20276,#20277,#20278,#20279,#20280,#20281,#20282,#20283,#20284,
#20285,#20286,#20287,#20288,#20289,#20290,#20291,#20292,#20293,#20294,#20295,
#20296,#20297,#20298,#20299,#20300,#20301,#20302,#20303,#20304,#20305,#20306,
#20307,#20308,#20309,#20310,#20311,#20312,#20313,#20314,#20315,#20316,#20317,
#20318,#20319,#20320,#20321,#20322,#20323,#20324,#20325,#20326,#20327,#20328,
#20329,#20330,#20331,#20332,#20333,#20334,#20335,#20336,#20337,#20338,#20339,
#20340,#20341,#20342,#20343,#20344,#20345,#20346,#20347,#20348,#20349,#20350,
#20351,#20352,#20353,#20354,#20355,#20356,#20357,#20358,#20359,#20360,#20361,
#20362,#20363,#20364,#20365,#20366,#20367,#20368,#20369,#20370,#20371,#20372,
#20373,#20374,#20375,#20376,#20377,#20378,#20379,#20380,#20381,#20382,#20383,
#20384,#20385,#20386,#20387,#20388,#20389,#20390,#20391,#20392,#20393,#20394,
#20395,#20396,#20397,#20398),.UNSPECIFIED.,.F.,.F.,(4,3,3,3,3,3,3,3,3,3,
3,3,3,3,3,3,3,3,3,3,3,3,3,3,3,3,3,3,3,3,3,3,3,3,3,3,3,3,3,3,3,3,3,3,3,3,
3,3,3,3,3,3,3,3,3,3,3,3,3,3,3,3,3,3,3,3,3,3,3,3,3,3,3,3,3,3,4),(133.06574654591,
133.153625358515,133.198806684549,133.28269379382,133.36656443332,133.450438270789,
133.534306572632,133.618196896589,133.697678619697,133.781565728968,133.865436368467,
133.949310205935,134.033178507778,134.117068831734,134.196550554845,134.280437664118,
134.364308303619,134.448182141089,134.532050442935,134.615940766893,134.695422489994,
134.779309599265,134.863180238764,134.947054076232,135.030922378076,135.114812702032,
135.194294425142,135.278181534413,135.362052173913,135.445926011381,135.529794313224,
135.613684637181,135.69316636029,135.777053469562,135.860924109062,135.944797946531,
136.028666248375,136.112556572332,136.192038295438,136.275925404709,136.359796044209,
136.443669881677,136.527538183521,136.611428507478,136.690910230586,136.774797339857,
136.858667979357,136.942541816826,137.02641011867,137.110300442627,137.189782165734,
137.273669275005,137.357539914505,137.441413751974,137.525282053817,137.609172377774,
137.688654100882,137.772541210153,137.856411849652,137.94028568712,138.024153988963,
138.108044312919,138.18752603603,138.271413145303,138.355283784804,138.439157622274,
138.52302592412,138.606916248078,138.686397971179,138.77028508045,138.854155719949,
138.938029557418,139.021897859261,139.105788183218,139.185269906327,139.27217567586,
139.348931851342),.UNSPECIFIED.);
#291=B_SPLINE_CURVE_WITH_KNOTS('',3,(#20403,#20404,#20405,#20406,#20407,
#20408,#20409,#20410,#20411,#20412,#20413,#20414,#20415,#20416,#20417,#20418,
#20419,#20420,#20421,#20422,#20423,#20424,#20425,#20426,#20427,#20428,#20429,
#20430,#20431,#20432,#20433,#20434,#20435,#20436,#20437,#20438,#20439,#20440,
#20441,#20442,#20443,#20444,#20445,#20446,#20447,#20448,#20449,#20450,#20451,
#20452,#20453,#20454,#20455,#20456,#20457,#20458,#20459,#20460,#20461,#20462,
#20463,#20464,#20465,#20466,#20467,#20468,#20469,#20470,#20471,#20472,#20473,
#20474,#20475,#20476,#20477,#20478,#20479,#20480,#20481,#20482,#20483,#20484,
#20485,#20486,#20487,#20488,#20489,#20490,#20491,#20492,#20493,#20494,#20495,
#20496,#20497,#20498,#20499,#20500,#20501,#20502,#20503,#20504,#20505,#20506,
#20507,#20508,#20509,#20510,#20511,#20512,#20513,#20514,#20515,#20516,#20517,
#20518,#20519,#20520,#20521,#20522,#20523,#20524,#20525,#20526,#20527,#20528,
#20529,#20530,#20531,#20532,#20533,#20534,#20535,#20536,#20537,#20538,#20539,
#20540,#20541,#20542,#20543,#20544,#20545,#20546,#20547,#20548,#20549,#20550,
#20551,#20552,#20553,#20554,#20555,#20556,#20557,#20558,#20559,#20560,#20561,
#20562,#20563,#20564,#20565,#20566,#20567,#20568,#20569,#20570,#20571,#20572,
#20573,#20574,#20575,#20576,#20577,#20578,#20579,#20580,#20581,#20582,#20583,
#20584,#20585,#20586,#20587,#20588,#20589,#20590,#20591,#20592,#20593,#20594,
#20595,#20596,#20597,#20598,#20599,#20600,#20601,#20602,#20603,#20604,#20605,
#20606,#20607,#20608,#20609,#20610,#20611,#20612,#20613,#20614,#20615,#20616,
#20617,#20618,#20619,#20620,#20621,#20622,#20623,#20624,#20625,#20626,#20627,
#20628,#20629,#20630,#20631,#20632,#20633,#20634),.UNSPECIFIED.,.F.,.F.,
(4,3,3,3,3,3,3,3,3,3,3,3,3,3,3,3,3,3,3,3,3,3,3,3,3,3,3,3,3,3,3,3,3,3,3,
3,3,3,3,3,3,3,3,3,3,3,3,3,3,3,3,3,3,3,3,3,3,3,3,3,3,3,3,3,3,3,3,3,3,3,3,
3,3,3,3,3,3,4),(-148.605803813969,-148.522140022128,-148.438471933085,-148.354805244716,
-148.271119566466,-148.243458733086,-148.159573063184,-148.075703885924,
-147.991831509244,-147.907964680095,-147.824075773303,-147.744322508396,
-147.660436838491,-147.576567661227,-147.492695284544,-147.408828455391,
-147.324939548596,-147.245186283705,-147.161300613802,-147.077431436542,
-146.993559059861,-146.90969223071,-146.825803323918,-146.746050059015,
-146.66216438911,-146.578295211848,-146.494422835165,-146.410556006012,
-146.326667099218,-146.246913834324,-146.163028164421,-146.079158987161,
-145.99528661048,-145.911419781329,-145.827530874536,-145.747777609634,
-145.663891939729,-145.580022762467,-145.496150385784,-145.412283556631,
-145.328394649837,-145.248641384943,-145.16475571504,-145.080886537779,
-144.997014161098,-144.913147331947,-144.829258425155,-144.749505160253,
-144.665619490348,-144.581750313085,-144.497877936402,-144.41401110725,
-144.330122200456,-144.250368935562,-144.166483265659,-144.082614088398,
-143.998741711717,-143.914874882566,-143.830985975773,-143.751232710872,
-143.667347040967,-143.583477863704,-143.499605487021,-143.415738657868,
-143.331849751074,-143.252096486181,-143.168210816278,-143.084341639018,
-143.000469262337,-142.916602433186,-142.832713526393,-142.752960261491,
-142.669402437547,-142.582706454893,-142.499167632398,-142.415631931664,
-142.332082149227,-142.322618506932),.UNSPECIFIED.);
#292=B_SPLINE_CURVE_WITH_KNOTS('',3,(#20635,#20636,#20637,#20638,#20639,
#20640,#20641,#20642,#20643,#20644,#20645,#20646,#20647,#20648,#20649,#20650,
#20651,#20652,#20653,#20654,#20655,#20656,#20657,#20658,#20659,#20660,#20661,
#20662,#20663,#20664,#20665,#20666,#20667,#20668,#20669,#20670,#20671,#20672,
#20673,#20674,#20675,#20676,#20677,#20678,#20679,#20680,#20681,#20682,#20683,
#20684,#20685,#20686,#20687,#20688,#20689,#20690,#20691,#20692,#20693,#20694,
#20695,#20696,#20697,#20698,#20699,#20700,#20701,#20702,#20703,#20704,#20705,
#20706,#20707,#20708,#20709,#20710,#20711,#20712,#20713,#20714,#20715,#20716,
#20717,#20718,#20719,#20720,#20721,#20722,#20723,#20724,#20725,#20726,#20727,
#20728,#20729,#20730,#20731,#20732,#20733,#20734,#20735,#20736,#20737,#20738,
#20739,#20740,#20741,#20742,#20743,#20744,#20745,#20746,#20747,#20748,#20749,
#20750,#20751,#20752,#20753,#20754,#20755,#20756,#20757,#20758,#20759,#20760,
#20761,#20762,#20763,#20764,#20765,#20766,#20767,#20768,#20769,#20770,#20771,
#20772,#20773,#20774,#20775,#20776,#20777,#20778,#20779,#20780,#20781,#20782,
#20783,#20784,#20785,#20786,#20787,#20788,#20789,#20790,#20791,#20792,#20793,
#20794,#20795,#20796,#20797,#20798,#20799,#20800,#20801,#20802,#20803,#20804,
#20805,#20806,#20807,#20808,#20809,#20810,#20811,#20812,#20813,#20814,#20815,
#20816,#20817,#20818,#20819,#20820,#20821,#20822,#20823,#20824,#20825,#20826,
#20827,#20828,#20829,#20830,#20831,#20832,#20833,#20834,#20835,#20836,#20837,
#20838,#20839,#20840,#20841,#20842,#20843,#20844,#20845,#20846,#20847,#20848,
#20849,#20850,#20851,#20852,#20853,#20854,#20855,#20856,#20857,#20858,#20859,
#20860,#20861,#20862,#20863),.UNSPECIFIED.,.F.,.F.,(4,3,3,3,3,3,3,3,3,3,
3,3,3,3,3,3,3,3,3,3,3,3,3,3,3,3,3,3,3,3,3,3,3,3,3,3,3,3,3,3,3,3,3,3,3,3,
3,3,3,3,3,3,3,3,3,3,3,3,3,3,3,3,3,3,3,3,3,3,3,3,3,3,3,3,3,3,4),(139.348931851489,
139.432781290692,139.516625387566,139.600492989817,139.684141841475,139.768028950746,
139.851899590246,139.935773427714,140.019641729558,140.103532053515,140.183013776623,
140.266900885895,140.350771525394,140.434645362863,140.518513664707,140.602403988664,
140.681885711771,140.765772821042,140.849643460542,140.93351729801,141.017385599854,
141.101275923811,141.180757646919,141.26464475619,141.34851539569,141.432389233158,
141.516257535002,141.600147858959,141.679629582067,141.763516691338,141.847387330838,
141.931261168306,142.01512947015,142.099019794107,142.178501517215,142.262388626485,
142.346259265984,142.430133103452,142.514001405295,142.597891729251,142.677373452363,
142.761260561636,142.845131201137,142.929005038607,143.012873340453,143.096763664411,
143.176245387512,143.260132496783,143.344003136282,143.42787697375,143.511745275594,
143.59563559955,143.67511732266,143.759004431931,143.84287507143,143.926748908899,
144.010617210742,144.094507534699,144.173989257808,144.257876367079,144.341747006579,
144.425620844049,144.509489145893,144.59337946985,144.672861192956,144.756748302227,
144.840618941727,144.924492779196,145.00836108104,145.092251404997,145.171733128104,
145.255379913839,145.33900944156,145.422639950478,145.506266407228,145.589910997829,
145.632117158518),.UNSPECIFIED.);
#293=B_SPLINE_CURVE_WITH_KNOTS('',3,(#20868,#20869,#20870,#20871,#20872,
#20873,#20874,#20875,#20876,#20877,#20878,#20879,#20880,#20881,#20882,#20883,
#20884),.UNSPECIFIED.,.F.,.F.,(4,1,1,1,1,1,1,1,1,1,1,1,1,1,4),(-154.888989121148,
-154.732229654063,-154.233093429373,-153.733957204682,-153.234820979992,
-152.735684755301,-152.236548530611,-151.73741230592,-151.238276081229,
-150.739139856539,-150.240003631848,-149.740867407158,-149.241731182467,
-148.742594957777,-148.605803832893),.UNSPECIFIED.);
#294=B_SPLINE_CURVE_WITH_KNOTS('',3,(#20885,#20886,#20887,#20888,#20889,
#20890,#20891,#20892,#20893,#20894,#20895,#20896,#20897,#20898,#20899,#20900,
#20901,#20902,#20903,#20904,#20905,#20906,#20907,#20908,#20909,#20910,#20911,
#20912,#20913,#20914,#20915,#20916,#20917,#20918,#20919,#20920,#20921,#20922,
#20923,#20924,#20925,#20926,#20927,#20928,#20929,#20930,#20931,#20932,#20933,
#20934,#20935,#20936,#20937,#20938,#20939,#20940,#20941,#20942,#20943,#20944,
#20945,#20946,#20947,#20948,#20949,#20950,#20951,#20952,#20953,#20954,#20955,
#20956,#20957,#20958,#20959,#20960,#20961,#20962,#20963,#20964,#20965,#20966,
#20967,#20968,#20969,#20970,#20971,#20972,#20973,#20974,#20975,#20976,#20977,
#20978,#20979,#20980,#20981,#20982,#20983,#20984,#20985,#20986,#20987,#20988,
#20989,#20990,#20991,#20992,#20993,#20994,#20995,#20996,#20997,#20998,#20999,
#21000,#21001,#21002,#21003,#21004,#21005,#21006,#21007,#21008,#21009,#21010,
#21011,#21012,#21013,#21014,#21015,#21016,#21017,#21018,#21019,#21020,#21021,
#21022,#21023,#21024,#21025,#21026,#21027,#21028,#21029,#21030,#21031,#21032,
#21033,#21034,#21035,#21036,#21037,#21038,#21039,#21040,#21041,#21042,#21043,
#21044,#21045,#21046,#21047,#21048,#21049,#21050,#21051,#21052,#21053,#21054,
#21055,#21056,#21057,#21058,#21059,#21060,#21061,#21062,#21063,#21064,#21065,
#21066,#21067,#21068,#21069,#21070,#21071,#21072,#21073,#21074,#21075,#21076,
#21077,#21078,#21079,#21080,#21081,#21082,#21083,#21084,#21085,#21086,#21087,
#21088,#21089,#21090,#21091,#21092,#21093,#21094,#21095,#21096,#21097,#21098,
#21099,#21100,#21101,#21102,#21103,#21104,#21105,#21106,#21107,#21108,#21109,
#21110,#21111,#21112,#21113),.UNSPECIFIED.,.F.,.F.,(4,3,3,3,3,3,3,3,3,3,
3,3,3,3,3,3,3,3,3,3,3,3,3,3,3,3,3,3,3,3,3,3,3,3,3,3,3,3,3,3,3,3,3,3,3,3,
3,3,3,3,3,3,3,3,3,3,3,3,3,3,3,3,3,3,3,3,3,3,3,3,3,3,3,3,3,3,4),(145.632117158668,
145.670605063252,145.754492172522,145.83836281202,145.922236649487,146.006104951329,
146.089995275284,146.1694769984,146.253364107671,146.337234747171,146.421108584639,
146.504976886483,146.58886721044,146.668348933548,146.752236042821,146.836106682322,
146.919980519792,147.003848821637,147.087739145595,147.167220868697,147.251107977968,
147.334978617467,147.418852454935,147.502720756779,147.586611080735,147.666092803845,
147.749979913116,147.833850552616,147.917724390084,148.001592691927,148.085483015884,
148.164964738993,148.248851848265,148.332722487765,148.416596325233,148.500464627077,
148.584354951034,148.663836674141,148.747723783412,148.831594422912,148.91546826038,
148.999336562224,149.083226886181,149.162708609289,149.24659571856,149.33046635806,
149.414340195529,149.498208497373,149.58209882133,149.661580544437,149.745467653708,
149.829338293208,149.913212130677,149.99708043252,150.080970756477,150.160452479585,
150.244339588856,150.328210228355,150.412084065823,150.495952367666,150.579842691622,
150.659324414733,150.743211524006,150.827082163507,150.910956000977,150.994824302823,
151.078714626781,151.158196349882,151.242083459153,151.325954098653,151.409827936121,
151.493696237965,151.577586561921,151.65706828503,151.741856065642,151.828579265745,
151.915302465848),.UNSPECIFIED.);
#295=B_SPLINE_CURVE_WITH_KNOTS('',3,(#21118,#21119,#21120,#21121,#21122,
#21123,#21124,#21125,#21126,#21127,#21128,#21129,#21130,#21131,#21132,#21133),
 .UNSPECIFIED.,.F.,.F.,(4,1,1,1,1,1,1,1,1,1,1,1,1,4),(-161.172174428328,
-160.72186435035,-160.222728125659,-159.723591900968,-159.224455676278,
-158.725319451587,-158.226183226897,-157.727047002206,-157.227910777516,
-156.728774552825,-156.229638328135,-155.730502103444,-155.231365878754,
-154.888989121148),.UNSPECIFIED.);
#296=B_SPLINE_CURVE_WITH_KNOTS('',3,(#21134,#21135,#21136,#21137,#21138,
#21139,#21140,#21141,#21142,#21143,#21144,#21145,#21146,#21147,#21148,#21149,
#21150),.UNSPECIFIED.,.F.,.F.,(4,1,1,1,1,1,1,1,1,1,1,1,1,1,4),(151.915302472681,
152.155940220178,152.654812155326,153.153684090474,153.652556025622,154.15142796077,
154.650299895918,155.149171831067,155.648043766215,156.146915701363,156.645787636511,
157.144659571659,157.643531506807,158.142403441955,158.198487773027),
 .UNSPECIFIED.);
#297=B_SPLINE_CURVE_WITH_KNOTS('',3,(#21155,#21156,#21157,#21158,#21159,
#21160,#21161,#21162,#21163,#21164,#21165,#21166,#21167,#21168,#21169,#21170,
#21171),.UNSPECIFIED.,.F.,.F.,(4,1,1,1,1,1,1,1,1,1,1,1,1,1,4),(-167.455359731888,
-167.210635271326,-166.711499046636,-166.212362821945,-165.713226597255,
-165.214090372564,-164.714954147874,-164.215817923183,-163.716681698493,
-163.217545473802,-162.718409249112,-162.219273024421,-161.720136799731,
-161.22100057504,-161.172174428328),.UNSPECIFIED.);
#298=B_SPLINE_CURVE_WITH_KNOTS('',3,(#21172,#21173,#21174,#21175,#21176,
#21177,#21178,#21179,#21180,#21181,#21182,#21183,#21184,#21185,#21186,#21187,
#21188,#21189,#21190,#21191,#21192,#21193,#21194,#21195,#21196,#21197,#21198,
#21199,#21200,#21201,#21202,#21203,#21204,#21205,#21206,#21207,#21208,#21209,
#21210,#21211,#21212,#21213,#21214,#21215,#21216,#21217,#21218,#21219,#21220,
#21221,#21222,#21223,#21224,#21225,#21226,#21227,#21228,#21229,#21230,#21231,
#21232,#21233,#21234,#21235,#21236,#21237,#21238,#21239,#21240,#21241,#21242,
#21243,#21244,#21245,#21246,#21247,#21248,#21249,#21250,#21251,#21252,#21253,
#21254,#21255,#21256,#21257,#21258,#21259,#21260,#21261,#21262,#21263,#21264,
#21265,#21266,#21267,#21268,#21269,#21270,#21271,#21272,#21273,#21274,#21275,
#21276,#21277,#21278,#21279,#21280,#21281,#21282,#21283,#21284,#21285,#21286,
#21287,#21288,#21289,#21290,#21291,#21292,#21293,#21294,#21295,#21296,#21297,
#21298,#21299,#21300,#21301,#21302,#21303,#21304,#21305,#21306,#21307,#21308,
#21309,#21310,#21311,#21312,#21313,#21314,#21315,#21316,#21317,#21318,#21319,
#21320,#21321,#21322,#21323,#21324,#21325,#21326,#21327,#21328,#21329,#21330,
#21331,#21332,#21333,#21334,#21335,#21336,#21337,#21338,#21339,#21340,#21341,
#21342,#21343,#21344,#21345,#21346,#21347,#21348,#21349,#21350,#21351,#21352,
#21353,#21354,#21355,#21356,#21357,#21358,#21359,#21360,#21361,#21362,#21363,
#21364,#21365,#21366,#21367,#21368,#21369,#21370,#21371,#21372,#21373,#21374,
#21375,#21376,#21377,#21378,#21379,#21380,#21381,#21382,#21383,#21384,#21385,
#21386,#21387,#21388,#21389,#21390,#21391,#21392,#21393,#21394,#21395,#21396,
#21397,#21398,#21399,#21400,#21401,#21402,#21403),.UNSPECIFIED.,.F.,.F.,
(4,3,3,3,3,3,3,3,3,3,3,3,3,3,3,3,3,3,3,3,3,3,3,3,3,3,3,3,3,3,3,3,3,3,3,
3,3,3,3,3,3,3,3,3,3,3,3,3,3,3,3,3,3,3,3,3,3,3,3,3,3,3,3,3,3,3,3,3,3,3,3,
3,3,3,3,3,3,4),(158.198487773027,158.282067716573,158.365632542258,158.449200633782,
158.53276711861,158.616352361724,158.641275377103,158.725162486376,158.809033125877,
158.892906963347,158.976775265193,159.060665589151,159.140147312252,159.224034421523,
159.307905061022,159.391778898491,159.475647200334,159.55953752429,159.6390192474,
159.722906356671,159.80677699617,159.890650833639,159.974519135482,160.058409459439,
160.137891182548,160.221778291819,160.305648931319,160.389522768788,160.473391070632,
160.557281394589,160.636763117696,160.720650226967,160.804520866467,160.888394703936,
160.97226300578,161.056153329736,161.135635052844,161.219522162115,161.303392801615,
161.387266639084,161.471134940928,161.555025264885,161.634506987992,161.718394097263,
161.802264736764,161.886138574232,161.970006876076,162.053897200033,162.13337892314,
162.21726603241,162.301136671909,162.385010509377,162.46887881122,162.552769135176,
162.632250858288,162.716137967561,162.800008607062,162.883882444532,162.967750746378,
163.051641070336,163.131122793437,163.215009902708,163.298880542208,163.382754379676,
163.466622681519,163.550513005476,163.629994728585,163.713881837856,163.797752477355,
163.881626314824,163.965494616667,164.049384940624,164.128866663733,164.212606748055,
164.296333176365,164.380048090638,164.463765710071,164.481673080207),
 .UNSPECIFIED.);
#299=B_SPLINE_CURVE_WITH_KNOTS('',3,(#21408,#21409,#21410,#21411,#21412,
#21413,#21414,#21415,#21416,#21417,#21418,#21419,#21420,#21421,#21422,#21423,
#21424,#21425,#21426,#21427,#21428,#21429,#21430,#21431,#21432,#21433,#21434,
#21435,#21436,#21437,#21438,#21439,#21440,#21441,#21442,#21443,#21444,#21445,
#21446,#21447,#21448,#21449,#21450,#21451,#21452,#21453,#21454,#21455,#21456,
#21457,#21458,#21459,#21460,#21461,#21462,#21463,#21464,#21465,#21466,#21467,
#21468,#21469,#21470,#21471,#21472,#21473,#21474,#21475,#21476,#21477,#21478,
#21479,#21480,#21481,#21482,#21483,#21484,#21485,#21486,#21487,#21488,#21489,
#21490,#21491,#21492,#21493,#21494,#21495,#21496,#21497,#21498,#21499,#21500,
#21501,#21502,#21503,#21504,#21505,#21506,#21507,#21508,#21509,#21510,#21511,
#21512,#21513,#21514,#21515,#21516,#21517,#21518,#21519,#21520,#21521,#21522,
#21523,#21524,#21525,#21526,#21527,#21528,#21529,#21530,#21531,#21532,#21533,
#21534,#21535,#21536,#21537,#21538,#21539,#21540,#21541,#21542,#21543,#21544,
#21545,#21546,#21547,#21548,#21549,#21550,#21551,#21552,#21553,#21554,#21555,
#21556,#21557,#21558,#21559,#21560,#21561,#21562,#21563,#21564,#21565,#21566,
#21567,#21568,#21569,#21570,#21571,#21572,#21573,#21574,#21575,#21576,#21577,
#21578,#21579,#21580,#21581,#21582,#21583,#21584,#21585,#21586,#21587,#21588,
#21589,#21590,#21591,#21592,#21593,#21594,#21595,#21596,#21597,#21598,#21599,
#21600,#21601,#21602,#21603,#21604,#21605,#21606,#21607,#21608,#21609,#21610,
#21611,#21612,#21613,#21614,#21615,#21616,#21617,#21618,#21619,#21620,#21621,
#21622,#21623,#21624,#21625,#21626,#21627,#21628,#21629,#21630,#21631,#21632,
#21633,#21634,#21635,#21636),.UNSPECIFIED.,.F.,.F.,(4,3,3,3,3,3,3,3,3,3,
3,3,3,3,3,3,3,3,3,3,3,3,3,3,3,3,3,3,3,3,3,3,3,3,3,3,3,3,3,3,3,3,3,3,3,3,
3,3,3,3,3,3,3,3,3,3,3,3,3,3,3,3,3,3,3,3,3,3,3,3,3,3,3,3,3,3,4),(-173.738545042687,
-173.699406192303,-173.615520474108,-173.531651247652,-173.447778820846,
-173.36391194116,-173.280022983632,-173.200269967613,-173.116384358978,
-173.032515243893,-172.9486429302,-172.864776164356,-172.780887320795,-172.701133742922,
-172.617248030574,-172.533378810287,-172.449506390094,-172.365639517252,
-172.281750566889,-172.201997518232,-172.118111870431,-172.034242715556,
-171.950370361485,-171.866503555021,-171.782614670828,-171.702861293541,
-171.618975614894,-171.535106428785,-171.451234043183,-171.367367205088,
-171.283478289399,-171.203725068851,-171.119839401012,-171.035970225832,
-170.95209785124,-170.868231024179,-170.784342119456,-170.70458884416,-170.620703174694,
-170.536833997881,-170.452961621661,-170.369094792976,-170.285205886656,
-170.20545261947,-170.12156694863,-170.037697770418,-169.953825392773,-169.869958562653,
-169.786069654891,-169.706316394779,-169.622430725601,-169.538561549075,
-169.454689173137,-169.370822344733,-169.286933438686,-169.207180170088,
-169.123294499777,-169.039425322103,-168.955552945005,-168.871686115435,
-168.787797208226,-168.708043945398,-168.62415827567,-168.540289098585,
-168.456416722082,-168.37254989311,-168.288660986495,-168.208907720707,
-168.125022050752,-168.041152873438,-167.957280496704,-167.8734136675,-167.789524760655,
-167.709771496017,-167.624918798546,-167.540081689336,-167.455359735508),
 .UNSPECIFIED.);
#300=B_SPLINE_CURVE_WITH_KNOTS('',3,(#21637,#21638,#21639,#21640,#21641,
#21642,#21643,#21644,#21645,#21646,#21647,#21648,#21649,#21650,#21651,#21652,
#21653,#21654,#21655,#21656,#21657,#21658,#21659,#21660,#21661,#21662,#21663,
#21664,#21665,#21666,#21667,#21668,#21669,#21670,#21671,#21672,#21673,#21674,
#21675,#21676,#21677,#21678,#21679,#21680,#21681,#21682,#21683,#21684,#21685,
#21686,#21687,#21688,#21689,#21690,#21691,#21692,#21693,#21694,#21695,#21696,
#21697,#21698,#21699,#21700,#21701,#21702,#21703,#21704,#21705,#21706,#21707,
#21708,#21709,#21710,#21711,#21712,#21713,#21714,#21715,#21716,#21717,#21718,
#21719,#21720,#21721,#21722,#21723,#21724,#21725,#21726,#21727,#21728,#21729,
#21730,#21731,#21732,#21733,#21734,#21735,#21736,#21737,#21738,#21739,#21740,
#21741,#21742,#21743,#21744,#21745,#21746,#21747,#21748,#21749,#21750,#21751,
#21752,#21753,#21754,#21755,#21756,#21757,#21758,#21759,#21760,#21761,#21762,
#21763,#21764,#21765,#21766,#21767,#21768,#21769,#21770,#21771,#21772,#21773,
#21774,#21775,#21776,#21777,#21778,#21779,#21780,#21781,#21782,#21783,#21784,
#21785,#21786,#21787,#21788,#21789,#21790,#21791,#21792,#21793,#21794,#21795,
#21796,#21797,#21798,#21799,#21800,#21801,#21802,#21803,#21804,#21805,#21806,
#21807,#21808,#21809,#21810,#21811,#21812,#21813,#21814,#21815,#21816,#21817,
#21818,#21819,#21820,#21821,#21822,#21823,#21824,#21825,#21826,#21827,#21828,
#21829,#21830,#21831,#21832,#21833,#21834,#21835,#21836,#21837,#21838,#21839,
#21840,#21841,#21842,#21843,#21844,#21845,#21846,#21847,#21848,#21849,#21850,
#21851,#21852,#21853,#21854,#21855,#21856,#21857,#21858,#21859,#21860,#21861,
#21862,#21863,#21864,#21865),.UNSPECIFIED.,.F.,.F.,(4,3,3,3,3,3,3,3,3,3,
3,3,3,3,3,3,3,3,3,3,3,3,3,3,3,3,3,3,3,3,3,3,3,3,3,3,3,3,3,3,3,3,3,3,3,3,
3,3,3,3,3,3,3,3,3,3,3,3,3,3,3,3,3,3,3,3,3,3,3,3,3,3,3,3,3,3,4),(164.481673080314,
164.569118274427,164.627738598881,164.711625708152,164.795496347652,164.87937018512,
164.963238486964,165.04712881092,165.126610534029,165.2104976433,165.2943682828,
165.378242120268,165.462110422112,165.546000746069,165.625482469177,165.709369578449,
165.793240217948,165.877114055417,165.960982357261,166.044872681218,166.124354404325,
166.208241513596,166.292112153095,166.375985990563,166.459854292407,166.543744616363,
166.623226339473,166.707113448745,166.790984088245,166.874857925714,166.958726227558,
167.042616551515,167.122098274622,167.205985383896,167.289856023399,167.373729860871,
167.457598162718,167.541488486678,167.62097020977,167.704857319034,167.788727958525,
167.872601795986,167.956470097822,168.040360421771,168.119842144918,168.203729254202,
168.287599893714,168.371473731196,168.455342033052,168.539232357021,168.618714080066,
168.702601189323,168.786471828809,168.870345666264,168.954213968094,169.038104292037,
169.117586015214,169.201473124485,169.285343763985,169.369217601454,169.453085903297,
169.536976227254,169.616457950362,169.700345059686,169.784215699238,169.86808953676,
169.951957838656,170.035848162665,170.11532988551,170.199216994602,170.283087633921,
170.36696147121,170.450829772875,170.534720096655,170.614201820658,170.701501165913,
170.764858384118),.UNSPECIFIED.);
#301=B_SPLINE_CURVE_WITH_KNOTS('',3,(#21871,#21872,#21873,#21874,#21875,
#21876,#21877,#21878,#21879,#21880,#21881,#21882,#21883,#21884,#21885,#21886,
#21887,#21888,#21889,#21890,#21891,#21892,#21893,#21894,#21895,#21896,#21897,
#21898,#21899,#21900,#21901,#21902,#21903,#21904,#21905,#21906,#21907,#21908,
#21909,#21910,#21911,#21912,#21913,#21914,#21915,#21916,#21917,#21918,#21919,
#21920,#21921,#21922,#21923,#21924,#21925,#21926,#21927,#21928,#21929,#21930,
#21931,#21932,#21933,#21934,#21935,#21936,#21937,#21938,#21939,#21940,#21941,
#21942,#21943,#21944,#21945,#21946,#21947,#21948,#21949,#21950,#21951,#21952,
#21953,#21954,#21955,#21956,#21957,#21958,#21959,#21960,#21961,#21962,#21963,
#21964,#21965,#21966,#21967,#21968,#21969,#21970,#21971,#21972,#21973,#21974,
#21975,#21976,#21977,#21978,#21979,#21980,#21981,#21982,#21983,#21984,#21985,
#21986,#21987,#21988,#21989,#21990,#21991,#21992,#21993,#21994,#21995,#21996,
#21997,#21998,#21999,#22000,#22001,#22002,#22003,#22004,#22005,#22006,#22007,
#22008,#22009,#22010,#22011,#22012,#22013,#22014,#22015,#22016,#22017,#22018,
#22019,#22020,#22021,#22022,#22023,#22024,#22025,#22026,#22027,#22028,#22029,
#22030,#22031,#22032,#22033,#22034,#22035,#22036,#22037,#22038,#22039,#22040,
#22041,#22042,#22043,#22044,#22045,#22046,#22047,#22048,#22049,#22050,#22051,
#22052,#22053,#22054,#22055,#22056,#22057,#22058,#22059,#22060,#22061,#22062,
#22063,#22064,#22065,#22066,#22067,#22068,#22069,#22070,#22071,#22072,#22073,
#22074,#22075,#22076,#22077,#22078,#22079,#22080,#22081,#22082,#22083,#22084,
#22085,#22086),.UNSPECIFIED.,.F.,.F.,(4,2,2,2,2,2,2,2,2,2,2,2,2,2,2,2,2,
2,2,2,2,2,2,2,2,2,2,2,2,2,2,2,2,2,2,2,2,2,2,2,2,2,2,2,2,2,2,2,2,2,2,2,2,
2,2,2,2,2,2,2,2,2,2,2,2,2,2,2,2,2,2,2,2,2,2,2,2,2,2,2,2,2,2,2,2,2,2,2,2,
2,2,2,2,2,2,2,2,2,2,2,2,2,2,2,2,2,2,4),(-2.50346624102753,-2.43566920503879,
-2.42234310441723,-2.41035223133324,-2.37127141320223,-2.31761164675876,
-2.29859044626815,-2.27703879221759,-2.2248560455562,-2.18904768902528,
-2.17607336568454,-2.1638362674717,-2.1239626082453,-2.08289413542988,-2.05863349320715,
-2.03821977278105,-2.00561269853488,-1.97829323757455,-1.94103356910006,
-1.92891303314842,-1.91578007696407,-1.89955124089702,-1.85806998165083,
-1.82268755444853,-1.80211163604484,-1.77857993497384,-1.75126575489051,
-1.70260310294369,-1.68726144390728,-1.67716363456753,-1.65689027179377,
-1.62317397840196,-1.58021080636604,-1.56120223810918,-1.53963604757273,
-1.52761556617662,-1.4722056871182,-1.44834505614351,-1.43770829427052,
-1.42482247531397,-1.41668210727651,-1.39252640615786,-1.35943129143669,
-1.32853587377931,-1.30821411897408,-1.28328768866377,-1.25290018652973,
-1.2030445926792,-1.1922795136485,-1.17962456865186,-1.16428534746891,-1.12819197914595,
-1.11363628885357,-1.08275460647199,-1.06243842889265,-1.03752117251266,
-1.00714964079731,-0.957239748577986,-0.946483423730389,-0.933818042528201,
-0.918460270652399,-0.882268090172703,-0.842592179484583,-0.823627131129384,
-0.812109376798758,-0.7853416346558,-0.747758021721972,-0.713514886085762,
-0.700886880660439,-0.696882063678745,-0.696137250227313,-0.695202287417338,
-0.694399496298766,-0.69366231154534,-0.692951505311127,-0.692239065910569,
-0.691501346633369,-0.690715330571306,-0.689855991440339,-0.688893893977781,
-0.68779255385779,-0.686505193452603,-0.669950760361063,-0.62627733587133,
-0.592875183501239,-0.576900412250272,-0.556514282642967,-0.533244428834864,
-0.484086277971169,-0.462531063040552,-0.452374125784664,-0.44147482145213,
-0.436499934341845,-0.415921371225028,-0.349296598887226,-0.328915722615678,
-0.325520518491996,-0.3208861435602,-0.293223633430687,-0.255120882169807,
-0.222254699809382,-0.209457603808669,-0.197591336071566,-0.129828723489989,
-0.0994569524648762,-0.079786402304052,-0.060619434171579,-0.000296546468343627),
 .UNSPECIFIED.);
#302=B_SPLINE_CURVE_WITH_KNOTS('',3,(#22089,#22090,#22091,#22092,#22093,
#22094,#22095,#22096,#22097,#22098,#22099,#22100,#22101,#22102,#22103,#22104,
#22105,#22106,#22107,#22108,#22109,#22110,#22111,#22112,#22113,#22114,#22115,
#22116,#22117,#22118,#22119,#22120,#22121,#22122,#22123,#22124,#22125,#22126,
#22127,#22128,#22129,#22130,#22131,#22132,#22133,#22134,#22135,#22136,#22137,
#22138,#22139,#22140,#22141,#22142,#22143,#22144,#22145,#22146,#22147,#22148,
#22149,#22150,#22151,#22152,#22153,#22154,#22155,#22156,#22157,#22158,#22159,
#22160,#22161,#22162,#22163,#22164,#22165,#22166,#22167,#22168,#22169,#22170,
#22171,#22172,#22173,#22174,#22175,#22176,#22177,#22178,#22179,#22180,#22181,
#22182,#22183,#22184,#22185,#22186,#22187,#22188,#22189,#22190,#22191,#22192,
#22193,#22194,#22195,#22196,#22197,#22198,#22199,#22200,#22201,#22202,#22203,
#22204,#22205,#22206,#22207,#22208,#22209,#22210,#22211,#22212,#22213,#22214,
#22215,#22216,#22217,#22218,#22219,#22220,#22221,#22222,#22223,#22224,#22225,
#22226,#22227),.UNSPECIFIED.,.F.,.F.,(4,3,3,3,3,3,3,3,3,3,3,3,3,3,3,3,3,
3,3,3,3,3,3,3,3,3,3,3,3,3,3,3,3,3,3,3,3,3,3,3,3,3,3,3,3,3,4),(11.6154215191107,
11.7037890220323,11.792149404157,11.88052357879,11.9688971865904,12.0572944191562,
12.1145577438013,12.2021423255354,12.2897048061461,12.3772666890726,12.4648219322771,
12.5523990053126,12.6136939684918,12.7016932197362,12.7896766558619,12.8776648682661,
12.9656484882494,13.0536532570389,13.1128301931823,13.2006194523635,13.2883899961423,
13.3761630672174,13.4639307927713,13.551720479078,13.6119664178728,13.6998390788243,
13.787694051925,13.8755522709807,13.9634053514766,14.0512799364259,14.1111026425634,
14.1989543387987,14.2867881460337,14.3746251065054,14.4624569262738,14.5503104433313,
14.6102388672539,14.6980876008522,14.7859183567643,14.873752161574,14.9615807742626,
15.0494310323098,15.1093750919444,15.1972366894229,15.2850783147494,15.3729229087857,
15.4568668615432),.UNSPECIFIED.);
#303=B_SPLINE_CURVE_WITH_KNOTS('',3,(#22232,#22233,#22234,#22235,#22236,
#22237,#22238,#22239,#22240,#22241,#22242,#22243,#22244,#22245,#22246,#22247,
#22248,#22249,#22250,#22251,#22252,#22253,#22254,#22255,#22256,#22257,#22258,
#22259,#22260,#22261,#22262,#22263,#22264,#22265,#22266,#22267,#22268,#22269,
#22270,#22271,#22272,#22273,#22274,#22275,#22276,#22277,#22278,#22279,#22280,
#22281,#22282,#22283,#22284,#22285,#22286,#22287,#22288,#22289,#22290,#22291,
#22292,#22293,#22294,#22295,#22296,#22297,#22298,#22299,#22300,#22301,#22302,
#22303,#22304,#22305,#22306,#22307,#22308,#22309,#22310,#22311,#22312,#22313,
#22314,#22315,#22316,#22317,#22318,#22319,#22320,#22321,#22322,#22323,#22324,
#22325,#22326,#22327,#22328,#22329,#22330,#22331,#22332,#22333,#22334,#22335,
#22336,#22337,#22338,#22339,#22340,#22341,#22342,#22343,#22344,#22345,#22346,
#22347,#22348,#22349,#22350,#22351,#22352,#22353,#22354,#22355,#22356,#22357,
#22358,#22359,#22360,#22361,#22362,#22363,#22364,#22365,#22366,#22367,#22368,
#22369,#22370,#22371,#22372,#22373,#22374,#22375,#22376,#22377,#22378,#22379,
#22380,#22381,#22382,#22383,#22384,#22385,#22386,#22387,#22388,#22389,#22390,
#22391,#22392,#22393,#22394,#22395,#22396,#22397,#22398,#22399,#22400,#22401,
#22402,#22403,#22404,#22405,#22406,#22407,#22408,#22409,#22410,#22411,#22412,
#22413,#22414,#22415,#22416,#22417,#22418,#22419,#22420,#22421,#22422,#22423,
#22424,#22425,#22426,#22427,#22428,#22429,#22430,#22431,#22432,#22433,#22434,
#22435,#22436,#22437,#22438,#22439,#22440,#22441,#22442,#22443,#22444,#22445,
#22446,#22447,#22448,#22449,#22450,#22451,#22452,#22453,#22454,#22455,#22456,
#22457,#22458,#22459,#22460,#22461,#22462,#22463,#22464,#22465),
 .UNSPECIFIED.,.F.,.F.,(4,2,2,2,2,2,2,2,2,2,2,2,2,2,2,2,2,2,2,2,2,2,2,2,
2,2,2,2,2,2,2,2,2,2,2,2,2,2,2,2,2,2,2,2,2,2,2,2,2,2,2,2,2,2,2,2,2,2,2,2,
2,2,2,2,2,2,2,2,2,2,2,2,2,2,2,2,2,2,2,2,2,2,2,2,2,2,2,2,2,2,2,2,2,2,2,2,
2,2,2,2,2,2,2,2,2,2,2,2,2,2,2,2,2,2,2,2,4),(-5.59900260275164,-5.57358240255277,
-5.51165284056021,-5.49263343147153,-5.47121234894638,-5.42398221307496,
-5.39516584557432,-5.3812712053524,-5.37134641644009,-5.35916799738254,
-5.32885752303004,-5.26581391524423,-5.24678968929203,-5.22534966611294,
-5.17847547088572,-5.14948182461449,-5.13554812274009,-5.12561293920981,
-5.11346219280575,-5.076415254475,-5.02096939997193,-5.00201805586705,-4.98089140929248,
-4.92791834000774,-4.9018770271356,-4.88862137263518,-4.87872227782179,
-4.8726118309089,-4.85291041528789,-4.80301215700534,-4.77906957765278,
-4.75715086190172,-4.73580964228653,-4.69625405224592,-4.66104010524081,
-4.64031843680571,-4.63018620019017,-4.61504399459285,-4.56657558685244,
-4.53777400190244,-4.51454876625657,-4.49411681288997,-4.45767782720016,
-4.4526939042528,-4.41037080659345,-4.39272768956872,-4.38168137600639,
-4.36302775406093,-4.31072814770884,-4.28703801625921,-4.26524071621447,
-4.24637696734528,-4.20907327992395,-4.16288904681854,-4.15484808569998,
-4.1420653383365,-4.12966941855086,-4.08642028836228,-4.0402578741606,-4.01869842575924,
-3.9970320789072,-3.94774176684927,-3.90851453659152,-3.89595078434686,
-3.88512761203502,-3.83595040185292,-3.80534008288096,-3.78031764295576,
-3.76000978685046,-3.72934084871589,-3.68216354281777,-3.67049623815089,
-3.66268637483629,-3.65014340250904,-3.63930659521469,-3.59045632130235,
-3.54581366141594,-3.52483920545617,-3.50234972282123,-3.45547769134334,
-3.41692070959218,-3.40437177170927,-3.39353894583252,-3.34421499832587,
-3.31369122375166,-3.28870648845562,-3.26839461624078,-3.23764478219075,
-3.19057679959306,-3.17892170112111,-3.17111705729583,-3.15857951209892,
-3.14773912298333,-3.09835172750094,-3.06787083493495,-3.04290480581821,
-3.02259085270363,-2.99180015628655,-2.94478715371729,-2.93313820362214,
-2.9253361890858,-2.91280137576584,-2.90016922072955,-2.86143600694281,
-2.81910702155092,-2.79527683714919,-2.77477688298191,-2.74069060294262,
-2.69060390246969,-2.67256321414734,-2.66152113907093,-2.64330037384373,
-2.62910108771731,-2.56115342594594,-2.54063289062032,-2.51766972993501,
-2.50346624102753),.UNSPECIFIED.);
#304=B_SPLINE_CURVE_WITH_KNOTS('',3,(#22467,#22468,#22469,#22470,#22471,
#22472,#22473,#22474,#22475,#22476,#22477,#22478,#22479),.UNSPECIFIED.,
 .F.,.F.,(4,3,3,3,4),(15.4568668615432,15.5447259441062,15.608511316635,
15.7018829174837,15.707963267949),.UNSPECIFIED.);
#305=B_SPLINE_CURVE_WITH_KNOTS('',3,(#22480,#22481,#22482,#22483,#22484,
#22485,#22486,#22487,#22488,#22489,#22490,#22491,#22492,#22493,#22494,#22495),
 .UNSPECIFIED.,.F.,.F.,(4,1,1,1,1,1,1,1,1,1,1,1,1,4),(15.7079632826947,
16.1076475413255,16.606783766016,17.1059199907065,17.6050562153971,18.1041924400876,
18.6033286647781,19.1024648894686,19.6016011141592,20.1007373388497,20.5998735635402,
21.0990097882307,21.5981460129213,21.7400919742423),.UNSPECIFIED.);
#306=B_SPLINE_CURVE_WITH_KNOTS('',3,(#22501,#22502,#22503,#22504,#22505,
#22506,#22507,#22508,#22509,#22510,#22511,#22512,#22513,#22514,#22515,#22516,
#22517,#22518,#22519,#22520,#22521,#22522,#22523,#22524,#22525,#22526,#22527,
#22528,#22529,#22530,#22531,#22532,#22533,#22534,#22535,#22536,#22537,#22538,
#22539,#22540,#22541,#22542,#22543,#22544,#22545,#22546,#22547,#22548,#22549,
#22550,#22551,#22552,#22553,#22554,#22555,#22556,#22557,#22558,#22559,#22560,
#22561,#22562,#22563,#22564,#22565,#22566,#22567,#22568,#22569,#22570,#22571,
#22572,#22573,#22574,#22575,#22576,#22577,#22578,#22579,#22580,#22581,#22582,
#22583,#22584,#22585,#22586,#22587,#22588,#22589,#22590,#22591,#22592,#22593,
#22594,#22595,#22596,#22597,#22598,#22599,#22600,#22601,#22602,#22603,#22604,
#22605,#22606,#22607,#22608,#22609,#22610,#22611,#22612,#22613,#22614,#22615,
#22616,#22617,#22618,#22619,#22620,#22621,#22622,#22623,#22624,#22625,#22626,
#22627,#22628,#22629,#22630,#22631,#22632,#22633,#22634,#22635,#22636,#22637,
#22638,#22639,#22640,#22641,#22642,#22643,#22644,#22645,#22646,#22647,#22648,
#22649,#22650,#22651,#22652,#22653,#22654,#22655,#22656,#22657,#22658,#22659,
#22660,#22661,#22662,#22663,#22664,#22665,#22666,#22667,#22668,#22669,#22670,
#22671,#22672,#22673,#22674,#22675,#22676,#22677,#22678,#22679,#22680,#22681,
#22682,#22683,#22684,#22685,#22686,#22687,#22688,#22689,#22690,#22691,#22692,
#22693,#22694,#22695,#22696,#22697,#22698,#22699,#22700,#22701,#22702,#22703,
#22704,#22705,#22706,#22707,#22708,#22709,#22710,#22711,#22712,#22713,#22714,
#22715,#22716,#22717,#22718,#22719,#22720,#22721,#22722,#22723,#22724,#22725,
#22726,#22727,#22728,#22729,#22730,#22731,#22732,#22733,#22734,#22735,#22736,
#22737,#22738,#22739,#22740,#22741,#22742,#22743,#22744,#22745,#22746,#22747,
#22748,#22749,#22750,#22751,#22752,#22753,#22754,#22755,#22756,#22757,#22758,
#22759,#22760,#22761,#22762,#22763,#22764,#22765,#22766,#22767,#22768,#22769,
#22770,#22771,#22772,#22773,#22774,#22775,#22776,#22777,#22778),
 .UNSPECIFIED.,.F.,.F.,(4,2,2,2,2,2,2,2,2,2,2,2,2,2,2,2,2,2,2,2,2,2,2,2,
2,2,2,2,2,2,2,2,2,2,2,2,2,2,2,2,2,2,2,2,2,2,2,2,2,2,2,2,2,2,2,2,2,2,2,2,
2,2,2,2,2,2,2,2,2,2,2,2,2,2,2,2,2,2,2,2,2,2,2,2,2,2,2,2,2,2,2,2,2,2,2,2,
2,2,2,2,2,2,2,2,2,2,2,2,2,2,2,2,2,2,2,2,2,2,2,2,2,2,2,2,2,2,2,2,2,2,2,2,
2,2,2,2,2,2,4),(-2.97196746186506,-2.96554523147083,-2.94375453468809,-2.9200782670592,
-2.86789256842528,-2.84913715582557,-2.83808885593877,-2.82053203157918,
-2.77326033280646,-2.73996878261319,-2.72087423787642,-2.69942052484035,
-2.68752647692188,-2.65638477391494,-2.61017277181855,-2.5975304658713,
-2.58500486364593,-2.54754739868587,-2.49346285010931,-2.47449444696937,
-2.45286562308431,-2.44077643098385,-2.38263843636578,-2.36073911712372,
-2.34937078793702,-2.33504290993638,-2.32544974605833,-2.29349861593572,
-2.24826374765408,-2.22919420733565,-2.20770812064741,-2.19577776633339,
-2.17956666855177,-2.12946516239794,-2.11137058604908,-2.1003284331591,
-2.08216188986844,-2.04059787428,-2.001735654572,-1.98279537104709,-1.96112352505991,
-1.91774281422472,-1.88041246503279,-1.86436234421339,-1.85438123978714,
-1.83595214157335,-1.80776113304496,-1.75924403899271,-1.73753185246712,
-1.71601464646001,-1.67292575493603,-1.62589690251005,-1.61368496978913,
-1.60067733179182,-1.59241774917134,-1.56768350400614,-1.51137060711735,
-1.49012079036956,-1.46807935799086,-1.44388203285615,-1.39176253176631,
-1.37388251137214,-1.36283924323199,-1.34444896643786,-1.29620030516498,
-1.26127745363222,-1.24072833206364,-1.21709824679231,-1.18957319606848,
-1.13316976391415,-1.12246831819291,-1.1097036729239,-1.1016804290902,-1.05554123375904,
-1.01815323081825,-0.999286043247915,-0.977493681817305,-0.953813956574885,
-0.901601889460169,-0.882869052147508,-0.871974343344133,-0.871451452338479,
-0.870924972089645,-0.870388005932971,-0.869834385563424,-0.86959819539595,
-0.86933921966252,-0.869052002827504,-0.868729804214971,-0.868364190597761,
-0.867944499445601,-0.867457130185425,-0.866884610757177,-0.866204378022422,
-0.86538720745753,-0.864395236690978,-0.863179555823405,-0.861677384207923,
-0.860450545261345,-0.841979054709722,-0.782582939308917,-0.759313611014873,
-0.748058574936621,-0.729041866799972,-0.68040905134498,-0.642035253523077,
-0.631210144962236,-0.621402342565702,-0.620068238234284,-0.61818748843547,
-0.615436987028471,-0.611397425798984,-0.589422175342839,-0.52922459688947,
-0.523970921706879,-0.504736997211866,-0.485849232861956,-0.462133899145304,
-0.409648415184581,-0.391148480639574,-0.380262466323677,-0.379222988399134,
-0.377003493705187,-0.375282570559809,-0.37102322061783,-0.359245578098004,
-0.327407181154658,-0.281981642284065,-0.262556297193585,-0.243598695643424,
-0.221503920951076,-0.179876928881037,-0.150266609942873,-0.13950151117311,
-0.129683655183871,-0.101666480253791,-0.0344675474333192,-0.0165223660564507,
-7.86535600802601E-5),.UNSPECIFIED.);
#307=B_SPLINE_CURVE_WITH_KNOTS('',3,(#22779,#22780,#22781,#22782,#22783,
#22784,#22785,#22786,#22787,#22788,#22789,#22790,#22791,#22792,#22793,#22794),
 .UNSPECIFIED.,.F.,.F.,(4,2,2,2,2,2,2,4),(-5.72269097713674,-5.7048997707614,
-5.66921491536667,-5.64074759372965,-5.62693046584006,-5.6170261790475,
-5.60479096905175,-5.59900260275164),.UNSPECIFIED.);
#308=B_SPLINE_CURVE_WITH_KNOTS('',3,(#22796,#22797,#22798,#22799),
 .UNSPECIFIED.,.F.,.F.,(4,4),(21.7400919742423,21.9911485668441),
 .UNSPECIFIED.);
#309=B_SPLINE_CURVE_WITH_KNOTS('',3,(#22800,#22801,#22802,#22803,#22804,
#22805,#22806,#22807,#22808,#22809,#22810,#22811,#22812,#22813,#22814,#22815,
#22816,#22817,#22818,#22819,#22820,#22821,#22822,#22823,#22824,#22825,#22826,
#22827,#22828,#22829,#22830,#22831,#22832,#22833,#22834,#22835,#22836,#22837,
#22838,#22839,#22840,#22841,#22842,#22843,#22844,#22845,#22846,#22847,#22848,
#22849,#22850,#22851,#22852,#22853,#22854,#22855,#22856,#22857,#22858,#22859,
#22860,#22861,#22862,#22863,#22864,#22865,#22866,#22867,#22868,#22869,#22870,
#22871,#22872,#22873,#22874,#22875,#22876,#22877,#22878,#22879,#22880,#22881,
#22882,#22883,#22884,#22885,#22886,#22887,#22888,#22889,#22890,#22891,#22892,
#22893,#22894,#22895,#22896,#22897,#22898,#22899,#22900,#22901,#22902,#22903,
#22904,#22905,#22906,#22907,#22908,#22909,#22910,#22911,#22912,#22913,#22914,
#22915,#22916,#22917,#22918,#22919,#22920,#22921,#22922,#22923,#22924,#22925,
#22926,#22927,#22928,#22929,#22930,#22931,#22932,#22933,#22934,#22935,#22936,
#22937,#22938,#22939,#22940,#22941,#22942,#22943,#22944,#22945,#22946,#22947,
#22948,#22949,#22950,#22951,#22952,#22953,#22954,#22955,#22956,#22957,#22958,
#22959,#22960,#22961,#22962,#22963,#22964,#22965,#22966,#22967,#22968,#22969,
#22970,#22971,#22972,#22973,#22974,#22975,#22976,#22977,#22978,#22979,#22980,
#22981,#22982,#22983,#22984,#22985,#22986,#22987,#22988,#22989,#22990,#22991,
#22992,#22993,#22994,#22995,#22996,#22997,#22998,#22999,#23000,#23001,#23002,
#23003,#23004,#23005,#23006,#23007,#23008,#23009,#23010,#23011,#23012,#23013,
#23014,#23015,#23016,#23017,#23018,#23019),.UNSPECIFIED.,.F.,.F.,(4,3,3,
3,3,3,3,3,3,3,3,3,3,3,3,3,3,3,3,3,3,3,3,3,3,3,3,3,3,3,3,3,3,3,3,3,3,3,3,
3,3,3,3,3,3,3,3,3,3,3,3,3,3,3,3,3,3,3,3,3,3,3,3,3,3,3,3,3,3,3,3,3,3,4),
(21.9911485751286,22.0842384360753,22.0972822376118,22.1851351036133,22.2729700638413,
22.3608081401585,22.448641052211,22.5364956141511,22.5964184623023,22.6842713276911,
22.7721062872985,22.8599443629887,22.9477772744123,23.0356318357261,23.0955546869928,
23.1834075526208,23.27124251247,23.3590805884042,23.4469135000723,23.5347680616292,
23.5946909116834,23.6825437772571,23.7703787370515,23.8582168129308,23.9460497245441,
24.0339042860466,24.0938271363739,24.1816800019336,24.2695149617138,24.3573530375785,
24.4451859491769,24.5330405106645,24.5929633610644,24.6808162266509,24.7686511864583,
24.8564892623505,24.9443221739767,25.032176735492,25.092099585755,25.1799524513211,
25.2677874111078,25.355625486979,25.4434583985842,25.5313129600785,25.5912358104455,
25.6790886760229,25.766923635821,25.8547617117038,25.9425946233205,26.0304491848264,
26.090372035136,26.1782249007086,26.2660598605019,26.3538979363798,26.4417308479916,
26.5295854094927,26.5895082598265,26.6773611254005,26.7651960851951,26.8530341610745,
26.9408670726877,27.0287216341901,27.0886444845171,27.1764973500911,27.2643323098857,
27.352170385765,27.4400032973782,27.5278578588806,27.5877807092076,27.675632926961,
27.7634773101345,27.8513089857246,27.939155693041,28.0232375357607),
 .UNSPECIFIED.);
#310=B_SPLINE_CURVE_WITH_KNOTS('',3,(#23024,#23025,#23026,#23027,#23028,
#23029,#23030,#23031,#23032,#23033,#23034,#23035,#23036,#23037,#23038,#23039,
#23040,#23041,#23042,#23043,#23044,#23045,#23046,#23047,#23048,#23049,#23050,
#23051,#23052,#23053,#23054,#23055,#23056,#23057,#23058,#23059,#23060,#23061,
#23062,#23063,#23064,#23065,#23066,#23067,#23068,#23069,#23070,#23071,#23072,
#23073,#23074,#23075,#23076,#23077,#23078,#23079,#23080,#23081,#23082,#23083,
#23084,#23085,#23086,#23087,#23088,#23089,#23090,#23091,#23092,#23093,#23094,
#23095,#23096,#23097,#23098,#23099,#23100,#23101,#23102,#23103,#23104,#23105,
#23106,#23107,#23108,#23109,#23110,#23111,#23112,#23113,#23114,#23115,#23116,
#23117,#23118,#23119,#23120,#23121,#23122,#23123,#23124,#23125,#23126,#23127,
#23128,#23129,#23130,#23131,#23132,#23133,#23134,#23135,#23136,#23137,#23138,
#23139,#23140,#23141,#23142,#23143,#23144,#23145,#23146,#23147,#23148,#23149,
#23150,#23151,#23152,#23153,#23154,#23155,#23156,#23157,#23158,#23159,#23160,
#23161,#23162,#23163,#23164,#23165,#23166,#23167,#23168,#23169,#23170,#23171,
#23172,#23173,#23174,#23175,#23176,#23177,#23178,#23179,#23180,#23181,#23182,
#23183,#23184,#23185,#23186,#23187,#23188,#23189,#23190,#23191,#23192,#23193,
#23194,#23195,#23196,#23197,#23198,#23199,#23200,#23201,#23202,#23203,#23204,
#23205,#23206,#23207,#23208,#23209,#23210,#23211,#23212,#23213,#23214,#23215,
#23216,#23217,#23218,#23219,#23220,#23221,#23222,#23223,#23224,#23225,#23226,
#23227,#23228,#23229,#23230,#23231,#23232,#23233,#23234,#23235,#23236,#23237,
#23238,#23239,#23240,#23241,#23242,#23243,#23244,#23245,#23246,#23247,#23248,
#23249,#23250,#23251,#23252,#23253,#23254,#23255,#23256,#23257,#23258,#23259,
#23260,#23261,#23262,#23263,#23264,#23265,#23266,#23267,#23268,#23269,#23270,
#23271,#23272,#23273,#23274,#23275,#23276,#23277,#23278,#23279,#23280,#23281,
#23282,#23283,#23284,#23285,#23286,#23287,#23288,#23289,#23290,#23291,#23292,
#23293,#23294,#23295,#23296,#23297,#23298,#23299,#23300,#23301,#23302,#23303,
#23304,#23305,#23306,#23307,#23308,#23309,#23310,#23311,#23312,#23313,#23314,
#23315,#23316,#23317,#23318,#23319,#23320,#23321,#23322,#23323,#23324,#23325),
 .UNSPECIFIED.,.F.,.F.,(4,2,2,2,2,2,2,2,2,2,2,2,2,2,2,2,2,2,2,2,2,2,2,2,
2,2,2,2,2,2,2,2,2,2,2,2,2,2,2,2,2,2,2,2,2,2,2,2,2,2,2,2,2,2,2,2,2,2,2,2,
2,2,2,2,2,2,2,2,2,2,2,2,2,2,2,2,2,2,2,2,2,2,2,2,2,2,2,2,2,2,2,2,2,2,2,2,
2,2,2,2,2,2,2,2,2,2,2,2,2,2,2,2,2,2,2,2,2,2,2,2,2,2,2,2,2,2,2,2,2,2,2,2,
2,2,2,2,2,2,2,2,2,2,2,2,2,2,2,2,2,2,4),(-6.06758662286169,-6.05672118825285,
-6.04398051113079,-6.0334226331625,-6.01645295742768,-5.96666224032135,
-5.94114870105503,-5.92208655058119,-5.91518501487488,-5.8934594205242,
-5.84516952494057,-5.81686818659048,-5.80779422838678,-5.79443767954243,
-5.79349800157478,-5.78139613242103,-5.74401084754885,-5.70741227554712,
-5.68623075021572,-5.6675727357668,-5.64882559886436,-5.58864345832522,
-5.5666613677867,-5.56355015090866,-5.56159369713408,-5.56033134932902,
-5.55949467533685,-5.55892676896793,-5.5576607109228,-5.55654449748931,
-5.55553499768505,-5.55459418941356,-5.55368497778539,-5.55276492868988,
-5.55177336537258,-5.54087185868793,-5.5219755565811,-5.47140328296167,
-5.44725177462835,-5.42865316832329,-5.42216638709216,-5.41919045683931,
-5.3956199805333,-5.3361070297681,-5.31762079130934,-5.31656252102421,-5.3157355291818,
-5.31508399021442,-5.31456676757517,-5.31415332858434,-5.31382081068278,
-5.31355192854873,-5.3128676449826,-5.31223466419711,-5.31164612693527,
-5.31109596225334,-5.31057875703017,-5.31008964022883,-5.30962417776799,
-5.30917827411671,-5.30874807656039,-5.3083298774212,-5.30792000816874,
-5.30751471697572,-5.30711001706769,-5.30670148574894,-5.2956590562236,
-5.27765940673098,-5.22457788682926,-5.20078636996917,-5.17894020571089,
-5.16010343352462,-5.11847597057348,-5.08311004235011,-5.06790088348071,
-5.05531648675626,-5.04273421768311,-5.0031222086333,-4.96535122427611,
-4.95343436929804,-4.93196026441603,-4.91020054069653,-4.86251208498258,
-4.83392024190604,-4.81534636325053,-4.80535799733817,-4.78940550815818,
-4.73389901708083,-4.70980469701429,-4.6878128270867,-4.66905181585447,
-4.60130973741285,-4.58154842692496,-4.56663799035407,-4.55543071779441,
-4.53245022824654,-4.47443858681815,-4.46238716115369,-4.44079230976937,
-4.42180096123763,-4.36313103880956,-4.33923779230291,-4.33115234655257,
-4.31832361029933,-4.30765787948439,-4.2543917421821,-4.22186452681116,
-4.1988154916661,-4.17832496274169,-4.1094394811482,-4.09555848268397,-4.07757565161444,
-4.06653305458312,-4.04825149061814,-3.99675856673836,-3.97257833171424,
-3.95054491909916,-3.92928909844223,-3.87282789977919,-3.84819289792589,
-3.83113291561169,-3.82006763470954,-3.80067290596053,-3.75009256408658,
-3.72621861706015,-3.70433270841676,-3.68551715512471,-3.62268318677427,
-3.59082819880285,-3.5790428179909,-3.56535289758157,-3.50498071401217,
-3.48086804822901,-3.45886723926148,-3.43758778758782,-3.38091392375934,
-3.34779794910163,-3.33504250496864,-3.32262183945877,-3.27979225686106,
-3.23286871133276,-3.21139990690842,-3.19231689299758,-3.14874343295967,
-3.11572311208957,-3.0956648088067,-3.08457342216825,-3.06795378935973,
-3.0218279603193,-2.98441336346076,-2.97196746186506),.UNSPECIFIED.);
#311=B_SPLINE_CURVE_WITH_KNOTS('',3,(#23327,#23328,#23329,#23330,#23331,
#23332,#23333,#23334,#23335,#23336),.UNSPECIFIED.,.F.,.F.,(4,3,3,4),(28.0232375357607,
28.0869169338981,28.1806254081031,28.2743338823082),.UNSPECIFIED.);
#312=B_SPLINE_CURVE_WITH_KNOTS('',3,(#23337,#23338,#23339,#23340,#23341,
#23342,#23343,#23344,#23345,#23346,#23347,#23348,#23349,#23350,#23351,#23352,
#23353,#23354,#23355,#23356,#23357,#23358,#23359,#23360,#23361,#23362,#23363,
#23364,#23365,#23366,#23367,#23368,#23369,#23370,#23371,#23372,#23373,#23374,
#23375,#23376,#23377,#23378,#23379,#23380,#23381,#23382,#23383,#23384,#23385,
#23386,#23387,#23388,#23389,#23390,#23391,#23392,#23393,#23394,#23395,#23396,
#23397,#23398,#23399,#23400,#23401,#23402,#23403,#23404,#23405,#23406,#23407,
#23408,#23409,#23410,#23411,#23412,#23413,#23414,#23415,#23416,#23417,#23418,
#23419,#23420,#23421,#23422,#23423,#23424,#23425,#23426,#23427,#23428,#23429,
#23430,#23431,#23432,#23433,#23434,#23435,#23436,#23437,#23438,#23439,#23440,
#23441,#23442,#23443,#23444,#23445,#23446,#23447,#23448,#23449,#23450,#23451,
#23452,#23453,#23454,#23455,#23456,#23457,#23458,#23459,#23460,#23461,#23462,
#23463,#23464,#23465,#23466,#23467,#23468,#23469,#23470,#23471,#23472,#23473,
#23474,#23475,#23476,#23477,#23478,#23479,#23480,#23481,#23482,#23483,#23484,
#23485,#23486,#23487,#23488,#23489,#23490,#23491,#23492,#23493,#23494,#23495,
#23496,#23497,#23498,#23499,#23500,#23501,#23502,#23503,#23504,#23505,#23506,
#23507,#23508,#23509,#23510,#23511,#23512,#23513,#23514,#23515,#23516,#23517,
#23518,#23519,#23520,#23521,#23522,#23523,#23524,#23525,#23526,#23527,#23528,
#23529,#23530,#23531,#23532,#23533,#23534,#23535,#23536,#23537,#23538,#23539,
#23540,#23541,#23542,#23543,#23544,#23545,#23546,#23547,#23548,#23549,#23550,
#23551,#23552,#23553,#23554,#23555,#23556,#23557,#23558,#23559,#23560,#23561,
#23562,#23563,#23564,#23565,#23566,#23567,#23568,#23569,#23570,#23571,#23572,
#23573,#23574,#23575,#23576,#23577,#23578,#23579,#23580,#23581,#23582,#23583,
#23584,#23585,#23586,#23587,#23588,#23589,#23590,#23591,#23592,#23593,#23594,
#23595,#23596,#23597,#23598,#23599,#23600,#23601,#23602,#23603,#23604,#23605,
#23606,#23607,#23608,#23609,#23610,#23611,#23612,#23613,#23614,#23615,#23616,
#23617,#23618,#23619,#23620),.UNSPECIFIED.,.F.,.F.,(4,2,2,2,2,2,2,2,2,2,
2,2,2,2,2,2,2,2,2,2,2,2,2,2,2,2,2,2,2,2,2,2,2,2,2,2,2,2,2,2,2,2,2,2,2,2,
2,2,2,2,2,2,2,2,2,2,2,2,2,2,2,2,2,2,2,2,2,2,2,2,2,2,2,2,2,2,2,2,2,2,2,2,
2,2,2,2,2,2,2,2,2,2,2,2,2,2,2,2,2,2,2,2,2,2,2,2,2,2,2,2,2,2,2,2,2,2,2,2,
2,2,2,2,2,2,2,2,2,2,2,2,2,2,2,2,2,2,2,2,2,2,2,4),(-6.19174977417099,-6.17790055894357,
-6.16530844262692,-6.14488062628941,-6.11016394335594,-6.05746865424026,
-6.04395990877691,-6.03345737334001,-6.01671312488883,-5.96693939896737,
-5.94108351866951,-5.92183282063829,-5.91339110029996,-5.89094141021784,
-5.84321905355417,-5.81582671700227,-5.80705047866299,-5.79376231777089,
-5.79283345590746,-5.78046847860075,-5.75110684024062,-5.70992911883133,
-5.68781295060037,-5.66839735790778,-5.64985257178812,-5.58453612918225,
-5.56437800196991,-5.56185865109168,-5.56024447158564,-5.55917924296637,
-5.55845613724759,-5.55714597697236,-5.5559893725437,-5.55494108762057,
-5.55396078138865,-5.5530082564484,-5.55203588284284,-5.54147642800634,
-5.52457428735703,-5.47472865740141,-5.44900954047236,-5.42977729035764,
-5.42205833795195,-5.41902630307087,-5.41614286536467,-5.39146794003943,
-5.33472194871901,-5.31650090691653,-5.31550703188536,-5.31472580806067,
-5.31410649336461,-5.31361164388215,-5.31321340678309,-5.31289086926891,
-5.31262817114584,-5.31194633479694,-5.3113140118618,-5.31072444801069,
-5.31017164063459,-5.30965020797847,-5.30915527141661,-5.30868234635121,
-5.30822723719189,-5.30778593130822,-5.30735448554185,-5.30692889644243,
-5.29573799550333,-5.27907634992805,-5.22435293542331,-5.20025642266531,
-5.1781773307116,-5.15915929913742,-5.12126130497449,-5.07456457511193,
-5.06676062206611,-5.05419163944611,-5.04130164166706,-5.0087161772395,
-4.96034832777065,-4.93645306482614,-4.91570524324687,-4.88014968311171,
-4.83865893376585,-4.82238056721064,-4.80919322439788,-4.79686877353386,
-4.76471717714858,-4.73337436413831,-4.70897605865634,-4.68675245002698,
-4.66525730794326,-4.6008837523092,-4.58069467204775,-4.56555050419774,
-4.55423614060313,-4.53600703437018,-4.48510939633242,-4.46150698067304,
-4.43966322989653,-4.41784287826541,-4.36852982104803,-4.32914466389923,
-4.31651089497893,-4.30369093417459,-4.26608021284519,-4.21760521409203,
-4.19524853232157,-4.17384677045649,-4.11742965631162,-4.09260597282443,
-4.08431152843695,-4.07123722613881,-4.06050864990156,-4.00710393798522,
-3.97442997609026,-3.95126494422135,-3.93052607211835,-3.86413107294597,
-3.84928816341928,-3.83055785684892,-3.81940148587177,-3.80130100514156,
-3.74849319904076,-3.72448780047543,-3.70245210051695,-3.68080770527405,
-3.61907787523084,-3.58877090111763,-3.57698016609012,-3.5628675431258,
-3.47781268181903,-3.45594630129282,-3.43680114361935,-3.37783159005303,
-3.35401276423705,-3.3459267790151,-3.3330665613329,-3.32047046038928,-3.27960629669956,
-3.24448573447427,-3.2321624904099,-3.21960145114545),.UNSPECIFIED.);
#313=B_SPLINE_CURVE_WITH_KNOTS('',3,(#23626,#23627,#23628,#23629,#23630,
#23631,#23632,#23633,#23634,#23635,#23636,#23637,#23638,#23639,#23640,#23641,
#23642,#23643,#23644,#23645,#23646,#23647,#23648,#23649,#23650,#23651,#23652,
#23653,#23654,#23655,#23656,#23657,#23658,#23659,#23660,#23661,#23662,#23663,
#23664,#23665,#23666,#23667,#23668,#23669,#23670,#23671,#23672,#23673,#23674,
#23675,#23676,#23677,#23678,#23679,#23680,#23681,#23682,#23683,#23684,#23685,
#23686,#23687,#23688,#23689,#23690,#23691,#23692,#23693,#23694,#23695,#23696,
#23697,#23698,#23699,#23700,#23701,#23702,#23703,#23704,#23705,#23706,#23707,
#23708,#23709,#23710,#23711,#23712,#23713,#23714,#23715,#23716,#23717,#23718,
#23719,#23720,#23721,#23722,#23723,#23724,#23725,#23726,#23727,#23728,#23729,
#23730,#23731,#23732,#23733,#23734,#23735,#23736,#23737,#23738,#23739,#23740,
#23741,#23742,#23743,#23744,#23745,#23746,#23747,#23748,#23749,#23750,#23751,
#23752,#23753,#23754,#23755,#23756,#23757,#23758,#23759,#23760,#23761,#23762,
#23763,#23764,#23765,#23766,#23767,#23768,#23769,#23770,#23771,#23772,#23773,
#23774,#23775,#23776,#23777,#23778,#23779,#23780,#23781,#23782,#23783,#23784,
#23785,#23786,#23787,#23788,#23789,#23790,#23791,#23792,#23793,#23794,#23795,
#23796,#23797,#23798,#23799,#23800,#23801,#23802,#23803,#23804,#23805,#23806,
#23807,#23808,#23809,#23810,#23811,#23812,#23813,#23814,#23815,#23816,#23817,
#23818,#23819,#23820,#23821,#23822,#23823,#23824,#23825,#23826,#23827,#23828,
#23829,#23830,#23831,#23832,#23833,#23834,#23835,#23836,#23837,#23838,#23839,
#23840,#23841,#23842),.UNSPECIFIED.,.F.,.F.,(4,3,3,3,3,3,3,3,3,3,3,3,3,
3,3,3,3,3,3,3,3,3,3,3,3,3,3,3,3,3,3,3,3,3,3,3,3,3,3,3,3,3,3,3,3,3,3,3,3,
3,3,3,3,3,3,3,3,3,3,3,3,3,3,3,3,3,3,3,3,3,3,3,4),(34.5575191894878,34.6518273097851,
34.7461354300824,34.8339898030957,34.9218262952673,35.0096659023973,35.0975003577409,
35.1853564084918,35.2450073652305,35.3328617382438,35.4206982304155,35.5085378375455,
35.5963722928892,35.6842283436401,35.7438793003786,35.8317336733919,35.9195701655634,
36.0074097726934,36.0952442280371,36.183100278788,36.2427512355268,36.3306056085401,
36.4184421007117,36.5062817078417,36.5941161631853,36.6819722139362,36.7416231706749,
36.8294775436881,36.9173140358597,37.0051536429896,37.0929880983332,37.1808441490841,
37.240495105823,37.3283494788363,37.4161859710079,37.504025578138,37.5918600334816,
37.6797160842325,37.7393670409711,37.8272214139844,37.915057906156,38.002897513286,
38.0907319686296,38.1785880193805,38.2382389761193,38.3260933491326,38.4139298413042,
38.5017694484342,38.5896039037779,38.6774599545289,38.7371109112674,38.8249652842806,
38.9128017764521,39.000641383582,39.0884758389256,39.1763318896765,39.2359828464155,
39.3238372194288,39.4116737116004,39.4995133187305,39.5873477740742,39.6752038248252,
39.7348547815636,39.8227091545768,39.9105456467483,39.9983852538783,40.0862197092219,
40.1740757599728,40.2337267167118,40.3226968924185,40.4105362766921,40.5000718481154,
40.5896074195387),.UNSPECIFIED.);
#314=B_SPLINE_CURVE_WITH_KNOTS('',3,(#23843,#23844,#23845,#23846,#23847,
#23848,#23849,#23850,#23851,#23852,#23853,#23854),.UNSPECIFIED.,.F.,.F.,
(4,2,2,2,2,4),(-6.1912980755545,-6.1778196623817,-6.16552121345783,-6.14529911471674,
-6.11138976728743,-6.06758662286169),.UNSPECIFIED.);
#315=B_SPLINE_CURVE_WITH_KNOTS('',3,(#23855,#23856,#23857,#23858,#23859,
#23860,#23861,#23862,#23863,#23864,#23865,#23866,#23867,#23868,#23869,#23870,
#23871,#23872,#23873,#23874,#23875,#23876,#23877,#23878,#23879,#23880,#23881,
#23882,#23883,#23884,#23885,#23886,#23887,#23888,#23889,#23890,#23891,#23892,
#23893,#23894,#23895,#23896,#23897,#23898,#23899,#23900,#23901,#23902,#23903,
#23904,#23905,#23906,#23907,#23908,#23909,#23910,#23911,#23912,#23913,#23914,
#23915,#23916,#23917,#23918,#23919,#23920,#23921,#23922,#23923,#23924,#23925,
#23926,#23927,#23928,#23929,#23930,#23931,#23932,#23933,#23934,#23935,#23936,
#23937,#23938,#23939,#23940,#23941,#23942,#23943,#23944,#23945,#23946,#23947,
#23948,#23949,#23950,#23951,#23952,#23953,#23954,#23955,#23956,#23957,#23958,
#23959,#23960,#23961,#23962,#23963,#23964,#23965,#23966,#23967,#23968,#23969,
#23970,#23971,#23972,#23973,#23974,#23975,#23976,#23977,#23978,#23979,#23980,
#23981,#23982,#23983,#23984,#23985,#23986,#23987,#23988,#23989,#23990,#23991,
#23992,#23993,#23994,#23995,#23996,#23997,#23998,#23999,#24000,#24001,#24002,
#24003,#24004,#24005,#24006,#24007,#24008,#24009,#24010,#24011,#24012,#24013,
#24014,#24015,#24016,#24017,#24018,#24019,#24020,#24021,#24022,#24023,#24024,
#24025,#24026,#24027,#24028,#24029,#24030,#24031,#24032,#24033,#24034,#24035,
#24036,#24037,#24038,#24039,#24040,#24041,#24042,#24043,#24044,#24045,#24046,
#24047,#24048,#24049,#24050,#24051,#24052,#24053,#24054,#24055,#24056,#24057,
#24058,#24059,#24060,#24061,#24062,#24063,#24064,#24065,#24066,#24067,#24068,
#24069,#24070,#24071,#24072,#24073,#24074,#24075,#24076,#24077,#24078,#24079,
#24080,#24081,#24082,#24083,#24084,#24085,#24086,#24087,#24088,#24089,#24090,
#24091,#24092,#24093,#24094,#24095,#24096,#24097,#24098,#24099,#24100,#24101,
#24102),.UNSPECIFIED.,.F.,.F.,(4,2,2,2,2,2,2,2,2,2,2,2,2,2,2,2,2,2,2,2,
2,2,2,2,2,2,2,2,2,2,2,2,2,2,2,2,2,2,2,2,2,2,2,2,2,2,2,2,2,2,2,2,2,2,2,2,
2,2,2,2,2,2,2,2,2,2,2,2,2,2,2,2,2,2,2,2,2,2,2,2,2,2,2,2,2,2,2,2,2,2,2,2,
2,2,2,2,2,2,2,2,2,2,2,2,2,2,2,2,2,2,2,2,2,2,2,2,2,2,2,2,2,2,2,4),(-3.21960145114545,
-3.21022947980482,-3.19112654555098,-3.12190443326165,-3.09587143195948,
-3.08443680155034,-3.06975920450714,-3.05054634619234,-2.98342362393314,
-2.9642023801869,-2.94244696641799,-2.93032115889807,-2.87179626716825,
-2.84993062193197,-2.83849524516932,-2.82382056968935,-2.80461365150436,
-2.73747429472207,-2.71825414929352,-2.6964975555484,-2.68437034145876,
-2.62584826119843,-2.60398569176725,-2.59255083537871,-2.57787477984499,
-2.55866494068083,-2.49153507515123,-2.47231455933765,-2.45055882323833,
-2.43843248183758,-2.37990893501068,-2.35804534744514,-2.3466103957743,
-2.33193504074819,-2.31272656637389,-2.24559355529108,-2.22637337949345,
-2.2046175153028,-2.19249094397454,-2.1339684033277,-2.11210553979271,-2.10067075481821,
-2.08599521481463,-2.06678628118138,-1.999655502551,-1.98043536443547,-1.9586797916078,
-1.94655345954775,-1.88803101997814,-1.86616805217765,-1.85473330934196,
-1.84005800533958,-1.82084947963615,-1.75371837659818,-1.73449841990162,
-1.7127429390072,-1.70061662313771,-1.64209473571131,-1.62023204519314,
-1.6087974018717,-1.59412213994422,-1.57491362269492,-1.50778337306259,
-1.48856353157109,-1.46680823447338,-1.45468203755197,-1.3961604996727,
-1.37429790761334,-1.36286333691478,-1.34818820794881,-1.32897988637461,
-1.2618499381358,-1.24263024288065,-1.22087508652415,-1.20874896039024,
-1.15022786805139,-1.12836545764103,-1.11693097207478,-1.10225593378729,
-1.08304772078849,-1.01591833074346,-0.99669876728702,-0.974943771699952,
-0.962817738757497,-0.904297047533957,-0.882434779930312,-0.870962174567235,
-0.860513830808857,-0.859315401260965,-0.857322528650568,-0.854023333159055,
-0.832319673335272,-0.771005489349052,-0.751900051905642,-0.732659958985613,
-0.710803786802656,-0.671104247453748,-0.639253207951319,-0.626917177408989,
-0.616905504178548,-0.614457072570467,-0.611372041135868,-0.608511309618207,
-0.587273001283989,-0.524787244576754,-0.512229481817021,-0.491917860624872,
-0.471652228619173,-0.455383098515217,-0.40103038495825,-0.38539648417881,
-0.374160267884775,-0.37006891953753,-0.367619896947356,-0.344190706999339,
-0.278024281148239,-0.25785169605832,-0.238760867794644,-0.21606878029411,
-0.17140056146557,-0.149906130813608,-0.136588295513562,-0.126447364794008,
-0.123761332807637),.UNSPECIFIED.);
#316=B_SPLINE_CURVE_WITH_KNOTS('',3,(#24108,#24109,#24110,#24111,#24112,
#24113,#24114,#24115,#24116,#24117,#24118,#24119,#24120,#24121,#24122,#24123,
#24124,#24125,#24126,#24127,#24128,#24129,#24130,#24131,#24132,#24133,#24134,
#24135,#24136,#24137,#24138,#24139,#24140,#24141,#24142,#24143,#24144,#24145,
#24146,#24147,#24148,#24149,#24150,#24151,#24152,#24153,#24154,#24155,#24156,
#24157,#24158,#24159,#24160,#24161,#24162,#24163,#24164,#24165,#24166,#24167,
#24168,#24169,#24170,#24171,#24172,#24173,#24174,#24175,#24176,#24177,#24178,
#24179,#24180,#24181,#24182,#24183,#24184,#24185,#24186,#24187,#24188,#24189,
#24190,#24191,#24192,#24193,#24194,#24195,#24196,#24197,#24198,#24199,#24200,
#24201,#24202,#24203,#24204,#24205,#24206,#24207,#24208,#24209,#24210,#24211,
#24212,#24213,#24214,#24215,#24216,#24217,#24218,#24219,#24220,#24221,#24222,
#24223,#24224,#24225,#24226,#24227,#24228,#24229,#24230,#24231,#24232,#24233,
#24234,#24235,#24236,#24237,#24238,#24239,#24240,#24241,#24242,#24243,#24244,
#24245,#24246,#24247,#24248,#24249,#24250,#24251,#24252,#24253,#24254,#24255,
#24256,#24257,#24258,#24259,#24260,#24261,#24262,#24263,#24264,#24265,#24266,
#24267,#24268,#24269,#24270,#24271,#24272,#24273,#24274,#24275,#24276,#24277,
#24278,#24279,#24280,#24281,#24282,#24283,#24284,#24285,#24286,#24287,#24288,
#24289,#24290,#24291,#24292,#24293,#24294,#24295,#24296,#24297,#24298,#24299,
#24300,#24301,#24302,#24303,#24304,#24305,#24306,#24307,#24308,#24309,#24310,
#24311,#24312,#24313,#24314,#24315,#24316,#24317,#24318,#24319,#24320,#24321,
#24322,#24323,#24324,#24325,#24326,#24327,#24328,#24329,#24330,#24331,#24332,
#24333,#24334,#24335,#24336,#24337,#24338,#24339,#24340,#24341,#24342,#24343,
#24344,#24345,#24346,#24347,#24348,#24349,#24350,#24351),.UNSPECIFIED.,
 .F.,.F.,(4,2,2,2,2,2,2,2,2,2,2,2,2,2,2,2,2,2,2,2,2,2,2,2,2,2,2,2,2,2,2,
2,2,2,2,2,2,2,2,2,2,2,2,2,2,2,2,2,2,2,2,2,2,2,2,2,2,2,2,2,2,2,2,2,2,2,2,
2,2,2,2,2,2,2,2,2,2,2,2,2,2,2,2,2,2,2,2,2,2,2,2,2,2,2,2,2,2,2,2,2,2,2,2,
2,2,2,2,2,2,2,2,2,2,2,2,2,2,2,2,2,2,4),(-2.97193325191145,-2.97164574381583,
-2.92102915801035,-2.90216692995615,-2.89111652013216,-2.87364861696247,
-2.82834372839519,-2.79144189690155,-2.7725982633729,-2.75076459223857,
-2.72699873701708,-2.67412231978996,-2.65595025215559,-2.64490809658809,
-2.62681899905642,-2.59954947584692,-2.55088088755474,-2.52883403008647,
-2.50758810140748,-2.45918934095238,-2.41685203979126,-2.40440363217966,
-2.39167904182718,-2.35884312687339,-2.34683759451771,-2.30118673634944,
-2.28212551253655,-2.26062832232885,-2.21249860315353,-2.17121832592259,
-2.15871404305064,-2.14604947757248,-2.13069328305726,-2.09450777103372,
-2.05469867866883,-2.03575910358966,-2.01408606064914,-1.9906554093374,
-1.94030618555707,-1.91990714178543,-1.9087997095913,-1.89238140091297,
-1.84650605846805,-1.80913980932642,-1.79016332429391,-1.76854676503619,
-1.75647112571681,-1.6980228099185,-1.67521535554473,-1.66396397111819,
-1.64862466304223,-1.60311662207386,-1.59700382718513,-1.5606621987561,
-1.54023539541018,-1.51699241246588,-1.48722028339018,-1.4314293137659,
-1.42085859124806,-1.4078453244037,-1.39958021464946,-1.35284846971754,
-1.3163753382843,-1.29758967640907,-1.27564723889801,-1.25165523263094,
-1.20173448753213,-1.18213389128223,-1.17106146744814,-1.15414593661864,
-1.12986344755896,-1.0722881894719,-1.05322543523818,-1.03173062852031,
-0.983967850883072,-0.942252395241978,-0.929770736403734,-0.917082329125133,
-0.901682142448709,-0.865247592264209,-0.825920341281493,-0.805248539838595,
-0.787460996593727,-0.76508144518638,-0.721751826282113,-0.695141924529433,
-0.68320670260102,-0.671960376617552,-0.670929298408179,-0.669720700601747,
-0.668276479581411,-0.650390392697354,-0.596212681215645,-0.572559135833189,
-0.557121076167727,-0.534388274815794,-0.508039114692328,-0.457135112408879,
-0.441744518263323,-0.43127672360959,-0.428685155619503,-0.426521220034364,
-0.423430915281326,-0.417764335747122,-0.394747082652951,-0.334119006313926,
-0.313491193834681,-0.311501757358665,-0.309706484477112,-0.307017635846705,
-0.281560258528114,-0.24929703766151,-0.211831127423816,-0.196354387224509,
-0.185900936827732,-0.167273217435851,-0.13699596743803,-0.0887764016844955,
-0.0697834210280926,-0.0508249785909599,-0.033290469383095,-7.60621500899032E-5),
 .UNSPECIFIED.);
#317=B_SPLINE_CURVE_WITH_KNOTS('',3,(#24352,#24353,#24354,#24355,#24356,
#24357,#24358,#24359,#24360,#24361,#24362,#24363,#24364),.UNSPECIFIED.,
 .F.,.F.,(4,3,3,3,4),(40.5896074195387,40.677463067737,40.7325986518599,
40.8255995484923,40.8407044966674),.UNSPECIFIED.);
#318=B_SPLINE_CURVE_WITH_KNOTS('',3,(#24366,#24367,#24368,#24369,#24370,
#24371,#24372,#24373,#24374,#24375),.UNSPECIFIED.,.F.,.F.,(4,2,2,2,4),(-0.123761332807637,
-0.100838124130903,-0.0326226656386009,-0.0154724073688336,-4.23457580937261E-5),
 .UNSPECIFIED.);
#319=B_SPLINE_CURVE_WITH_KNOTS('',3,(#24376,#24377,#24378,#24379,#24380,
#24381,#24382,#24383,#24384,#24385,#24386,#24387,#24388,#24389,#24390,#24391),
 .UNSPECIFIED.,.F.,.F.,(4,1,1,1,1,1,1,1,1,1,1,1,1,4),(40.8407044966674,
41.0644587758518,41.5635950005423,42.0627312252329,42.5618674499234,43.0610036746139,
43.5601398993044,44.059276123995,44.5584123486855,45.057548573376,45.5566847980665,
46.0558210227571,46.5549572474476,46.8727891676101),.UNSPECIFIED.);
#320=B_SPLINE_CURVE_WITH_KNOTS('',3,(#24396,#24397,#24398,#24399,#24400,
#24401,#24402,#24403,#24404,#24405,#24406,#24407,#24408,#24409,#24410,#24411,
#24412,#24413,#24414,#24415,#24416,#24417,#24418,#24419,#24420,#24421,#24422,
#24423,#24424,#24425,#24426,#24427,#24428,#24429,#24430,#24431,#24432,#24433,
#24434,#24435,#24436,#24437,#24438,#24439,#24440,#24441,#24442,#24443,#24444,
#24445,#24446,#24447,#24448,#24449,#24450,#24451,#24452,#24453,#24454,#24455,
#24456,#24457,#24458,#24459,#24460,#24461,#24462,#24463,#24464,#24465,#24466,
#24467,#24468,#24469,#24470,#24471,#24472,#24473,#24474,#24475,#24476,#24477,
#24478,#24479,#24480,#24481,#24482,#24483,#24484,#24485,#24486,#24487,#24488,
#24489,#24490,#24491,#24492,#24493,#24494,#24495,#24496,#24497,#24498,#24499,
#24500,#24501,#24502,#24503,#24504,#24505,#24506,#24507,#24508,#24509,#24510,
#24511,#24512,#24513,#24514,#24515,#24516,#24517,#24518,#24519,#24520,#24521,
#24522,#24523,#24524,#24525,#24526,#24527,#24528,#24529,#24530,#24531,#24532,
#24533,#24534,#24535,#24536,#24537,#24538,#24539,#24540,#24541,#24542,#24543,
#24544,#24545,#24546,#24547,#24548,#24549,#24550,#24551,#24552,#24553,#24554,
#24555,#24556,#24557,#24558,#24559,#24560,#24561,#24562,#24563,#24564,#24565,
#24566,#24567,#24568,#24569,#24570,#24571,#24572,#24573,#24574,#24575,#24576,
#24577,#24578,#24579,#24580,#24581,#24582,#24583,#24584,#24585,#24586,#24587,
#24588,#24589,#24590,#24591,#24592,#24593,#24594,#24595,#24596,#24597,#24598,
#24599,#24600,#24601,#24602,#24603,#24604,#24605,#24606,#24607,#24608,#24609,
#24610,#24611,#24612,#24613,#24614,#24615,#24616,#24617,#24618,#24619,#24620,
#24621,#24622,#24623,#24624,#24625,#24626,#24627,#24628,#24629,#24630,#24631),
 .UNSPECIFIED.,.F.,.F.,(4,2,2,2,2,2,2,2,2,2,2,2,2,2,2,2,2,2,2,2,2,2,2,2,
2,2,2,2,2,2,2,2,2,2,2,2,2,2,2,2,2,2,2,2,2,2,2,2,2,2,2,2,2,2,2,2,2,2,2,2,
2,2,2,2,2,2,2,2,2,2,2,2,2,2,2,2,2,2,2,2,2,2,2,2,2,2,2,2,2,2,2,2,2,2,2,2,
2,2,2,2,2,2,2,2,2,2,2,2,2,2,2,2,2,2,2,2,2,4),(-6.06752948703079,-6.01968975532367,
-6.00279863227356,-5.97729076238544,-5.95859254006379,-5.93211083694878,
-5.87908462928733,-5.86132864964779,-5.85029413377576,-5.83937636039134,
-5.82013402624847,-5.76851251713189,-5.74491130681351,-5.7239372297368,
-5.70313148561065,-5.6586090845869,-5.62622511510572,-5.6115827919692,-5.60007748730739,
-5.58937275134007,-5.56524373229554,-5.5199334118267,-5.49518139551221,
-5.47784438500099,-5.45695813998917,-5.39132811303644,-5.37169925714225,
-5.36012517940655,-5.35400373133728,-5.35232377145435,-5.35079672789885,
-5.34878497557384,-5.33107367656639,-5.27763830554734,-5.25380157143114,
-5.23193364477924,-5.21310868128819,-5.17649705092115,-5.12943422451358,
-5.12137438236276,-5.10857205929379,-5.09619280852159,-5.05266151895532,
-5.00666210026908,-4.98511863150322,-4.96609123203312,-4.91902604917745,
-4.88812100560458,-4.86874620249341,-4.85768166922201,-4.84101385605415,
-4.78647590617933,-4.75392004146292,-4.73350912632917,-4.70923085635204,
-4.66820715326864,-4.63003247268438,-4.61714019136484,-4.60650849515677,
-4.58269317571645,-4.53699326847181,-4.50663984395818,-4.48634711077696,
-4.46117139570225,-4.40697730394375,-4.39362156739793,-4.37604107614999,
-4.36499328867072,-4.34626584044617,-4.29465495007958,-4.27076953772001,
-4.24887818118798,-4.23006572420335,-4.19362580542125,-4.13703954012282,
-4.12470293874582,-4.1118506776887,-4.07518075017096,-4.02357217418132,
-4.00201904726829,-3.98299853156462,-3.93568433401717,-3.90491630760021,
-3.8855873371089,-3.87452429095245,-3.85782505255265,-3.80332854344605,
-3.77935842095198,-3.75742632544126,-3.7360950905289,-3.68388020916178,
-3.64540278990727,-3.63309083417994,-3.62020915567856,-3.5571897006089,
-3.53333875106678,-3.51146404787057,-3.4900874894295,-3.43295118585468,
-3.40904269705533,-3.40095407803768,-3.38812210182429,-3.37576849245923,
-3.33182518793383,-3.28720013192981,-3.2654131585503,-3.24654299299434,
-3.20904089299356,-3.16295272135323,-3.15495076570774,-3.14220827216713,
-3.13149424736765,-3.10623092664853,-3.09564974794408,-3.0390892544507,
-3.01782572016804,-2.99580342183124,-2.97193325191145),.UNSPECIFIED.);
#321=B_SPLINE_CURVE_WITH_KNOTS('',3,(#24633,#24634,#24635,#24636,#24637),
 .UNSPECIFIED.,.F.,.F.,(4,1,4),(46.8727891676101,47.0540934721381,47.123889803847),
 .UNSPECIFIED.);
#322=B_SPLINE_CURVE_WITH_KNOTS('',3,(#24638,#24639,#24640,#24641,#24642,
#24643,#24644,#24645,#24646,#24647,#24648,#24649,#24650,#24651,#24652,#24653,
#24654,#24655,#24656,#24657,#24658,#24659,#24660,#24661,#24662,#24663,#24664,
#24665,#24666,#24667,#24668,#24669,#24670,#24671,#24672,#24673,#24674,#24675,
#24676,#24677,#24678,#24679,#24680,#24681,#24682,#24683,#24684,#24685,#24686,
#24687,#24688,#24689,#24690,#24691,#24692,#24693,#24694,#24695,#24696,#24697,
#24698,#24699,#24700,#24701,#24702,#24703,#24704,#24705,#24706,#24707,#24708,
#24709,#24710,#24711,#24712,#24713,#24714,#24715,#24716,#24717,#24718,#24719,
#24720,#24721,#24722,#24723,#24724,#24725,#24726,#24727,#24728,#24729,#24730,
#24731,#24732,#24733,#24734,#24735,#24736,#24737,#24738,#24739,#24740,#24741,
#24742,#24743,#24744,#24745,#24746,#24747,#24748,#24749,#24750,#24751,#24752,
#24753,#24754,#24755,#24756,#24757,#24758,#24759,#24760,#24761,#24762,#24763,
#24764,#24765,#24766,#24767,#24768,#24769,#24770,#24771,#24772,#24773,#24774,
#24775,#24776,#24777,#24778,#24779,#24780,#24781,#24782,#24783,#24784,#24785,
#24786,#24787,#24788,#24789,#24790,#24791,#24792,#24793,#24794,#24795,#24796,
#24797,#24798,#24799,#24800,#24801,#24802,#24803,#24804,#24805,#24806,#24807,
#24808,#24809,#24810,#24811,#24812,#24813,#24814,#24815,#24816,#24817,#24818,
#24819,#24820,#24821,#24822,#24823,#24824,#24825,#24826,#24827,#24828,#24829,
#24830,#24831,#24832,#24833,#24834,#24835,#24836,#24837,#24838,#24839,#24840,
#24841,#24842,#24843,#24844,#24845,#24846,#24847,#24848,#24849,#24850,#24851,
#24852,#24853,#24854,#24855,#24856,#24857,#24858,#24859,#24860,#24861,#24862,
#24863,#24864,#24865,#24866,#24867,#24868,#24869),.UNSPECIFIED.,.F.,.F.,
(4,2,2,2,2,2,2,2,2,2,2,2,2,2,2,2,2,2,2,2,2,2,2,2,2,2,2,2,2,2,2,2,2,2,2,
2,2,2,2,2,2,2,2,2,2,2,2,2,2,2,2,2,2,2,2,2,2,2,2,2,2,2,2,2,2,2,2,2,2,2,2,
2,2,2,2,2,2,2,2,2,2,2,2,2,2,2,2,2,2,2,2,2,2,2,2,2,2,2,2,2,2,2,2,2,2,2,2,
2,2,2,2,2,2,2,2,4),(-6.19118392946141,-6.13037761200805,-6.11093273724125,
-6.0918143257748,-6.06357102546708,-5.991874087076,-5.97971012129886,-5.96703953917199,
-5.92779582267618,-5.8928724473279,-5.86633525347181,-5.86322290707405,
-5.86091746316682,-5.85603361626317,-5.84535111229184,-5.82145515198586,
-5.7674476150873,-5.74952878321101,-5.73564738312852,-5.72397445151794,
-5.70085021757395,-5.65432578088489,-5.63134831756085,-5.61124156573648,
-5.59486940739819,-5.55901387544994,-5.51785286198639,-5.50162610579027,
-5.50035763511655,-5.49926118983562,-5.49829201249427,-5.48748519703164,
-5.47453260639729,-5.43797930406928,-5.40196185482296,-5.38079075388334,
-5.36582059512924,-5.3468344534799,-5.30984233649761,-5.26436766578781,
-5.24687785432739,-5.23570846593294,-5.21624903551618,-5.1661727113296,
-5.14199174210581,-5.11987318286207,-5.10087906665762,-5.06375082924483,
-5.02986046835593,-5.01741715553728,-5.0092649989165,-4.99633703633041,
-4.98380396117748,-4.94170496517013,-4.89685445677497,-4.87453669398018,
-4.85311211493562,-4.79630162960949,-4.77178531149256,-4.76355430223362,
-4.75054537581196,-4.73808164000655,-4.69473053315154,-4.64842648910057,
-4.62672777822736,-4.60475913002213,-4.55819274999848,-4.52892606002085,
-4.5100738298483,-4.49891716120239,-4.48092999692706,-4.42767042470952,
-4.40375960667328,-4.38177014343958,-4.36008996826393,-4.30727939445949,
-4.28111380660068,-4.26340945736504,-4.25224688168972,-4.23306097748823,
-4.18268731754972,-4.1584588601933,-4.13631756339948,-4.11733531626208,
-4.0804063518357,-4.03384296964623,-4.02567586731035,-4.01273252606796,
-4.00021283489043,-3.95786026081262,-3.91064189623736,-3.88895817104347,
-3.86697262073152,-3.82075324475661,-3.77914431751064,-3.76644917332635,
-3.75369557858554,-3.7154780847956,-3.66745014865499,-3.64509673896242,
-3.6236963011979,-3.56723089621119,-3.54244317846208,-3.53415640195549,
-3.5210903814546,-3.51035924399168,-3.45697986918221,-3.42431377682065,
-3.40114743426828,-3.38041190179878,-3.31397990711238,-3.29915428296019,
-3.28043715606588,-3.27035488719525,-3.25408593620953,-3.21935065787348),
 .UNSPECIFIED.);
#323=B_SPLINE_CURVE_WITH_KNOTS('',3,(#24875,#24876,#24877,#24878,#24879,
#24880,#24881,#24882,#24883,#24884,#24885,#24886,#24887,#24888,#24889,#24890,
#24891,#24892,#24893,#24894,#24895,#24896,#24897,#24898,#24899,#24900,#24901,
#24902,#24903,#24904,#24905,#24906,#24907,#24908,#24909,#24910,#24911,#24912,
#24913,#24914,#24915,#24916,#24917,#24918,#24919,#24920,#24921,#24922,#24923,
#24924,#24925,#24926,#24927,#24928,#24929,#24930,#24931,#24932,#24933,#24934,
#24935,#24936,#24937,#24938,#24939,#24940,#24941,#24942,#24943,#24944,#24945,
#24946,#24947,#24948,#24949,#24950,#24951,#24952,#24953,#24954,#24955,#24956,
#24957,#24958,#24959,#24960,#24961,#24962,#24963,#24964,#24965,#24966,#24967,
#24968,#24969,#24970,#24971,#24972,#24973,#24974,#24975,#24976,#24977,#24978,
#24979,#24980,#24981,#24982,#24983,#24984,#24985,#24986,#24987,#24988,#24989,
#24990,#24991,#24992,#24993,#24994,#24995,#24996,#24997,#24998,#24999,#25000,
#25001,#25002,#25003,#25004,#25005,#25006,#25007,#25008,#25009,#25010,#25011,
#25012,#25013,#25014,#25015,#25016,#25017,#25018,#25019,#25020,#25021,#25022,
#25023,#25024,#25025,#25026,#25027,#25028,#25029,#25030,#25031,#25032,#25033,
#25034,#25035,#25036,#25037,#25038,#25039,#25040,#25041,#25042,#25043,#25044,
#25045,#25046,#25047,#25048,#25049,#25050,#25051,#25052,#25053,#25054,#25055,
#25056,#25057,#25058,#25059,#25060,#25061,#25062,#25063,#25064,#25065,#25066,
#25067,#25068,#25069,#25070,#25071,#25072,#25073,#25074,#25075,#25076,#25077,
#25078,#25079,#25080,#25081,#25082,#25083,#25084,#25085,#25086,#25087,#25088,
#25089,#25090,#25091,#25092,#25093,#25094,#25095,#25096,#25097,#25098,#25099,
#25100,#25101,#25102,#25103,#25104,#25105,#25106,#25107,#25108,#25109,#25110,
#25111,#25112,#25113,#25114,#25115,#25116,#25117,#25118,#25119,#25120,#25121,
#25122,#25123,#25124,#25125,#25126,#25127,#25128,#25129,#25130,#25131,#25132,
#25133,#25134,#25135,#25136,#25137,#25138,#25139,#25140,#25141,#25142,#25143,
#25144,#25145,#25146,#25147,#25148,#25149,#25150,#25151,#25152,#25153,#25154,
#25155,#25156,#25157,#25158),.UNSPECIFIED.,.F.,.F.,(4,2,2,2,2,2,2,2,2,2,
2,2,2,2,2,2,2,2,2,2,2,2,2,2,2,2,2,2,2,2,2,2,2,2,2,2,2,2,2,2,2,2,2,2,2,2,
2,2,2,2,2,2,2,2,2,2,2,2,2,2,2,2,2,2,2,2,2,2,2,2,2,2,2,2,2,2,2,2,2,2,2,2,
2,2,2,2,2,2,2,2,2,2,2,2,2,2,2,2,2,2,2,2,2,2,2,2,2,2,2,2,2,2,2,2,2,2,2,2,
2,2,2,2,2,2,2,2,2,2,2,2,2,2,2,2,2,2,2,2,2,2,2,4),(-2.97193608483724,-2.95192887323686,
-2.94012091410521,-2.90939597506129,-2.86047323796893,-2.84964247725588,
-2.8370898122707,-2.7983648378627,-2.75335703660431,-2.73035666552808,-2.70960978611333,
-2.67103173278106,-2.62240165692139,-2.60709516004842,-2.59699068818906,
-2.57663599727033,-2.54265354284125,-2.49989542929081,-2.48091802615095,
-2.45930240684551,-2.44722791131797,-2.38876883161093,-2.36596416851559,
-2.35471288561814,-2.33937239663575,-2.32868938600274,-2.28950399592165,
-2.25190455096406,-2.23141072131705,-2.20837106893445,-2.17581260534265,
-2.12253913486938,-2.11187411227277,-2.09904396385401,-2.09095727041018,
-2.06705795903259,-2.01141884276346,-1.98969977530631,-1.96818876663688,
-1.92161264544932,-1.87858971518575,-1.86617991899995,-1.85341229946849,
-1.84538618615958,-1.79923984675326,-1.76186576808191,-1.74299906076222,
-1.72120576212628,-1.69752412548059,-1.64529768411949,-1.62657703831408,
-1.61552934972242,-1.59794300642241,-1.58457980200152,-1.5303846474279,
-1.50521890933385,-1.48492514159982,-1.45455170860782,-1.40878193496465,
-1.38503664389725,-1.37441247636476,-1.36150561710902,-1.3036436110138,
-1.26798071259805,-1.24759135033079,-1.22422159422923,-1.1972515690798,
-1.1483366310095,-1.13286194451083,-1.12168770151473,-1.1000891057743,-1.06173611117017,
-1.02448714822718,-1.00562548119416,-0.983823363157249,-0.960123367584209,
-0.907756340566979,-0.889155637231191,-0.878265985002877,-0.877800523395954,
-0.877339573478321,-0.87687710719356,-0.876407848295914,-0.875926931138482,
-0.875429662648014,-0.874911343635513,-0.874367124318079,-0.873791878721041,
-0.873180087941176,-0.872960224745066,-0.872699570843726,-0.872388713835824,
-0.872015543849654,-0.871564343823832,-0.871014546561892,-0.870339041284213,
-0.86950188436627,-0.868455248153306,-0.867135439061309,-0.848961851427595,
-0.792155219620062,-0.767687499783322,-0.760127278344985,-0.747378291801462,
-0.727195204507704,-0.6956224038808,-0.653785941992173,-0.639632919810163,
-0.629171961549914,-0.628038955424361,-0.627650531208356,-0.627135655781143,
-0.626434726475891,-0.625451391820586,-0.624026098420751,-0.621891513544238,
-0.618606603424055,-0.59760520556375,-0.534886668924286,-0.515517748846135,
-0.496189359178997,-0.47427068471987,-0.433661336058603,-0.403293736559134,
-0.391100521352264,-0.389622585788981,-0.388725809455814,-0.374088004665795,
-0.346541156696376,-0.288907830836164,-0.270388531947011,-0.260445690242536,
-0.241163694574249,-0.192923662299934,-0.188151847174608,-0.157581533242111,
-0.145362980693881,-0.135452691958635,-0.0774953999897133,-0.040120865432972,
-0.0194272729031921,-4.22450758382579E-5),.UNSPECIFIED.);
#324=B_SPLINE_CURVE_WITH_KNOTS('',3,(#25159,#25160,#25161,#25162,#25163,
#25164,#25165,#25166,#25167,#25168,#25169,#25170),.UNSPECIFIED.,.F.,.F.,
(4,2,2,2,2,4),(-6.19125061960131,-6.11459210477152,-6.10118218427413,-6.09138246653058,
-6.0805744142751,-6.06752948703079),.UNSPECIFIED.);
#325=B_SPLINE_CURVE_WITH_KNOTS('',3,(#25171,#25172,#25173,#25174,#25175,
#25176,#25177,#25178,#25179,#25180,#25181,#25182,#25183,#25184,#25185,#25186,
#25187,#25188,#25189,#25190,#25191,#25192,#25193,#25194,#25195,#25196,#25197,
#25198,#25199,#25200,#25201,#25202,#25203,#25204,#25205,#25206,#25207,#25208,
#25209,#25210,#25211,#25212,#25213,#25214,#25215,#25216,#25217,#25218,#25219,
#25220,#25221,#25222,#25223,#25224,#25225,#25226,#25227,#25228,#25229,#25230,
#25231,#25232,#25233,#25234,#25235,#25236,#25237,#25238,#25239,#25240,#25241,
#25242,#25243,#25244,#25245,#25246,#25247,#25248,#25249,#25250,#25251,#25252,
#25253,#25254,#25255,#25256,#25257,#25258,#25259,#25260,#25261,#25262,#25263,
#25264,#25265,#25266,#25267,#25268,#25269,#25270,#25271,#25272,#25273,#25274,
#25275,#25276,#25277,#25278,#25279,#25280,#25281,#25282,#25283,#25284,#25285,
#25286,#25287,#25288,#25289,#25290,#25291,#25292,#25293,#25294,#25295,#25296,
#25297,#25298,#25299,#25300,#25301,#25302,#25303,#25304,#25305,#25306,#25307,
#25308,#25309,#25310,#25311,#25312,#25313,#25314,#25315,#25316,#25317,#25318,
#25319,#25320,#25321,#25322,#25323,#25324,#25325,#25326,#25327,#25328,#25329,
#25330,#25331,#25332,#25333,#25334,#25335,#25336,#25337,#25338,#25339,#25340,
#25341,#25342,#25343,#25344,#25345,#25346,#25347,#25348,#25349,#25350,#25351,
#25352,#25353,#25354,#25355,#25356,#25357,#25358,#25359,#25360,#25361,#25362,
#25363,#25364,#25365,#25366,#25367,#25368,#25369,#25370,#25371,#25372,#25373,
#25374,#25375,#25376,#25377,#25378,#25379,#25380,#25381,#25382,#25383,#25384,
#25385,#25386,#25387,#25388,#25389,#25390,#25391,#25392,#25393,#25394,#25395,
#25396,#25397,#25398,#25399,#25400,#25401,#25402,#25403,#25404,#25405,#25406,
#25407,#25408),.UNSPECIFIED.,.F.,.F.,(4,2,2,2,2,2,2,2,2,2,2,2,2,2,2,2,2,
2,2,2,2,2,2,2,2,2,2,2,2,2,2,2,2,2,2,2,2,2,2,2,2,2,2,2,2,2,2,2,2,2,2,2,2,
2,2,2,2,2,2,2,2,2,2,2,2,2,2,2,2,2,2,2,2,2,2,2,2,2,2,2,2,2,2,2,2,2,2,2,2,
2,2,2,2,2,2,2,2,2,2,2,2,2,2,2,2,2,2,2,2,2,2,2,2,2,2,2,2,2,4),(-3.21935065787348,
-3.19883993215343,-3.17468046572755,-3.15257215478691,-3.13357248786813,
-3.09564218739132,-3.03911040714761,-3.02834218215764,-3.01534663051692,
-2.93503669739894,-2.91100011453367,-2.89028938197555,-2.85536529536879,
-2.79326096098075,-2.78246612806759,-2.76951952060248,-2.7536920558834,
-2.71502398629461,-2.67793946133549,-2.65894795258787,-2.63682451956624,
-2.61263304134145,-2.5571309527284,-2.54104592183675,-2.53094940153547,
-2.51195313597093,-2.46271554281743,-2.43196737827471,-2.41298554602547,
-2.39084333428992,-2.36661271308228,-2.31420585751401,-2.29625973902099,
-2.28510235990775,-2.26620327200656,-2.23680336056377,-2.19050319584225,
-2.16852192966704,-2.14683423988054,-2.09877524151553,-2.05740984799487,
-2.04483905359599,-2.03195324182503,-2.02384218017162,-1.99990260085111,
-1.94283716841452,-1.92125884073421,-1.89914773078583,-1.87498213319719,
-1.81969249512517,-1.80345275169595,-1.79336832740628,-1.77460794421193,
-1.75972195848574,-1.69345995746482,-1.67271944336393,-1.6495661656083,
-1.61688781155841,-1.56340595922979,-1.5526923073717,-1.53959174384977,
-1.52347634227395,-1.48302696811088,-1.44649984896306,-1.42590469936836,
-1.40231255218522,-1.37503727225636,-1.32617837815377,-1.31066594779575,
-1.30045903902699,-1.27976446586618,-1.24479086077293,-1.20321200726434,
-1.18410449774137,-1.16218302345912,-1.11758202812253,-1.07332603885463,
-1.06091736331595,-1.04784084730578,-1.03954395378982,-1.02674608117364,
-0.968499318443193,-0.944192451583691,-0.923539977830503,-0.889649820455283,
-0.830127757784366,-0.816623310358302,-0.80495799538402,-0.79099201017799,
-0.762046506379547,-0.714844132629646,-0.692907950015024,-0.675121487949285,
-0.670832324905051,-0.666461806578334,-0.64046577079663,-0.59076945943148,
-0.574183141373688,-0.568620726120053,-0.557711346467638,-0.542875572991077,
-0.509730565833909,-0.466117009584465,-0.445164893188363,-0.43147798176649,
-0.397285006004167,-0.34710160658848,-0.329047989813588,-0.326518363962881,
-0.324371516630138,-0.32216218654158,-0.316920419244058,-0.29844487407586,
-0.268191413548545,-0.219692548601389,-0.198837715538191,-0.180423147243701,
-0.129072604151441,-0.123769996527385),.UNSPECIFIED.);
#326=B_SPLINE_CURVE_WITH_KNOTS('',3,(#25413,#25414,#25415,#25416,#25417,
#25418,#25419,#25420,#25421,#25422,#25423,#25424,#25425,#25426,#25427,#25428,
#25429,#25430,#25431,#25432,#25433,#25434,#25435,#25436,#25437,#25438,#25439,
#25440,#25441,#25442,#25443,#25444,#25445,#25446,#25447,#25448,#25449,#25450,
#25451,#25452,#25453,#25454,#25455,#25456,#25457,#25458,#25459,#25460,#25461,
#25462,#25463,#25464,#25465,#25466,#25467,#25468,#25469,#25470,#25471,#25472,
#25473,#25474,#25475,#25476,#25477,#25478,#25479,#25480,#25481,#25482,#25483,
#25484,#25485,#25486,#25487,#25488,#25489,#25490,#25491,#25492,#25493,#25494,
#25495,#25496,#25497,#25498,#25499,#25500,#25501,#25502,#25503,#25504,#25505,
#25506,#25507,#25508,#25509,#25510,#25511,#25512,#25513,#25514,#25515,#25516,
#25517,#25518,#25519,#25520,#25521,#25522,#25523,#25524,#25525,#25526,#25527,
#25528,#25529,#25530,#25531,#25532,#25533,#25534,#25535,#25536,#25537,#25538,
#25539,#25540,#25541,#25542,#25543,#25544,#25545,#25546,#25547,#25548,#25549,
#25550,#25551,#25552,#25553,#25554,#25555,#25556,#25557,#25558,#25559,#25560,
#25561,#25562,#25563,#25564,#25565,#25566,#25567,#25568,#25569,#25570,#25571,
#25572,#25573,#25574,#25575,#25576,#25577,#25578,#25579,#25580,#25581,#25582,
#25583,#25584,#25585,#25586,#25587,#25588,#25589,#25590,#25591,#25592,#25593,
#25594,#25595,#25596,#25597,#25598,#25599,#25600,#25601,#25602,#25603,#25604,
#25605,#25606,#25607,#25608,#25609,#25610,#25611,#25612,#25613,#25614,#25615,
#25616,#25617,#25618,#25619,#25620,#25621,#25622,#25623,#25624,#25625,#25626,
#25627,#25628,#25629,#25630,#25631,#25632,#25633,#25634,#25635,#25636,#25637,
#25638,#25639,#25640,#25641,#25642,#25643,#25644,#25645,#25646,#25647,#25648,
#25649,#25650,#25651,#25652,#25653,#25654,#25655,#25656,#25657,#25658,#25659,
#25660,#25661,#25662,#25663,#25664),.UNSPECIFIED.,.F.,.F.,(4,2,2,2,2,2,
2,2,2,2,2,2,2,2,2,2,2,2,2,2,2,2,2,2,2,2,2,2,2,2,2,2,2,2,2,2,2,2,2,2,2,2,
2,2,2,2,2,2,2,2,2,2,2,2,2,2,2,2,2,2,2,2,2,2,2,2,2,2,2,2,2,2,2,2,2,2,2,2,
2,2,2,2,2,2,2,2,2,2,2,2,2,2,2,2,2,2,2,2,2,2,2,2,2,2,2,2,2,2,2,2,2,2,2,2,
2,2,2,2,2,2,2,2,2,2,2,4),(-6.06751823289617,-6.05216985439356,-6.04103481939818,
-6.02557321717136,-5.97667191387825,-5.94968968410486,-5.93039731693532,
-5.91944651626977,-5.90063830947764,-5.84116683591585,-5.8164919490186,
-5.80194847891225,-5.80106147909734,-5.79959516612697,-5.78736829731487,
-5.75662931646851,-5.71631317697064,-5.69444685649932,-5.67516324903087,
-5.6558514710628,-5.59291939713055,-5.57204497524852,-5.56884284248475,
-5.56676591268161,-5.56538124728371,-5.56442789091796,-5.55347319652719,
-5.54276581966756,-5.51863878038839,-5.47333433612668,-5.4590086239272,
-5.43960189395014,-5.42960245830538,-5.40775855864031,-5.34358675264726,
-5.3245364822329,-5.32305198427973,-5.32188176296775,-5.32095155593872,
-5.32020569217921,-5.3196024497203,-5.30759664293841,-5.29511853294368,
-5.2483675487801,-5.20603207764642,-5.18444778657414,-5.16544951498595,
-5.12818006932293,-5.08231423978833,-5.06590499029098,-5.0547968335007,
-5.03438207189384,-4.98405378648087,-4.96062675124528,-4.93895534777799,
-4.92001489661793,-4.88115097955362,-4.83958434917752,-4.821417591176,-4.81037548631603,
-4.79228128067626,-4.74218267710513,-4.72597268310792,-4.71404289800843,
-4.6925572783407,-4.67348748930582,-4.62019019659991,-4.58342395693775,
-4.57054122681807,-4.55823019031933,-4.52221913441196,-4.49450549413032,
-4.4703950265217,-4.4483953197237,-4.42711520985584,-4.37043780926428,-4.3373277814431,
-4.32457302525111,-4.31215184207256,-4.26933239663672,-4.22249370042298,
-4.20100430556186,-4.17926155933519,-4.12921099743551,-4.09039684130619,
-4.07808218236373,-4.06520371641284,-4.02872858719653,-3.97698848959201,
-3.95543577231078,-3.93641507025487,-3.88910970172197,-3.85833701207767,
-3.83900650592549,-3.82794344240008,-3.81124535387285,-3.77522116985027,
-3.73085601460143,-3.70938320584275,-3.69030354853046,-3.64562300336844,
-3.61333548988716,-3.60368651433719,-3.58930543073169,-3.57795425894659,
-3.55616676277755,-3.4977325755875,-3.485666969139,-3.46405934236577,-3.44507670393331,
-3.3763885214348,-3.3502333740173,-3.33875764952293,-3.32431075568772,-3.26557124610015,
-3.24146005785084,-3.21946002542466,-3.19818023406349,-3.14150432593376,
-3.10839224131371,-3.09563728477073,-3.08321632980159,-3.0405853613927,
-2.99518020863916,-2.97330607703263,-2.97193608483724),.UNSPECIFIED.);
#327=B_SPLINE_CURVE_WITH_KNOTS('',3,(#25666,#25667,#25668,#25669,#25670,
#25671,#25672,#25673,#25674,#25675,#25676,#25677),.UNSPECIFIED.,.F.,.F.,
(4,2,2,2,2,4),(-0.123769996527385,-0.0905127513457727,-0.0777901832579179,
-0.0678980718455824,-0.0543312819426131,-7.62333445612098E-5),
 .UNSPECIFIED.);
#328=B_SPLINE_CURVE_WITH_KNOTS('',3,(#25678,#25679,#25680,#25681,#25682,
#25683,#25684,#25685,#25686,#25687,#25688,#25689,#25690,#25691,#25692,#25693,
#25694,#25695,#25696,#25697,#25698,#25699,#25700,#25701,#25702,#25703,#25704,
#25705,#25706,#25707,#25708,#25709,#25710,#25711,#25712,#25713,#25714,#25715,
#25716,#25717,#25718,#25719,#25720,#25721,#25722,#25723,#25724,#25725,#25726,
#25727,#25728,#25729,#25730,#25731,#25732,#25733,#25734,#25735,#25736,#25737,
#25738,#25739,#25740,#25741,#25742,#25743,#25744,#25745,#25746,#25747,#25748,
#25749,#25750,#25751,#25752,#25753,#25754,#25755,#25756,#25757,#25758,#25759,
#25760,#25761,#25762,#25763,#25764,#25765,#25766,#25767,#25768,#25769,#25770,
#25771,#25772,#25773,#25774,#25775,#25776,#25777,#25778,#25779,#25780,#25781,
#25782,#25783,#25784,#25785,#25786,#25787,#25788,#25789,#25790,#25791,#25792,
#25793,#25794,#25795,#25796,#25797,#25798,#25799,#25800,#25801,#25802,#25803,
#25804,#25805,#25806,#25807,#25808,#25809,#25810,#25811,#25812,#25813,#25814,
#25815,#25816,#25817,#25818,#25819,#25820,#25821,#25822,#25823,#25824,#25825,
#25826,#25827,#25828,#25829,#25830,#25831,#25832,#25833,#25834,#25835,#25836,
#25837,#25838,#25839,#25840,#25841,#25842,#25843,#25844,#25845,#25846,#25847,
#25848,#25849,#25850,#25851,#25852,#25853,#25854,#25855,#25856,#25857,#25858,
#25859,#25860,#25861,#25862,#25863,#25864,#25865,#25866,#25867,#25868,#25869,
#25870,#25871,#25872,#25873,#25874,#25875,#25876,#25877,#25878,#25879,#25880,
#25881,#25882,#25883,#25884,#25885,#25886,#25887,#25888,#25889,#25890,#25891,
#25892,#25893,#25894,#25895,#25896,#25897,#25898,#25899,#25900,#25901,#25902,
#25903,#25904,#25905,#25906,#25907,#25908,#25909,#25910,#25911,#25912,#25913,
#25914,#25915,#25916,#25917,#25918,#25919,#25920,#25921,#25922,#25923,#25924,
#25925,#25926,#25927),.UNSPECIFIED.,.F.,.F.,(4,2,2,2,2,2,2,2,2,2,2,2,2,
2,2,2,2,2,2,2,2,2,2,2,2,2,2,2,2,2,2,2,2,2,2,2,2,2,2,2,2,2,2,2,2,2,2,2,2,
2,2,2,2,2,2,2,2,2,2,2,2,2,2,2,2,2,2,2,2,2,2,2,2,2,2,2,2,2,2,2,2,2,2,2,2,
2,2,2,2,2,2,2,2,2,2,2,2,2,2,2,2,2,2,2,2,2,2,2,2,2,2,2,2,2,2,2,2,2,2,2,2,
2,2,2,4),(-6.19126743548388,-6.16828474090662,-6.14963669721633,-6.12911626038459,
-6.09407045290797,-6.04469600614485,-6.02998196054132,-6.02386121116435,
-6.01159825099855,-5.95368397556366,-5.92710415616773,-5.90421029149716,
-5.90021607519006,-5.87841716429693,-5.82000325402683,-5.79737342519182,
-5.79267308287125,-5.78858396591072,-5.77677067690243,-5.763794382649,-5.72740605585022,
-5.69132633743218,-5.67014275657265,-5.65171719209081,-5.63454244806347,
-5.56796826879926,-5.54857202038289,-5.54709494978456,-5.54617504089132,
-5.54559020305959,-5.54419373615834,-5.54299794275277,-5.54195158343031,
-5.54101409538384,-5.54015203704611,-5.52924140760204,-5.51501686712426,
-5.45662020770856,-5.43203024657978,-5.41175884842804,-5.39118243177943,
-5.38957350127555,-5.35033717751618,-5.31363618012526,-5.2981433826564,
-5.28537722947894,-5.27269374992325,-5.23997200558627,-5.19165610213958,
-5.16761046779675,-5.14690102368562,-5.11310367121344,-5.07006809097023,
-5.05355856087118,-5.04024936256002,-5.0296336672651,-5.00647453346544,
-4.95036148269244,-4.93817769851656,-4.9163708986313,-4.89718777425577,
-4.86434940364664,-4.82343290460124,-4.80724377807857,-4.79410406073478,
-4.78174469382991,-4.74930740421553,-4.71774629642357,-4.69356256449648,
-4.6714423341025,-4.65244808474731,-4.61052461602099,-4.57196623791136,
-4.55331944261558,-4.54216457790801,-4.52398933596185,-4.47227732687522,
-4.44793903421221,-4.42574481020861,-4.40423002831425,-4.37061406694095,
-4.33110700122942,-4.3091582311323,-4.2978727563582,-4.28217170822759,-4.23302884429366,
-4.20615261685623,-4.18274749012401,-4.16209459124178,-4.12452332339496,
-4.08514945436609,-4.06323528165216,-4.05195189836505,-4.03623646868448,
-3.98708296269589,-3.96022269422368,-3.93682514102816,-3.91616993218671,
-3.8799125896541,-3.83959194282026,-3.82349638939828,-3.81040649619156,
-3.79800829724502,-3.76547446920891,-3.71726030650093,-3.69283088232667,
-3.67220171957627,-3.63872775754081,-3.59488424748989,-3.57825732565668,
-3.56488643363806,-3.55269358153526,-3.51528834266287,-3.48796576787696,
-3.46386705117982,-3.44178754238168,-3.42277161251931,-3.38511406908166,
-3.33893450363513,-3.33092372657556,-3.31814148682508,-3.30725003571265,
-3.25782453257591,-3.227198544306,-3.21940568334086),.UNSPECIFIED.);
#329=B_SPLINE_CURVE_WITH_KNOTS('',3,(#25933,#25934,#25935,#25936,#25937,
#25938,#25939,#25940,#25941,#25942,#25943,#25944,#25945,#25946,#25947,#25948,
#25949,#25950,#25951,#25952,#25953,#25954,#25955,#25956,#25957,#25958,#25959,
#25960,#25961,#25962,#25963,#25964,#25965,#25966,#25967,#25968,#25969,#25970,
#25971,#25972,#25973,#25974,#25975,#25976,#25977,#25978,#25979,#25980,#25981,
#25982,#25983,#25984,#25985,#25986,#25987,#25988,#25989,#25990,#25991,#25992,
#25993,#25994,#25995,#25996,#25997,#25998,#25999,#26000,#26001,#26002,#26003,
#26004,#26005,#26006,#26007,#26008,#26009,#26010,#26011,#26012,#26013,#26014,
#26015,#26016,#26017,#26018,#26019,#26020,#26021,#26022,#26023,#26024,#26025,
#26026,#26027,#26028,#26029,#26030,#26031,#26032,#26033,#26034,#26035,#26036,
#26037,#26038,#26039,#26040,#26041,#26042,#26043,#26044,#26045,#26046,#26047,
#26048,#26049,#26050,#26051,#26052,#26053,#26054,#26055,#26056,#26057,#26058,
#26059,#26060,#26061,#26062,#26063,#26064,#26065,#26066,#26067,#26068,#26069,
#26070,#26071,#26072,#26073,#26074,#26075,#26076,#26077,#26078,#26079,#26080,
#26081,#26082,#26083,#26084,#26085,#26086,#26087,#26088,#26089,#26090,#26091,
#26092,#26093,#26094,#26095,#26096,#26097,#26098,#26099,#26100,#26101,#26102,
#26103,#26104,#26105,#26106,#26107,#26108,#26109,#26110,#26111,#26112,#26113,
#26114,#26115,#26116,#26117,#26118,#26119,#26120,#26121,#26122,#26123,#26124,
#26125,#26126,#26127,#26128,#26129,#26130,#26131,#26132,#26133,#26134,#26135,
#26136,#26137,#26138,#26139,#26140,#26141,#26142,#26143,#26144,#26145,#26146,
#26147,#26148,#26149,#26150,#26151,#26152,#26153,#26154,#26155,#26156),
 .UNSPECIFIED.,.F.,.F.,(4,2,2,2,2,2,2,2,2,2,2,2,2,2,2,2,2,2,2,2,2,2,2,2,
2,2,2,2,2,2,2,2,2,2,2,2,2,2,2,2,2,2,2,2,2,2,2,2,2,2,2,2,2,2,2,2,2,2,2,2,
2,2,2,2,2,2,2,2,2,2,2,2,2,2,2,2,2,2,2,2,2,2,2,2,2,2,2,2,2,2,2,2,2,2,2,2,
2,2,2,2,2,2,2,2,2,2,2,2,2,2,2,4),(-2.97194085139843,-2.94720454401188,-2.92566231016735,
-2.90397702385757,-2.86051929887029,-2.82465054145874,-2.80787106414141,
-2.79681155251526,-2.7775973373761,-2.74716968982091,-2.69923207646114,
-2.68023021012824,-2.65865057730204,-2.64661598158126,-2.58979555400551,
-2.56692485617133,-2.5564119937776,-2.54327419413601,-2.5270360980217,-2.48549429734368,
-2.4501651762219,-2.429592601371,-2.40605095797732,-2.36037576064841,-2.32250927335493,
-2.31162328725177,-2.29915169432355,-2.29141098067681,-2.24597551189013,
-2.21611003985732,-2.19281752224885,-2.17217174544167,-2.13554071754574,
-2.0861573261149,-2.07001213803844,-2.06003746159135,-2.04174443590058,
-2.02744768186526,-1.95977683493294,-1.93924675203804,-1.91630760462578,
-1.86901146007682,-1.83078791279796,-1.81994514128857,-1.80741050635883,
-1.79960887728262,-1.78796090745952,-1.74095528196348,-1.71016066593002,
-1.68984610606951,-1.66488083338587,-1.63440217472169,-1.58500446603003,
-1.57416275046488,-1.56162647157065,-1.52366524158169,-1.47187743755666,
-1.45047394030724,-1.42863155009465,-1.40484773404046,-1.35183276020116,
-1.33377485674184,-1.32273254318616,-1.30452844940075,-1.26303606644378,
-1.22415961713766,-1.20521982789832,-1.18354678337682,-1.1399823029505,
-1.10471572555404,-1.08762624998673,-1.07657703856195,-1.05777790033058,
-1.01581243229156,-0.978129648870317,-0.959230991313171,-0.937491640597036,
-0.893420452873878,-0.84855216661018,-0.836259127369291,-0.827241481570068,
-0.814007125752753,-0.788054562102724,-0.734781189971937,-0.713689333105909,
-0.695987873343957,-0.673847854430633,-0.63384205353527,-0.602616315005399,
-0.590379232392695,-0.57848395128835,-0.56335215670829,-0.528407931174318,
-0.48918639969776,-0.468054608601724,-0.446837684251083,-0.383704569944666,
-0.355887136398819,-0.345104699599106,-0.336392856808139,-0.32355232068174,
-0.299200230067635,-0.242460285456655,-0.221530628746799,-0.210680784737342,
-0.184716624213847,-0.148210722704724,-0.110535353186893,-0.0984733264317177,
-0.088502788824408,-0.0744376508116578,-4.22937978884163E-5),
 .UNSPECIFIED.);
#330=B_SPLINE_CURVE_WITH_KNOTS('',3,(#26157,#26158,#26159,#26160,#26161,
#26162,#26163,#26164,#26165,#26166,#26167,#26168),.UNSPECIFIED.,.F.,.F.,
(4,2,2,2,2,4),(-6.19124774226682,-6.17979920712744,-6.16889498083572,-6.14808214462905,
-6.07247948514389,-6.06751823289617),.UNSPECIFIED.);
#331=B_SPLINE_CURVE_WITH_KNOTS('',3,(#26169,#26170,#26171,#26172,#26173,
#26174,#26175,#26176,#26177,#26178,#26179,#26180,#26181,#26182,#26183,#26184,
#26185,#26186,#26187,#26188,#26189,#26190,#26191,#26192,#26193,#26194,#26195,
#26196,#26197,#26198,#26199,#26200,#26201,#26202,#26203,#26204,#26205,#26206,
#26207,#26208,#26209,#26210,#26211,#26212,#26213,#26214,#26215,#26216,#26217,
#26218,#26219,#26220,#26221,#26222,#26223,#26224,#26225,#26226,#26227,#26228,
#26229,#26230,#26231,#26232,#26233,#26234,#26235,#26236,#26237,#26238,#26239,
#26240,#26241,#26242,#26243,#26244,#26245,#26246,#26247,#26248,#26249,#26250,
#26251,#26252,#26253,#26254,#26255,#26256,#26257,#26258,#26259,#26260,#26261,
#26262,#26263,#26264,#26265,#26266,#26267,#26268,#26269,#26270,#26271,#26272,
#26273,#26274,#26275,#26276,#26277,#26278,#26279,#26280,#26281,#26282,#26283,
#26284,#26285,#26286,#26287,#26288,#26289,#26290,#26291,#26292,#26293,#26294,
#26295,#26296,#26297,#26298,#26299,#26300,#26301,#26302,#26303,#26304,#26305,
#26306,#26307,#26308,#26309,#26310,#26311,#26312,#26313,#26314,#26315,#26316,
#26317,#26318,#26319,#26320,#26321,#26322,#26323,#26324,#26325,#26326,#26327,
#26328,#26329,#26330,#26331,#26332,#26333,#26334,#26335,#26336,#26337,#26338,
#26339,#26340,#26341,#26342,#26343,#26344,#26345,#26346,#26347,#26348,#26349,
#26350,#26351,#26352,#26353,#26354,#26355,#26356,#26357,#26358,#26359,#26360,
#26361,#26362,#26363,#26364,#26365,#26366,#26367,#26368,#26369,#26370,#26371,
#26372,#26373,#26374,#26375,#26376,#26377,#26378,#26379,#26380,#26381,#26382,
#26383,#26384,#26385,#26386,#26387,#26388,#26389,#26390,#26391,#26392,#26393,
#26394,#26395,#26396,#26397,#26398,#26399,#26400,#26401,#26402),
 .UNSPECIFIED.,.F.,.F.,(4,2,2,2,2,2,2,2,2,2,2,2,2,2,2,2,2,2,2,2,2,2,2,2,
2,2,2,2,2,2,2,2,2,2,2,2,2,2,2,2,2,2,2,2,2,2,2,2,2,2,2,2,2,2,2,2,2,2,2,2,
2,2,2,2,2,2,2,2,2,2,2,2,2,2,2,2,2,2,2,2,2,2,2,2,2,2,2,2,2,2,2,2,2,2,2,2,
2,2,2,2,2,2,2,2,2,2,2,2,2,2,2,2,2,2,2,2,4),(-3.21940568334086,-3.21537518281795,
-3.19388774193548,-3.17165692436193,-3.12302283788408,-3.09569644682846,
-3.07754890742245,-3.0663938538005,-3.04771748855768,-3.03294881751308,
-2.96636327134014,-2.94563227095093,-2.9224521615715,-2.88981276131488,
-2.83646498215127,-2.82572714784475,-2.81267331782483,-2.77725580497548,
-2.72441739094326,-2.70274064263488,-2.68074610034784,-2.65682487107412,
-2.60349271392291,-2.58556032236083,-2.57440246759245,-2.55548681158526,
-2.52604015184907,-2.47982883707528,-2.45784279271721,-2.43615845527834,
-2.42411163874887,-2.37240571003688,-2.34551192307258,-2.33452652564069,
-2.32188896753746,-2.2822927869588,-2.23329088089453,-2.21145448751781,
-2.18962991914374,-2.17742623062078,-2.12169781414149,-2.09834709892359,
-2.08770600008823,-2.07445341813518,-2.05805153802712,-2.01573901141806,
-1.98093861853728,-1.96023434351834,-1.93616654182965,-1.88785460325268,
-1.8551250464599,-1.84246469577492,-1.82967460853503,-1.79675708291012,
-1.74011555734052,-1.71857923434076,-1.69641361277398,-1.67213458252677,
-1.62079143998806,-1.60228743225512,-1.59113339355084,-1.57282210582547,
-1.52459732453246,-1.48971601185184,-1.46893898393931,-1.44516035009689,
-1.36908148091808,-1.35380556144267,-1.34238444613811,-1.31829372119246,
-1.27994683956392,-1.24705192910284,-1.22786357015394,-1.20606381835904,
-1.19388794222435,-1.1373428992037,-1.11442862701847,-1.10384670406367,
-1.09045852983862,-1.07379911084305,-1.02972730707585,-0.996447331222667,
-0.975828834285558,-0.951338733694337,-0.903134242177257,-0.870665632373246,
-0.858295198757108,-0.848295578259484,-0.834311223982213,-0.805282885672852,
-0.758244952392974,-0.736665546557421,-0.717480796217459,-0.69539793510178,
-0.654411094506414,-0.624539223894218,-0.61224561467836,-0.602218042126419,
-0.588128117322131,-0.558615882604407,-0.512531037488587,-0.490904180488482,
-0.471707812870348,-0.44967731277801,-0.40899133647246,-0.378573842295565,
-0.366300615793601,-0.356265328841865,-0.34214640007698,-0.312499905836464,
-0.266673952521797,-0.245035028836767,-0.225835694027473,-0.203818362017452,
-0.163207496702661,-0.132704799728157,-0.12380451714121),.UNSPECIFIED.);
#332=B_SPLINE_CURVE_WITH_KNOTS('',3,(#26407,#26408,#26409,#26410,#26411,
#26412,#26413,#26414,#26415,#26416,#26417,#26418,#26419,#26420,#26421,#26422,
#26423,#26424,#26425,#26426,#26427,#26428,#26429,#26430,#26431,#26432,#26433,
#26434,#26435,#26436,#26437,#26438,#26439,#26440,#26441,#26442,#26443,#26444,
#26445,#26446,#26447,#26448,#26449,#26450,#26451,#26452,#26453,#26454,#26455,
#26456,#26457,#26458,#26459,#26460,#26461,#26462,#26463,#26464,#26465,#26466,
#26467,#26468,#26469,#26470,#26471,#26472,#26473,#26474,#26475,#26476,#26477,
#26478,#26479,#26480,#26481,#26482,#26483,#26484,#26485,#26486,#26487,#26488,
#26489,#26490,#26491,#26492,#26493,#26494,#26495,#26496,#26497,#26498,#26499,
#26500,#26501,#26502,#26503,#26504,#26505,#26506,#26507,#26508,#26509,#26510,
#26511,#26512,#26513,#26514,#26515,#26516,#26517,#26518,#26519,#26520,#26521,
#26522,#26523,#26524,#26525,#26526,#26527,#26528,#26529,#26530,#26531,#26532,
#26533,#26534,#26535,#26536,#26537,#26538,#26539,#26540,#26541,#26542,#26543,
#26544,#26545,#26546,#26547,#26548,#26549,#26550,#26551,#26552,#26553,#26554,
#26555,#26556,#26557,#26558,#26559,#26560,#26561,#26562,#26563,#26564,#26565,
#26566,#26567,#26568,#26569,#26570,#26571,#26572,#26573,#26574,#26575,#26576,
#26577,#26578,#26579,#26580,#26581,#26582,#26583,#26584,#26585,#26586,#26587,
#26588,#26589,#26590,#26591,#26592,#26593,#26594,#26595,#26596,#26597,#26598,
#26599,#26600,#26601,#26602,#26603,#26604,#26605,#26606,#26607,#26608,#26609,
#26610,#26611,#26612,#26613,#26614,#26615,#26616,#26617,#26618,#26619,#26620,
#26621,#26622,#26623,#26624,#26625,#26626,#26627,#26628,#26629,#26630,#26631,
#26632,#26633,#26634,#26635,#26636,#26637,#26638,#26639,#26640,#26641,#26642,
#26643,#26644,#26645,#26646,#26647,#26648,#26649,#26650,#26651,#26652,#26653,
#26654,#26655,#26656,#26657,#26658),.UNSPECIFIED.,.F.,.F.,(4,2,2,2,2,2,
2,2,2,2,2,2,2,2,2,2,2,2,2,2,2,2,2,2,2,2,2,2,2,2,2,2,2,2,2,2,2,2,2,2,2,2,
2,2,2,2,2,2,2,2,2,2,2,2,2,2,2,2,2,2,2,2,2,2,2,2,2,2,2,2,2,2,2,2,2,2,2,2,
2,2,2,2,2,2,2,2,2,2,2,2,2,2,2,2,2,2,2,2,2,2,2,2,2,2,2,2,2,2,2,2,2,2,2,2,
2,2,2,2,2,2,2,2,2,2,2,4),(-6.06757918107776,-6.0425092840288,-6.01913297277231,
-6.00269541027639,-6.00150315298628,-5.9998313797898,-5.99763976448805,
-5.98465418449314,-5.9406681252557,-5.9088475850095,-5.8836036632628,-5.8810292257421,
-5.87923008645437,-5.87722136327289,-5.8742110451739,-5.86788716148614,
-5.84269595422236,-5.78665680273765,-5.76856503940206,-5.76500447727211,
-5.75283216642732,-5.74047817198498,-5.67918711101816,-5.65423562140544,
-5.6325240517583,-5.61715766711512,-5.58736987975874,-5.53897062659706,
-5.52177496444567,-5.5204609047147,-5.51935035276981,-5.50794793173914,
-5.50029649178016,-5.48077251674079,-5.42946812382137,-5.39793361855681,
-5.37797793281941,-5.35385127240683,-5.29558425720612,-5.28281203245124,
-5.27454271554864,-5.26152521450837,-5.25095638266374,-5.22767217437242,
-5.17427351781813,-5.14749367538006,-5.1272835884852,-5.09937774256489,
-5.06054431887117,-5.03650023810903,-5.02838323144583,-5.01552196856433,
-5.0048737315627,-4.98073387911697,-4.93529157456466,-4.92094640247116,
-4.89725205134467,-4.87671895644528,-4.84207563224789,-4.79977336674278,
-4.78341996674339,-4.770221271667,-4.75973499494835,-4.73705191893717,-4.68034176094925,
-4.66822463102999,-4.64657038874826,-4.62761834863283,-4.58794163748908,
-4.54293239717864,-4.53536231103792,-4.52306537548176,-4.51016510867539,
-4.47384643051742,-4.42200101559401,-4.4004483927239,-4.38142732226523,
-4.32275420088346,-4.28831320715352,-4.27643508322084,-4.26291901857581,
-4.20361235139557,-4.16988039991287,-4.14940084427622,-4.12547595072461,
-4.04538047260695,-4.03244839446304,-4.02183700689893,-3.99820596617183,
-3.94248514280315,-3.91696301581566,-3.89669919714872,-3.86699525065758,
-3.81847538714104,-3.79451216933769,-3.78318289032979,-3.76821010785203,
-3.71108531348086,-3.67794447119182,-3.6574994466546,-3.63340544408877,
-3.59185012370537,-3.55200549463713,-3.53976894458819,-3.52679307883785,
-3.48199018969532,-3.45056451401728,-3.43861234632596,-3.41710658863934,
-3.39538173783905,-3.34707275653335,-3.31877978936851,-3.3003136537619,
-3.28926962034477,-3.27145927913169,-3.21923671067992,-3.1950365723045,
-3.17299358771688,-3.15174471974862,-3.09562857937333,-3.09013019814411,
-3.06039538616283,-3.04817502755174,-3.0351783347152,-2.99976503962884,
-2.97194085139843),.UNSPECIFIED.);
#333=B_SPLINE_CURVE_WITH_KNOTS('',3,(#26660,#26661,#26662,#26663,#26664,
#26665,#26666,#26667,#26668,#26669,#26670,#26671),.UNSPECIFIED.,.F.,.F.,
(4,2,2,2,2,4),(-0.12380451714121,-0.120419049820546,-0.110388596683704,
-0.0962877087444727,-0.0203605578094701,-8.03739326426108E-5),
 .UNSPECIFIED.);
#334=B_SPLINE_CURVE_WITH_KNOTS('',3,(#26672,#26673,#26674,#26675,#26676,
#26677,#26678,#26679,#26680,#26681,#26682,#26683,#26684,#26685,#26686,#26687,
#26688,#26689,#26690,#26691,#26692,#26693,#26694,#26695,#26696,#26697,#26698,
#26699,#26700,#26701,#26702,#26703,#26704,#26705,#26706,#26707,#26708,#26709,
#26710,#26711,#26712,#26713,#26714,#26715,#26716,#26717,#26718,#26719,#26720,
#26721,#26722,#26723,#26724,#26725,#26726,#26727,#26728,#26729,#26730,#26731,
#26732,#26733,#26734,#26735,#26736,#26737,#26738,#26739,#26740,#26741,#26742,
#26743,#26744,#26745,#26746,#26747,#26748,#26749,#26750,#26751,#26752,#26753,
#26754,#26755,#26756,#26757,#26758,#26759,#26760,#26761,#26762,#26763,#26764,
#26765,#26766,#26767,#26768,#26769,#26770,#26771,#26772,#26773,#26774,#26775,
#26776,#26777,#26778,#26779,#26780,#26781,#26782,#26783,#26784,#26785,#26786,
#26787,#26788,#26789,#26790,#26791,#26792,#26793,#26794,#26795,#26796,#26797,
#26798,#26799,#26800,#26801,#26802,#26803,#26804,#26805,#26806,#26807,#26808,
#26809,#26810,#26811,#26812,#26813,#26814,#26815,#26816,#26817,#26818,#26819,
#26820,#26821,#26822,#26823,#26824,#26825,#26826,#26827,#26828,#26829,#26830,
#26831,#26832,#26833,#26834,#26835,#26836,#26837,#26838,#26839,#26840,#26841,
#26842,#26843,#26844,#26845,#26846,#26847,#26848,#26849,#26850,#26851,#26852,
#26853,#26854,#26855,#26856,#26857,#26858,#26859,#26860,#26861,#26862,#26863,
#26864,#26865,#26866,#26867,#26868,#26869,#26870,#26871,#26872,#26873,#26874,
#26875,#26876,#26877,#26878,#26879,#26880,#26881,#26882,#26883,#26884,#26885,
#26886,#26887,#26888,#26889,#26890,#26891,#26892,#26893,#26894,#26895,#26896,
#26897,#26898,#26899,#26900,#26901),.UNSPECIFIED.,.F.,.F.,(4,2,2,2,2,2,
2,2,2,2,2,2,2,2,2,2,2,2,2,2,2,2,2,2,2,2,2,2,2,2,2,2,2,2,2,2,2,2,2,2,2,2,
2,2,2,2,2,2,2,2,2,2,2,2,2,2,2,2,2,2,2,2,2,2,2,2,2,2,2,2,2,2,2,2,2,2,2,2,
2,2,2,2,2,2,2,2,2,2,2,2,2,2,2,2,2,2,2,2,2,2,2,2,2,2,2,2,2,2,2,2,2,2,2,2,
4),(-6.19122556259034,-6.18004740270646,-6.16748591998267,-6.09113194607832,
-6.07706836346535,-6.06704779425147,-6.05473520553522,-6.02501903578712,
-5.98397307877302,-5.96188042653447,-5.94269819912774,-5.92110448534014,
-5.87399109860499,-5.84499751355316,-5.83102063291017,-5.8210229763796,
-5.80864667274274,-5.77935919896759,-5.73815902250305,-5.71603969695784,
-5.69686303505453,-5.67529397400228,-5.6277335336895,-5.59896071793734,
-5.58503255073024,-5.57504767079496,-5.56431860329828,-5.54017043434067,
-5.49464051115725,-5.4718140082508,-5.45273490810619,-5.43180851022003,
-5.37882004361869,-5.35191059712329,-5.33840671596333,-5.32847465982512,
-5.31565405015465,-5.26964061721162,-5.23840972234037,-5.22646140127431,
-5.2048640825141,-5.18277462051979,-5.14845992804416,-5.11124578379915,
-5.09566355949358,-5.08284897101742,-5.0702115402229,-5.01960042980399,
-4.98590509253942,-4.96290430734998,-4.94210216476408,-4.87788392953217,
-4.84684417213855,-4.83501970443291,-4.82098522698032,-4.76229845625624,
-4.73766427614092,-4.71532813422006,-4.69391474227125,-4.63809691043105,
-4.60153542554785,-4.58953062666189,-4.57585291875668,-4.51508742865812,
-4.49090680494819,-4.4687880773086,-4.44979307946989,-4.41265860140473,
-4.37403350522802,-4.35231588542249,-4.34104388667543,-4.32524399167478,
-4.2871529368824,-4.28318436773609,-4.25328416838485,-4.24161278356404,
-4.22025690534415,-4.19783417444567,-4.1500095774358,-4.10985760192419,
-4.09780744778015,-4.0842092232353,-3.99989869582475,-3.97755882727475,
-3.95614885444126,-3.8994693489945,-3.87483294966568,-3.86657717297908,
-3.85354281502676,-3.8410998466868,-3.7973975195042,-3.76451350691437,-3.75223279299253,
-3.73033896190173,-3.71121389745691,-3.67282028174865,-3.63568216311131,
-3.62011333051749,-3.60730609629866,-3.59466237471625,-3.56193199085345,
-3.51362789091799,-3.48954513603817,-3.46884456223314,-3.43518517415531,
-3.3919894801938,-3.37545658835731,-3.36213514293282,-3.34990876266441,
-3.31273786921841,-3.28534066085584,-3.26122171044855,-3.23913259834888,
-3.22012209697371,-3.2192985515723),.UNSPECIFIED.);
#335=B_SPLINE_CURVE_WITH_KNOTS('',3,(#26907,#26908,#26909,#26910,#26911,
#26912,#26913,#26914,#26915,#26916,#26917,#26918,#26919,#26920,#26921,#26922,
#26923,#26924,#26925,#26926,#26927,#26928,#26929,#26930,#26931,#26932,#26933,
#26934,#26935,#26936,#26937,#26938,#26939,#26940,#26941,#26942,#26943,#26944,
#26945,#26946,#26947,#26948,#26949,#26950,#26951,#26952,#26953,#26954,#26955,
#26956,#26957,#26958,#26959,#26960,#26961,#26962,#26963,#26964,#26965,#26966,
#26967,#26968,#26969,#26970,#26971,#26972,#26973,#26974,#26975,#26976,#26977,
#26978,#26979,#26980,#26981,#26982,#26983,#26984,#26985,#26986,#26987,#26988,
#26989,#26990,#26991,#26992,#26993,#26994,#26995,#26996,#26997,#26998,#26999,
#27000,#27001,#27002,#27003,#27004,#27005,#27006,#27007,#27008,#27009,#27010,
#27011,#27012,#27013,#27014,#27015,#27016,#27017,#27018,#27019,#27020,#27021,
#27022,#27023,#27024,#27025,#27026,#27027,#27028,#27029,#27030,#27031,#27032,
#27033,#27034,#27035,#27036,#27037,#27038,#27039,#27040,#27041,#27042,#27043,
#27044,#27045,#27046,#27047,#27048,#27049,#27050,#27051,#27052,#27053,#27054,
#27055,#27056,#27057,#27058,#27059,#27060,#27061,#27062,#27063,#27064,#27065,
#27066,#27067,#27068,#27069,#27070,#27071,#27072,#27073,#27074,#27075,#27076,
#27077,#27078,#27079,#27080,#27081,#27082,#27083,#27084,#27085,#27086,#27087,
#27088,#27089,#27090,#27091,#27092,#27093,#27094,#27095,#27096,#27097,#27098,
#27099,#27100,#27101,#27102,#27103,#27104,#27105,#27106,#27107,#27108,#27109,
#27110,#27111,#27112,#27113,#27114,#27115,#27116,#27117,#27118,#27119,#27120,
#27121,#27122,#27123,#27124,#27125,#27126),.UNSPECIFIED.,.F.,.F.,(4,3,3,
3,3,3,3,3,3,3,3,3,3,3,3,3,3,3,3,3,3,3,3,3,3,3,3,3,3,3,3,3,3,3,3,3,3,3,3,
3,3,3,3,3,3,3,3,3,3,3,3,3,3,3,3,3,3,3,3,3,3,3,3,3,3,3,3,3,3,3,3,3,3,4),
(78.539816339745,78.6328610561734,78.6468657231173,78.7347200961305,78.822556588302,
78.9103961954321,78.9982306507758,79.0860867015266,79.1457376582654,79.2335920312787,
79.3214285234505,79.4092681305805,79.4971025859242,79.5849586366751,79.6446095934135,
79.7324639664267,79.8203004585983,79.9081400657283,79.9959745210719,80.0838305718228,
80.1434815285617,80.231335901575,80.3191723937466,80.4070120008766,80.4948464562203,
80.5827025069712,80.6423534637098,80.730207836723,80.8180443288945,80.9058839360245,
80.9937183913681,81.081574442119,81.1412253988579,81.2290797718712,81.3169162640427,
81.4047558711728,81.4925903265164,81.5804463772674,81.640097334006,81.7279517070193,
81.8157881991909,81.9036278063209,81.9914622616646,82.0793183124155,82.1389692691542,
82.2268236421675,82.3146601343391,82.4024997414692,82.4903341968129,82.5781902475638,
82.6378412043023,82.7256955773155,82.8135320694871,82.901371676617,82.9892061319606,
83.0770621827114,83.1367131394504,83.2245675124637,83.3124040046352,83.4002436117652,
83.4880780671088,83.5759341178598,83.6355850745985,83.7234394476117,83.8112759397833,
83.8991155469133,83.9869500022568,84.0748060530077,84.1344570097467,84.2223107498068,
84.3101568702724,84.3979902799314,84.4858391601252,84.5719056092393),
 .UNSPECIFIED.);
#336=B_SPLINE_CURVE_WITH_KNOTS('',3,(#27127,#27128,#27129,#27130,#27131,
#27132,#27133,#27134,#27135,#27136),.UNSPECIFIED.,.F.,.F.,(4,2,2,2,4),(-6.19130099814293,
-6.14184388955133,-6.1229614278331,-6.1022946734106,-6.06757918107776),
 .UNSPECIFIED.);
#337=B_SPLINE_CURVE_WITH_KNOTS('',3,(#27137,#27138,#27139,#27140,#27141,
#27142,#27143,#27144,#27145,#27146,#27147,#27148,#27149,#27150,#27151,#27152,
#27153,#27154,#27155,#27156,#27157,#27158,#27159,#27160,#27161,#27162,#27163,
#27164,#27165,#27166,#27167,#27168,#27169,#27170,#27171,#27172,#27173,#27174,
#27175,#27176,#27177,#27178,#27179,#27180,#27181,#27182,#27183,#27184,#27185,
#27186,#27187,#27188,#27189,#27190,#27191,#27192,#27193,#27194,#27195,#27196,
#27197,#27198,#27199,#27200,#27201,#27202,#27203,#27204,#27205,#27206,#27207,
#27208,#27209,#27210,#27211,#27212,#27213,#27214,#27215,#27216,#27217,#27218,
#27219,#27220,#27221,#27222,#27223,#27224,#27225,#27226,#27227,#27228,#27229,
#27230,#27231,#27232,#27233,#27234,#27235,#27236,#27237,#27238,#27239,#27240,
#27241,#27242,#27243,#27244,#27245,#27246,#27247,#27248,#27249,#27250,#27251,
#27252,#27253,#27254,#27255,#27256,#27257,#27258,#27259,#27260,#27261,#27262,
#27263,#27264,#27265,#27266,#27267,#27268,#27269,#27270,#27271,#27272,#27273,
#27274,#27275,#27276,#27277,#27278,#27279,#27280,#27281,#27282,#27283,#27284,
#27285,#27286,#27287,#27288,#27289,#27290,#27291,#27292,#27293,#27294,#27295,
#27296,#27297,#27298,#27299,#27300,#27301,#27302,#27303,#27304,#27305,#27306,
#27307,#27308,#27309,#27310,#27311,#27312,#27313,#27314,#27315,#27316,#27317,
#27318,#27319,#27320,#27321,#27322,#27323,#27324,#27325,#27326,#27327,#27328,
#27329,#27330,#27331,#27332,#27333,#27334,#27335,#27336,#27337,#27338,#27339,
#27340,#27341,#27342,#27343,#27344,#27345,#27346,#27347,#27348,#27349,#27350,
#27351,#27352,#27353,#27354,#27355,#27356,#27357,#27358,#27359,#27360,#27361,
#27362,#27363,#27364,#27365,#27366,#27367,#27368,#27369,#27370,#27371,#27372,
#27373,#27374,#27375,#27376,#27377,#27378,#27379,#27380,#27381,#27382,#27383,
#27384,#27385,#27386,#27387,#27388,#27389,#27390,#27391,#27392,#27393,#27394,
#27395,#27396,#27397,#27398,#27399,#27400),.UNSPECIFIED.,.F.,.F.,(4,2,2,
2,2,2,2,2,2,2,2,2,2,2,2,2,2,2,2,2,2,2,2,2,2,2,2,2,2,2,2,2,2,2,2,2,2,2,2,
2,2,2,2,2,2,2,2,2,2,2,2,2,2,2,2,2,2,2,2,2,2,2,2,2,2,2,2,2,2,2,2,2,2,2,2,
2,2,2,2,2,2,2,2,2,2,2,2,2,2,2,2,2,2,2,2,2,2,2,2,2,2,2,2,2,2,2,2,2,2,2,2,
2,2,2,2,2,2,2,2,2,2,2,2,2,2,2,2,2,2,2,2,4),(-3.2192985515723,-3.18265944603559,
-3.14434517439237,-3.12271054243446,-3.11144339833662,-3.09560717917629,
-3.05018396632192,-3.04432698129421,-3.00837583280461,-2.98760755445556,
-2.96379769075988,-2.94941525188386,-2.90398453440576,-2.87976174903752,
-2.86901240027736,-2.8559810403335,-2.84772830370259,-2.82310650443899,
-2.76641397725233,-2.7450029092827,-2.7226646827579,-2.67325738302474,-2.63693130363473,
-2.62394592375348,-2.61146205320639,-2.60374130907329,-2.55828575630219,
-2.51923748099461,-2.50015962391689,-2.47818937511186,-2.45431887249412,
-2.4013812793087,-2.3831247563813,-2.37197059794452,-2.35341023317234,-2.32496180164914,
-2.27674090889921,-2.25486002931815,-2.2330793914816,-2.22092455711493,
-2.16324613987547,-2.14124574970439,-2.13069226849502,-2.11723575208084,
-2.10044553346399,-2.05544567550507,-2.02292895824591,-2.00235332073483,
-1.97760819146157,-1.94780682686908,-1.89809023372047,-1.88554351573609,
-1.87263054675197,-1.86449315278697,-1.84042789113114,-1.78934925871981,
-1.76624873104276,-1.74524285504112,-1.70438660485658,-1.65165088707617,
-1.63929599995273,-1.62615086713831,-1.60995173647188,-1.56896776463117,
-1.53333986424049,-1.51272195368063,-1.48920601434088,-1.46209356739356,
-1.41311463885229,-1.39746117381454,-1.3862224074529,-1.36354736859436,
-1.32111552123002,-1.28642196505976,-1.26572381443998,-1.24162980472358,
-1.19332593809121,-1.16059263856094,-1.14795916129151,-1.1351409264376,
-1.07657216580981,-1.04094837950543,-1.02019812166103,-0.996319517697121,
-0.9479470278713,-0.915387861894753,-0.90247232835115,-0.889927778921748,
-0.882147513265054,-0.859751541562816,-0.800584697187891,-0.77886312606304,
-0.766150728356179,-0.745790583365495,-0.713879139954891,-0.677791452497193,
-0.661005985749173,-0.658752994464158,-0.648140347314674,-0.647282893276361,
-0.646370680460327,-0.645371486243262,-0.644248344657781,-0.642956161481402,
-0.642648982649548,-0.642184574832556,-0.641472454273843,-0.640359738802267,
-0.63857978180825,-0.618825466318749,-0.552693910308086,-0.53523534812288,
-0.516484097181045,-0.495003566717608,-0.457359302300728,-0.453922556818062,
-0.422039456846717,-0.409704011905179,-0.3971574922677,-0.391530599966084,
-0.38488729847581,-0.354243021828057,-0.306479274633751,-0.291400620184979,
-0.283460049227869,-0.260608212341912,-0.234157658944324,-0.184731030556678,
-0.168621869564749,-0.158352893080881,-0.145998352350197,-0.123752409919132),
 .UNSPECIFIED.);
#338=B_SPLINE_CURVE_WITH_KNOTS('',3,(#27406,#27407,#27408,#27409,#27410,
#27411,#27412,#27413,#27414,#27415,#27416,#27417,#27418,#27419,#27420,#27421),
 .UNSPECIFIED.,.F.,.F.,(4,1,1,1,1,1,1,1,1,1,1,1,1,4),(84.8230016469245,
85.1322008800429,85.631072815191,86.1299447503392,86.6288166854873,87.1276886206354,
87.6265605557835,88.1254324909317,88.6243044260798,89.1231763612279,89.622048296376,
90.1209202315242,90.6197921666723,90.8551096506934),.UNSPECIFIED.);
#339=B_SPLINE_CURVE_WITH_KNOTS('',3,(#27422,#27423,#27424,#27425,#27426,
#27427,#27428,#27429,#27430,#27431),.UNSPECIFIED.,.F.,.F.,(4,3,3,4),(84.5719056092393,
84.6333289448948,84.7281652959096,84.8230016469245),.UNSPECIFIED.);
#340=B_SPLINE_CURVE_WITH_KNOTS('',3,(#27433,#27434,#27435,#27436,#27437,
#27438,#27439,#27440,#27441,#27442,#27443,#27444),.UNSPECIFIED.,.F.,.F.,
(4,2,2,2,2,4),(-0.123752409919132,-0.0930689444384096,-0.0582089112007299,
-0.0377177607519244,-0.0205407051112054,-4.23346110096705E-5),
 .UNSPECIFIED.);
#341=B_SPLINE_CURVE_WITH_KNOTS('',3,(#27445,#27446,#27447,#27448,#27449,
#27450,#27451,#27452,#27453,#27454,#27455,#27456,#27457,#27458,#27459,#27460),
 .UNSPECIFIED.,.F.,.F.,(4,1,1,1,1,1,1,1,1,1,1,1,1,4),(84.8230016469245,
84.9884465486181,85.4875827733086,85.9867189979992,86.4858552226897,86.9849914473802,
87.4841276720708,87.9832638967613,88.4824001214518,88.9815363461423,89.4806725708329,
89.9798087955234,90.4789450202139,90.855079291793),.UNSPECIFIED.);
#342=B_SPLINE_CURVE_WITH_KNOTS('',3,(#27466,#27467,#27468,#27469,#27470,
#27471,#27472,#27473,#27474,#27475,#27476,#27477,#27478,#27479,#27480,#27481,
#27482,#27483,#27484,#27485,#27486,#27487,#27488,#27489,#27490,#27491,#27492,
#27493,#27494,#27495,#27496,#27497,#27498,#27499,#27500,#27501,#27502,#27503,
#27504,#27505,#27506,#27507,#27508,#27509,#27510,#27511,#27512,#27513,#27514,
#27515,#27516,#27517,#27518,#27519,#27520,#27521,#27522,#27523,#27524,#27525,
#27526,#27527,#27528,#27529,#27530,#27531,#27532,#27533,#27534,#27535,#27536,
#27537,#27538,#27539,#27540,#27541,#27542,#27543,#27544,#27545,#27546,#27547,
#27548,#27549,#27550,#27551,#27552,#27553,#27554,#27555,#27556,#27557,#27558,
#27559,#27560,#27561,#27562,#27563,#27564,#27565,#27566,#27567,#27568,#27569,
#27570,#27571,#27572,#27573,#27574,#27575,#27576,#27577,#27578,#27579,#27580,
#27581,#27582,#27583,#27584,#27585,#27586,#27587,#27588,#27589,#27590,#27591,
#27592,#27593,#27594,#27595,#27596,#27597,#27598,#27599,#27600,#27601,#27602,
#27603,#27604,#27605,#27606,#27607,#27608,#27609,#27610,#27611,#27612,#27613,
#27614,#27615,#27616,#27617,#27618,#27619,#27620,#27621,#27622,#27623,#27624,
#27625,#27626,#27627,#27628,#27629,#27630,#27631,#27632,#27633,#27634,#27635,
#27636,#27637,#27638,#27639,#27640,#27641,#27642,#27643,#27644,#27645,#27646,
#27647,#27648,#27649,#27650,#27651,#27652,#27653,#27654,#27655,#27656,#27657,
#27658,#27659,#27660,#27661,#27662,#27663,#27664,#27665,#27666,#27667,#27668,
#27669,#27670,#27671,#27672,#27673,#27674,#27675,#27676,#27677,#27678,#27679,
#27680,#27681,#27682,#27683,#27684,#27685,#27686,#27687,#27688,#27689,#27690,
#27691,#27692,#27693,#27694,#27695,#27696,#27697,#27698,#27699,#27700,#27701,
#27702,#27703),.UNSPECIFIED.,.F.,.F.,(4,2,2,2,2,2,2,2,2,2,2,2,2,2,2,2,2,
2,2,2,2,2,2,2,2,2,2,2,2,2,2,2,2,2,2,2,2,2,2,2,2,2,2,2,2,2,2,2,2,2,2,2,2,
2,2,2,2,2,2,2,2,2,2,2,2,2,2,2,2,2,2,2,2,2,2,2,2,2,2,2,2,2,2,2,2,2,2,2,2,
2,2,2,2,2,2,2,2,2,2,2,2,2,2,2,2,2,2,2,2,2,2,2,2,2,2,2,2,2,4),(-2.97188390835979,
-2.95930360230679,-2.94813049352868,-2.92654700709351,-2.88824968232717,
-2.85094146776425,-2.83207769380161,-2.81028046180207,-2.78659016540223,
-2.7342946618611,-2.71563441099786,-2.70458798215227,-2.68695057534491,
-2.67352131896951,-2.6192975620724,-2.59420744323309,-2.57409993213815,
-2.54382795260748,-2.4984174132146,-2.47427087862044,-2.46361108093319,
-2.45077211713454,-2.44267676202592,-2.41873573334499,-2.36029330763336,
-2.34127912176928,-2.31971823122944,-2.3077041938349,-2.25312819013689,
-2.22918423253904,-2.2183268607472,-2.20581457084965,-2.19803439701932,
-2.15146502875884,-2.11374129623816,-2.09485613369102,-2.07309568903009,
-2.01988048900073,-2.01717711750618,-1.98453337403748,-1.97213593235675,
-1.95935497884516,-1.95131585634724,-1.90513800086238,-1.86782883109767,
-1.84896506190972,-1.82716795845727,-1.80347787548065,-1.7511836837004,
-1.73252247172757,-1.72147605415282,-1.70383956240128,-1.69041146482386,
-1.63618833630999,-1.61109701791401,-1.59098968567115,-1.56072033362341,
-1.51531892825007,-1.49117296105698,-1.48050940005662,-1.46767744606798,
-1.45958888267165,-1.43568024937039,-1.37840311223537,-1.35705864281533,
-1.33514458589156,-1.31121114205248,-1.2596315246863,-1.24096875896605,
-1.22992235088225,-1.2122873106871,-1.19886105801143,-1.1446388947538,-1.11954563582482,
-1.09943857432114,-1.0691734044744,-1.02378657882265,-0.999641897630113,
-0.98897218144264,-0.976151597421332,-0.968074049488683,-0.944217906727671,
-0.885986113094425,-0.866909016037012,-0.847924122848715,-0.838828430897599,
-0.811976487158419,-0.762174904402619,-0.747083888625468,-0.736041390284051,
-0.72384034197845,-0.712532820093758,-0.668463932200259,-0.63535328159074,
-0.615290171385401,-0.596320400449478,-0.547225528508128,-0.511291014668111,
-0.49846522688991,-0.488471446920141,-0.475344302630777,-0.430194801231896,
-0.393107848696171,-0.374254213376987,-0.355334441256989,-0.291948221686628,
-0.265012553372072,-0.252374515124856,-0.242470545133809,-0.229222440880817,
-0.186963697760637,-0.167084065608167,-0.139497337172782,-0.120655190704037,
-0.101368977746664,-0.0546587056616307,-0.0192581144472614,-0.0087590194227128,
-7.99011461200493E-5),.UNSPECIFIED.);
#343=B_SPLINE_CURVE_WITH_KNOTS('',3,(#27704,#27705,#27706,#27707),
 .UNSPECIFIED.,.F.,.F.,(4,4),(90.8551096506934,91.1061869363603),
 .UNSPECIFIED.);
#344=B_SPLINE_CURVE_WITH_KNOTS('',3,(#27709,#27710,#27711,#27712,#27713),
 .UNSPECIFIED.,.F.,.F.,(4,1,4),(90.855079291793,90.9780812449044,91.106186943595),
 .UNSPECIFIED.);
#345=B_SPLINE_CURVE_WITH_KNOTS('',3,(#27714,#27715,#27716,#27717,#27718,
#27719,#27720,#27721,#27722,#27723,#27724,#27725,#27726,#27727,#27728,#27729,
#27730,#27731,#27732,#27733,#27734,#27735,#27736,#27737,#27738,#27739,#27740,
#27741,#27742,#27743,#27744,#27745,#27746,#27747,#27748,#27749,#27750,#27751,
#27752,#27753,#27754,#27755,#27756,#27757,#27758,#27759,#27760,#27761,#27762,
#27763,#27764,#27765,#27766,#27767,#27768,#27769,#27770,#27771,#27772,#27773,
#27774,#27775,#27776,#27777,#27778,#27779,#27780,#27781,#27782,#27783,#27784,
#27785,#27786,#27787,#27788,#27789,#27790,#27791,#27792,#27793,#27794,#27795,
#27796,#27797,#27798,#27799,#27800,#27801,#27802,#27803,#27804,#27805,#27806,
#27807,#27808,#27809,#27810,#27811,#27812,#27813,#27814,#27815,#27816,#27817,
#27818,#27819,#27820,#27821,#27822,#27823,#27824,#27825,#27826,#27827,#27828,
#27829,#27830,#27831,#27832,#27833,#27834,#27835,#27836,#27837,#27838,#27839,
#27840,#27841,#27842,#27843,#27844,#27845,#27846,#27847,#27848,#27849,#27850,
#27851,#27852,#27853,#27854,#27855,#27856,#27857,#27858,#27859,#27860,#27861,
#27862,#27863,#27864,#27865,#27866,#27867,#27868,#27869,#27870,#27871,#27872,
#27873,#27874,#27875,#27876,#27877,#27878,#27879,#27880,#27881,#27882,#27883,
#27884,#27885,#27886,#27887,#27888,#27889,#27890,#27891,#27892,#27893,#27894,
#27895,#27896,#27897,#27898,#27899,#27900,#27901,#27902,#27903,#27904,#27905,
#27906,#27907,#27908,#27909,#27910,#27911,#27912,#27913,#27914,#27915,#27916,
#27917,#27918,#27919,#27920,#27921,#27922,#27923,#27924,#27925,#27926,#27927,
#27928,#27929,#27930,#27931,#27932,#27933),.UNSPECIFIED.,.F.,.F.,(4,3,3,
3,3,3,3,3,3,3,3,3,3,3,3,3,3,3,3,3,3,3,3,3,3,3,3,3,3,3,3,3,3,3,3,3,3,3,3,
3,3,3,3,3,3,3,3,3,3,3,3,3,3,3,3,3,3,3,3,3,3,3,3,3,3,3,3,3,3,3,3,3,3,4),
(91.1061869541041,91.1937659933166,91.2813481576857,91.3689282889393,91.4565282400459,
91.477217469595,91.5650703351689,91.6529052949637,91.7407433708428,91.8285762824558,
91.9164308439581,91.9763536942855,92.0642065598592,92.1520415196537,92.2398795955327,
92.3277125071459,92.4155670686481,92.475489918976,92.5633427845498,92.6511777443445,
92.7390158202237,92.8268487318367,92.914703293339,92.9746261436665,93.0624790092402,
93.1503139690347,93.2381520449139,93.3259849565268,93.4138395180291,93.4737623683571,
93.561615233931,93.6494501937261,93.7372882696053,93.8251211812183,93.9129757427206,
93.9728985930476,94.0607514586212,94.1485864184154,94.2364244942945,94.3242574059074,
94.4121119674096,94.4720348177381,94.559887683312,94.6477226431064,94.7355607189857,
94.8233936305985,94.9112481921007,94.9711710424286,95.0590239080024,95.1468588677968,
95.2346969436761,95.3225298552889,95.4103844167912,95.4703072671192,95.5581601326931,
95.6459950924875,95.7338331683666,95.8216660799797,95.9095206414821,95.9694434918097,
96.0572963573838,96.1451313171785,96.2329693930575,96.3208023046708,96.4086568661731,
96.4685797165002,96.5564325820741,96.6442675418685,96.7321056177478,96.8199385293601,
96.9077930908624,96.9677159411908,97.0552213902458,97.1382969843455),
 .UNSPECIFIED.);
#346=B_SPLINE_CURVE_WITH_KNOTS('',3,(#27938,#27939,#27940,#27941,#27942,
#27943,#27944,#27945,#27946,#27947,#27948,#27949,#27950,#27951,#27952,#27953,
#27954,#27955,#27956,#27957,#27958,#27959,#27960,#27961,#27962,#27963,#27964,
#27965,#27966,#27967,#27968,#27969,#27970,#27971,#27972,#27973,#27974,#27975,
#27976,#27977,#27978,#27979,#27980,#27981,#27982,#27983,#27984,#27985,#27986,
#27987,#27988,#27989,#27990,#27991,#27992,#27993,#27994,#27995,#27996,#27997,
#27998,#27999,#28000,#28001,#28002,#28003,#28004,#28005,#28006,#28007,#28008,
#28009,#28010,#28011,#28012,#28013,#28014,#28015,#28016,#28017,#28018,#28019,
#28020,#28021,#28022,#28023,#28024,#28025,#28026,#28027,#28028,#28029,#28030,
#28031,#28032,#28033,#28034,#28035,#28036,#28037,#28038,#28039,#28040,#28041,
#28042,#28043,#28044,#28045,#28046,#28047,#28048,#28049,#28050,#28051,#28052,
#28053,#28054,#28055,#28056,#28057,#28058,#28059,#28060,#28061,#28062,#28063,
#28064,#28065,#28066,#28067,#28068,#28069,#28070,#28071,#28072,#28073,#28074,
#28075,#28076,#28077,#28078,#28079,#28080,#28081,#28082,#28083,#28084,#28085,
#28086,#28087,#28088,#28089,#28090,#28091,#28092,#28093,#28094,#28095,#28096,
#28097,#28098,#28099,#28100,#28101,#28102,#28103,#28104,#28105,#28106,#28107,
#28108,#28109,#28110,#28111,#28112,#28113,#28114,#28115,#28116,#28117,#28118,
#28119,#28120,#28121,#28122,#28123,#28124,#28125,#28126,#28127,#28128,#28129,
#28130,#28131,#28132,#28133,#28134,#28135,#28136,#28137,#28138,#28139,#28140,
#28141,#28142,#28143,#28144,#28145,#28146,#28147,#28148,#28149,#28150,#28151,
#28152,#28153,#28154,#28155,#28156,#28157,#28158,#28159,#28160,#28161,#28162,
#28163,#28164,#28165,#28166,#28167,#28168,#28169,#28170,#28171,#28172,#28173,
#28174,#28175,#28176,#28177,#28178,#28179,#28180,#28181,#28182,#28183),
 .UNSPECIFIED.,.F.,.F.,(4,2,2,2,2,2,2,2,2,2,2,2,2,2,2,2,2,2,2,2,2,2,2,2,
2,2,2,2,2,2,2,2,2,2,2,2,2,2,2,2,2,2,2,2,2,2,2,2,2,2,2,2,2,2,2,2,2,2,2,2,
2,2,2,2,2,2,2,2,2,2,2,2,2,2,2,2,2,2,2,2,2,2,2,2,2,2,2,2,2,2,2,2,2,2,2,2,
2,2,2,2,2,2,2,2,2,2,2,2,2,2,2,2,2,2,2,2,2,2,2,2,2,2,4),(-6.06739611659123,
-6.04890634739659,-6.02918138480762,-6.00796119668724,-5.95506196377217,
-5.9281994073552,-5.91055613045296,-5.9062807363049,-5.89454214084383,-5.83796854963403,
-5.7995941317827,-5.78303501833826,-5.76172088759372,-5.69878898354961,
-5.67791540045163,-5.66287162905995,-5.65669994687286,-5.65259798077859,
-5.64823381999523,-5.59912663531025,-5.56848191341442,-5.56008297219719,
-5.55308141228642,-5.53547225595711,-5.51362860225442,-5.46757029749411,
-5.4381626263111,-5.42413864141611,-5.41845996335461,-5.40876425159925,
-5.39237654472097,-5.34264650304186,-5.31670432465222,-5.31405387462264,
-5.31187344235433,-5.30994754658458,-5.30810623452789,-5.28727060032299,
-5.26449143353979,-5.21870031346397,-5.18004364153831,-5.16749269679253,
-5.15666144336242,-5.10735244277498,-5.07681993232706,-5.0518315502198,
-5.03152038230495,-5.0007795558325,-4.95370065078756,-4.94204442086742,
-4.93423933264814,-4.92170138772236,-4.90907275024535,-4.85809638847423,
-4.82553299757179,-4.80253449665306,-4.78202716917478,-4.71367657308658,
-4.69961499356507,-4.68149683208091,-4.67045502268247,-4.65231329247252,
-4.5994060437416,-4.57563740288442,-4.55380253563748,-4.5323942329941,-4.49375889420732,
-4.45812472260172,-4.44286722896336,-4.4302566283844,-4.41770105224706,
-4.37747286092775,-4.32824441071514,-4.30678999234457,-4.28769718524396,
-4.25442037305272,-4.21417271423322,-4.19813566772727,-4.18510505632296,
-4.17454317604071,-4.15131022502166,-4.09555575100564,-4.08341969925314,
-4.0617487929656,-4.04280887834227,-4.00394192561131,-3.96241396068146,
-3.94422729829558,-3.93318544923321,-3.91511182561434,-3.86212235509494,
-3.83834316473064,-3.81650324081526,-3.79766396173923,-3.76082805603957,
-3.7064259906953,-3.69346046251259,-3.68121660739566,-3.64990939718142,
-3.64578850930668,-3.6060966288402,-3.57940795269051,-3.56120830499061,
-3.53549996849126,-3.46001428467461,-3.44729891042931,-3.43484245441477,
-3.39266217414502,-3.34436394152978,-3.32307172655708,-3.30108915425806,
-3.2633031222042,-3.22875502504213,-3.2082301723572,-3.19811308120898,-3.18288470572753,
-3.1343316752737,-3.09558651517567,-3.07503671030317,-3.05215162362301,
-3.02031166947022,-2.97478411742481,-2.97188390835979),.UNSPECIFIED.);
#347=B_SPLINE_CURVE_WITH_KNOTS('',3,(#28185,#28186,#28187,#28188,#28189,
#28190,#28191,#28192,#28193,#28194),.UNSPECIFIED.,.F.,.F.,(4,3,3,4),(97.1382969843455,
97.2257767656916,97.3132734200704,97.3893722574151),.UNSPECIFIED.);
#348=B_SPLINE_CURVE_WITH_KNOTS('',3,(#28195,#28196,#28197,#28198,#28199,
#28200,#28201,#28202,#28203,#28204,#28205,#28206,#28207,#28208,#28209,#28210),
 .UNSPECIFIED.,.F.,.F.,(4,1,1,1,1,1,1,1,1,1,1,1,1,4),(97.3893722612837,
97.4668521658813,97.9659883905718,98.4651246152623,98.9642608399529,99.4633970646434,
99.9625332893339,100.461669514024,100.960805738715,101.459941963405,101.959078188096,
102.458214412787,102.957350637477,103.421463986725),.UNSPECIFIED.);
#349=B_SPLINE_CURVE_WITH_KNOTS('',3,(#28216,#28217,#28218,#28219,#28220,
#28221,#28222,#28223,#28224,#28225,#28226,#28227,#28228,#28229,#28230,#28231,
#28232,#28233,#28234,#28235,#28236,#28237,#28238,#28239,#28240,#28241,#28242,
#28243,#28244,#28245,#28246,#28247,#28248,#28249,#28250,#28251,#28252,#28253,
#28254,#28255,#28256,#28257,#28258,#28259,#28260,#28261,#28262,#28263,#28264,
#28265,#28266,#28267,#28268,#28269,#28270,#28271,#28272,#28273,#28274,#28275,
#28276,#28277,#28278,#28279,#28280,#28281,#28282,#28283,#28284,#28285,#28286,
#28287,#28288,#28289,#28290,#28291,#28292,#28293,#28294,#28295,#28296,#28297,
#28298,#28299,#28300,#28301,#28302,#28303,#28304,#28305,#28306,#28307,#28308,
#28309,#28310,#28311,#28312,#28313,#28314,#28315,#28316,#28317,#28318,#28319,
#28320,#28321,#28322,#28323,#28324,#28325,#28326,#28327,#28328,#28329,#28330,
#28331,#28332,#28333,#28334,#28335,#28336,#28337,#28338,#28339,#28340,#28341,
#28342,#28343,#28344,#28345,#28346,#28347,#28348,#28349,#28350,#28351,#28352,
#28353,#28354,#28355,#28356,#28357,#28358,#28359,#28360,#28361,#28362,#28363,
#28364,#28365,#28366,#28367,#28368,#28369,#28370,#28371,#28372,#28373,#28374,
#28375,#28376,#28377,#28378,#28379,#28380,#28381,#28382,#28383,#28384,#28385,
#28386,#28387,#28388,#28389,#28390,#28391,#28392,#28393,#28394,#28395,#28396,
#28397,#28398,#28399,#28400,#28401,#28402,#28403,#28404,#28405,#28406,#28407,
#28408,#28409,#28410,#28411,#28412,#28413,#28414,#28415,#28416,#28417,#28418,
#28419,#28420,#28421,#28422,#28423,#28424,#28425,#28426,#28427,#28428,#28429,
#28430,#28431,#28432,#28433,#28434,#28435,#28436,#28437,#28438,#28439,#28440,
#28441,#28442,#28443,#28444,#28445,#28446,#28447,#28448,#28449,#28450,#28451),
 .UNSPECIFIED.,.F.,.F.,(4,2,2,2,2,2,2,2,2,2,2,2,2,2,2,2,2,2,2,2,2,2,2,2,
2,2,2,2,2,2,2,2,2,2,2,2,2,2,2,2,2,2,2,2,2,2,2,2,2,2,2,2,2,2,2,2,2,2,2,2,
2,2,2,2,2,2,2,2,2,2,2,2,2,2,2,2,2,2,2,2,2,2,2,2,2,2,2,2,2,2,2,2,2,2,2,2,
2,2,2,2,2,2,2,2,2,2,2,2,2,2,2,2,2,2,2,2,2,4),(-2.97195104590692,-2.96785731741696,
-2.92217885664269,-2.90936567333568,-2.89699615966277,-2.88935476710183,
-2.84416880408123,-2.82633349817458,-2.7976174272583,-2.77738972113305,
-2.75124194836679,-2.69474988104159,-2.67275371403184,-2.66228603455495,
-2.64904430325233,-2.6326094660691,-2.58975433302553,-2.55560533913252,
-2.53510160348009,-2.51128689789865,-2.46322801939443,-2.42809306775177,
-2.41733468308247,-2.40466748949289,-2.38930635285144,-2.35309235177817,
-2.31337370536685,-2.29442627164094,-2.27276611417383,-2.22958865696618,
-2.18956041580427,-2.17461787750089,-2.16328164650938,-2.13921313100205,
-2.08610587199597,-2.06144679348156,-2.04116654530749,-2.01585568527845,
-1.95838610543814,-1.93557379016381,-1.92506922811594,-1.91191309731386,
-1.89564032229228,-1.85386995916075,-1.8219345708956,-1.80296702805452,
-1.78133735396513,-1.76924711468633,-1.71115127327577,-1.68923066226832,
-1.67785911475009,-1.66354145407655,-1.61685984184392,-1.57530039887851,
-1.55647003830275,-1.5346128076183,-1.510797731504,-1.4575362420338,-1.43968161753604,
-1.42863823220506,-1.41022095978168,-1.3820622104627,-1.33347822731307,
-1.3117702180792,-1.29024962363137,-1.24226814993072,-1.20093905597605,
-1.18843740533266,-1.17577030489421,-1.16040936699153,-1.124196657836,-1.08447356358303,
-1.06552644824461,-1.0438656239945,-1.00068136685562,-0.960750293559231,
-0.945763688633204,-0.934437899479715,-0.91052378709959,-0.862241766807108,
-0.832374395201497,-0.81286113588637,-0.79127147505588,-0.763678287012345,
-0.707459976144883,-0.695686116009359,-0.684387070609555,-0.683232880624469,
-0.681867153745732,-0.664640140195931,-0.615990580307078,-0.586381523641675,
-0.570730661414335,-0.548681768559753,-0.523265479697681,-0.469984555741397,
-0.454593127443027,-0.444132045810674,-0.441361870022094,-0.438892899662171,
-0.435173421070681,-0.417129760065319,-0.361528325738389,-0.336380334968567,
-0.328730230085166,-0.325211210846139,-0.323035602891817,-0.320473782055981,
-0.295654411923943,-0.26462716457408,-0.217428748493838,-0.205073931066454,
-0.192832984744859,-0.119422015026088,-0.0949473551364795,-0.075450854731309,
-0.0563330778625723,-7.60666707596163E-5),.UNSPECIFIED.);
#350=B_SPLINE_CURVE_WITH_KNOTS('',3,(#28452,#28453,#28454,#28455,#28456,
#28457,#28458,#28459,#28460,#28461,#28462,#28463,#28464,#28465),
 .UNSPECIFIED.,.F.,.F.,(4,2,2,2,2,2,4),(-6.19108034638175,-6.17183981108263,
-6.16031491317487,-6.15046655821583,-6.13776449339168,-6.09803741160187,
-6.06739611659123),.UNSPECIFIED.);
#351=B_SPLINE_CURVE_WITH_KNOTS('',3,(#28467,#28468,#28469,#28470,#28471),
 .UNSPECIFIED.,.F.,.F.,(4,1,4),(103.421463986725,103.456486862168,103.672557546372),
 .UNSPECIFIED.);
#352=B_SPLINE_CURVE_WITH_KNOTS('',3,(#28472,#28473,#28474,#28475,#28476,
#28477,#28478,#28479,#28480,#28481,#28482,#28483,#28484,#28485,#28486,#28487,
#28488,#28489,#28490,#28491,#28492,#28493,#28494,#28495,#28496,#28497,#28498,
#28499,#28500,#28501,#28502,#28503,#28504,#28505,#28506,#28507,#28508,#28509,
#28510,#28511,#28512,#28513,#28514,#28515,#28516,#28517,#28518,#28519,#28520,
#28521,#28522,#28523,#28524,#28525,#28526,#28527,#28528,#28529,#28530,#28531,
#28532,#28533,#28534,#28535,#28536,#28537,#28538,#28539,#28540,#28541,#28542,
#28543,#28544,#28545,#28546,#28547,#28548,#28549,#28550,#28551,#28552,#28553,
#28554,#28555,#28556,#28557,#28558,#28559,#28560,#28561,#28562,#28563,#28564,
#28565,#28566,#28567,#28568,#28569,#28570,#28571,#28572,#28573,#28574,#28575,
#28576,#28577,#28578,#28579,#28580,#28581,#28582,#28583,#28584,#28585,#28586,
#28587,#28588,#28589,#28590,#28591,#28592,#28593,#28594,#28595,#28596,#28597,
#28598,#28599,#28600,#28601,#28602,#28603,#28604,#28605,#28606,#28607,#28608,
#28609,#28610,#28611,#28612,#28613,#28614,#28615,#28616,#28617,#28618,#28619,
#28620,#28621,#28622,#28623,#28624,#28625,#28626,#28627,#28628,#28629,#28630,
#28631,#28632,#28633,#28634,#28635,#28636,#28637,#28638,#28639,#28640,#28641,
#28642,#28643,#28644,#28645,#28646,#28647,#28648,#28649,#28650,#28651,#28652,
#28653,#28654,#28655,#28656,#28657,#28658,#28659,#28660,#28661,#28662,#28663,
#28664,#28665,#28666,#28667,#28668,#28669,#28670,#28671,#28672,#28673,#28674,
#28675,#28676,#28677,#28678,#28679,#28680,#28681,#28682,#28683,#28684,#28685,
#28686,#28687,#28688,#28689,#28690,#28691,#28692,#28693,#28694,#28695,#28696,
#28697,#28698,#28699,#28700,#28701,#28702,#28703,#28704,#28705,#28706,#28707,
#28708,#28709,#28710,#28711,#28712,#28713,#28714,#28715,#28716,#28717),
 .UNSPECIFIED.,.F.,.F.,(4,2,2,2,2,2,2,2,2,2,2,2,2,2,2,2,2,2,2,2,2,2,2,2,
2,2,2,2,2,2,2,2,2,2,2,2,2,2,2,2,2,2,2,2,2,2,2,2,2,2,2,2,2,2,2,2,2,2,2,2,
2,2,2,2,2,2,2,2,2,2,2,2,2,2,2,2,2,2,2,2,2,2,2,2,2,2,2,2,2,2,2,2,2,2,2,2,
2,2,2,2,2,2,2,2,2,2,2,2,2,2,2,2,2,2,2,2,2,2,2,2,2,2,4),(-6.19125288673404,
-6.17508219709553,-6.15753828259376,-6.11890984406139,-6.06250600267116,
-6.0524853606948,-6.04017426316179,-6.01332573894149,-5.97047335452146,
-5.94807557503419,-5.92894927198427,-5.90931059639689,-5.84407907151587,
-5.82109036638719,-5.81587510621001,-5.80596728296801,-5.79507843430614,
-5.75653171497579,-5.72958245957422,-5.70558689319716,-5.68651984516126,
-5.66705175205571,-5.6641559080366,-5.60425624187656,-5.58082308107648,
-5.57594514987642,-5.57302517221989,-5.57101555516809,-5.56957655694856,
-5.5595755231996,-5.54659016163239,-5.51026850910374,-5.47416556457379,
-5.45297783343695,-5.43347707129468,-5.41558498912886,-5.35044439733363,
-5.33122320336565,-5.3295909586851,-5.32865538683616,-5.32811778636156,
-5.32780797684332,-5.32654555762053,-5.32551152573869,-5.32465588809124,
-5.31465419817859,-5.30229036980523,-5.25735975327803,-5.2122888585239,
-5.19060495819653,-5.16861900165768,-5.12240154924134,-5.08040741364554,
-5.06785874457934,-5.05494799488295,-5.0223860941896,-4.97401732211412,
-4.95013675861123,-4.92938711638593,-4.89494423688343,-4.85265005010578,
-4.83000771555363,-4.8187711618381,-4.80310566556307,-4.75411942988798,
-4.72702283520463,-4.70351428385425,-4.68289430727978,-4.64723106888212,
-4.60628148935744,-4.59008741573791,-4.57694516150772,-4.56458820386378,
-4.51955815990319,-4.47542462339307,-4.45354349280265,-4.43441048738455,
-4.38606085447809,-4.35572649014296,-4.33650430271747,-4.32534082603624,
-4.30766550428407,-4.25402043504048,-4.23006041690325,-4.20804738425489,
-4.18899481938808,-4.14921542231969,-4.10398524131171,-4.08813957479584,
-4.07682472514551,-4.05953706342537,-4.00896908886919,-3.98471358475004,
-3.96255920837257,-3.94358332940043,-3.90675480382874,-3.85213066297697,
-3.83908227614756,-3.8283418059308,-3.80411735082831,-3.7586690931932,-3.74428449282565,
-3.72047259794651,-3.69970478302615,-3.66376438673982,-3.62269242749822,
-3.60647926546033,-3.59332682923647,-3.58097747450412,-3.54856941972768,
-3.54559334511914,-3.49329007397899,-3.47103271320139,-3.44956483935213,
-3.39195886652383,-3.36802134121612,-3.35991063287445,-3.34702523428542,
-3.33445369996295,-3.29310435540861,-3.24485406110885,-3.22320627505701,
-3.21940741207938),.UNSPECIFIED.);
#353=B_SPLINE_CURVE_WITH_KNOTS('',3,(#28722,#28723,#28724,#28725,#28726,
#28727,#28728,#28729,#28730,#28731,#28732,#28733,#28734,#28735,#28736,#28737,
#28738,#28739,#28740,#28741,#28742,#28743,#28744,#28745,#28746,#28747,#28748,
#28749,#28750,#28751,#28752,#28753,#28754,#28755,#28756,#28757,#28758,#28759,
#28760,#28761,#28762,#28763,#28764,#28765,#28766,#28767,#28768,#28769,#28770,
#28771,#28772,#28773,#28774,#28775,#28776,#28777,#28778,#28779,#28780,#28781,
#28782,#28783,#28784,#28785,#28786,#28787,#28788,#28789,#28790,#28791,#28792,
#28793,#28794,#28795,#28796,#28797,#28798,#28799,#28800,#28801,#28802,#28803,
#28804,#28805,#28806,#28807,#28808,#28809,#28810,#28811,#28812,#28813,#28814,
#28815,#28816,#28817,#28818,#28819,#28820,#28821,#28822,#28823,#28824,#28825,
#28826,#28827,#28828,#28829,#28830,#28831,#28832,#28833,#28834,#28835,#28836,
#28837,#28838,#28839,#28840,#28841,#28842,#28843,#28844,#28845,#28846,#28847,
#28848,#28849,#28850,#28851,#28852,#28853,#28854,#28855,#28856,#28857,#28858,
#28859,#28860,#28861,#28862,#28863,#28864,#28865,#28866,#28867,#28868,#28869,
#28870,#28871,#28872,#28873,#28874,#28875,#28876,#28877,#28878,#28879,#28880,
#28881,#28882,#28883,#28884,#28885,#28886,#28887,#28888,#28889,#28890,#28891,
#28892,#28893,#28894,#28895,#28896,#28897,#28898,#28899,#28900,#28901,#28902,
#28903,#28904,#28905,#28906,#28907,#28908,#28909,#28910,#28911,#28912,#28913,
#28914,#28915,#28916,#28917,#28918,#28919,#28920,#28921,#28922,#28923,#28924,
#28925,#28926,#28927,#28928,#28929,#28930,#28931,#28932,#28933,#28934,#28935,
#28936,#28937,#28938,#28939,#28940,#28941,#28942,#28943,#28944,#28945,#28946,
#28947,#28948,#28949,#28950,#28951,#28952,#28953,#28954,#28955,#28956,#28957,
#28958,#28959,#28960,#28961),.UNSPECIFIED.,.F.,.F.,(4,2,2,2,2,2,2,2,2,2,
2,2,2,2,2,2,2,2,2,2,2,2,2,2,2,2,2,2,2,2,2,2,2,2,2,2,2,2,2,2,2,2,2,2,2,2,
2,2,2,2,2,2,2,2,2,2,2,2,2,2,2,2,2,2,2,2,2,2,2,2,2,2,2,2,2,2,2,2,2,2,2,2,
2,2,2,2,2,2,2,2,2,2,2,2,2,2,2,2,2,2,2,2,2,2,2,2,2,2,2,2,2,2,2,2,2,2,2,2,
2,4),(-6.06743986436456,-6.05146266686438,-6.0170766699814,-5.99084287541892,
-5.97507687341059,-5.95074837268195,-5.8929187530285,-5.87463693518481,
-5.86344954632942,-5.85855813820818,-5.8461204240607,-5.7970592585569,-5.76703887105114,
-5.7427810693363,-5.72341768441375,-5.69487220762185,-5.645197661881,-5.62784180292691,
-5.61429260539229,-5.60778130290437,-5.59112163908842,-5.54146782770256,
-5.51568819018526,-5.5071799204263,-5.4895290323691,-5.4678741999934,-5.41239384283465,
-5.38824717806325,-5.37545860914837,-5.36723691164706,-5.35660471760888,
-5.33278319787387,-5.32061964495729,-5.27250869023555,-5.24885362716181,
-5.2283114013168,-5.19350239543318,-5.15138697292266,-5.13506185151351,
-5.12187822882361,-5.1113858862278,-5.08865910725165,-5.03202786703808,
-5.01990971238666,-4.99825483855614,-4.9793041181001,-4.93913632900284,
-4.90324785383206,-4.88794451549379,-4.87530890994602,-4.86277733620302,
-4.82205159650951,-4.77315900980552,-4.75172577616791,-4.72991981159943,
-4.67916751260443,-4.64148640859403,-4.62910999337595,-4.6163049389692,
-4.57927154320596,-4.54353448850621,-4.51643130035729,-4.49622539640922,
-4.46868052514976,-4.44871989026378,-4.40643226541081,-4.38883545317932,
-4.37778823478465,-4.35908074563864,-4.30684418683341,-4.28316228806938,
-4.26136893995054,-4.24250292108282,-4.2051415728905,-4.15898680497175,
-4.15095776999203,-4.13818734348755,-4.12578054895554,-4.08271636562276,
-4.03613866044279,-4.01463791746702,-3.99290855769124,-3.94279694223018,
-3.91563756117052,-3.89758991726223,-3.8865478433578,-3.86833414291467,
-3.81551251706288,-3.79175467510695,-3.76992485541263,-3.75107950282549,
-3.71414646890209,-3.66884927313065,-3.6513996393683,-3.64034890417972,
-3.62146488716467,-3.58915375469089,-3.54546932724234,-3.52376446640606,
-3.50224119236757,-3.4495260603246,-3.4234128377245,-3.40576488281478,-3.39471862304028,
-3.37607046366351,-3.32376422005898,-3.30007316990067,-3.27827539637536,
-3.25941182166347,-3.22211370384445,-3.17592639552706,-3.16788422257047,
-3.1551002096396,-3.14270532815845,-3.09565991500632,-3.05150376830842,
-3.03241680025527,-3.01095404856947,-2.99904967789612,-2.97195104590692),
 .UNSPECIFIED.);
#354=B_SPLINE_CURVE_WITH_KNOTS('',3,(#28962,#28963,#28964,#28965,#28966,
#28967,#28968,#28969,#28970,#28971,#28972,#28973,#28974,#28975,#28976,#28977,
#28978,#28979,#28980,#28981,#28982,#28983,#28984,#28985,#28986,#28987,#28988,
#28989,#28990,#28991,#28992,#28993,#28994,#28995,#28996,#28997,#28998,#28999,
#29000,#29001,#29002,#29003,#29004,#29005,#29006,#29007,#29008,#29009,#29010,
#29011,#29012,#29013,#29014,#29015,#29016,#29017,#29018,#29019,#29020,#29021,
#29022,#29023,#29024,#29025,#29026,#29027,#29028,#29029,#29030,#29031,#29032,
#29033,#29034,#29035,#29036,#29037,#29038,#29039,#29040,#29041,#29042,#29043,
#29044,#29045,#29046,#29047,#29048,#29049,#29050,#29051,#29052,#29053,#29054,
#29055,#29056,#29057,#29058,#29059,#29060,#29061,#29062,#29063,#29064,#29065,
#29066,#29067,#29068,#29069,#29070,#29071,#29072,#29073,#29074,#29075,#29076,
#29077,#29078,#29079,#29080,#29081,#29082,#29083,#29084,#29085,#29086,#29087,
#29088,#29089,#29090,#29091,#29092,#29093,#29094,#29095,#29096,#29097,#29098,
#29099,#29100,#29101,#29102,#29103,#29104,#29105,#29106,#29107,#29108,#29109,
#29110,#29111,#29112,#29113,#29114,#29115,#29116,#29117,#29118,#29119,#29120,
#29121,#29122,#29123,#29124,#29125,#29126,#29127,#29128,#29129,#29130,#29131,
#29132,#29133,#29134,#29135,#29136,#29137,#29138,#29139,#29140,#29141,#29142,
#29143,#29144,#29145,#29146,#29147,#29148,#29149,#29150,#29151,#29152,#29153,
#29154,#29155,#29156,#29157,#29158,#29159,#29160,#29161,#29162,#29163,#29164,
#29165,#29166,#29167,#29168,#29169,#29170,#29171,#29172,#29173,#29174,#29175,
#29176,#29177,#29178,#29179,#29180,#29181,#29182,#29183,#29184,#29185,#29186,
#29187,#29188,#29189,#29190,#29191,#29192,#29193,#29194,#29195,#29196,#29197,
#29198,#29199,#29200,#29201,#29202,#29203,#29204,#29205,#29206,#29207,#29208,
#29209,#29210,#29211,#29212,#29213,#29214,#29215,#29216,#29217,#29218,#29219,
#29220,#29221,#29222,#29223),.UNSPECIFIED.,.F.,.F.,(4,2,2,2,2,2,2,2,2,2,
2,2,2,2,2,2,2,2,2,2,2,2,2,2,2,2,2,2,2,2,2,2,2,2,2,2,2,2,2,2,2,2,2,2,2,2,
2,2,2,2,2,2,2,2,2,2,2,2,2,2,2,2,2,2,2,2,2,2,2,2,2,2,2,2,2,2,2,2,2,2,2,2,
2,2,2,2,2,2,2,2,2,2,2,2,2,2,2,2,2,2,2,2,2,2,2,2,2,2,2,2,2,2,2,2,2,2,2,2,
2,2,2,2,2,2,2,2,2,2,2,2,4),(-3.21940741207938,-3.20117837848131,-3.15588003122262,
-3.12595304682234,-3.10687043466454,-3.09570977334897,-3.07791981249033,
-3.05153371237635,-2.99960101454642,-2.97780527749097,-2.95593992425781,
-2.87092302223556,-2.85679505762079,-2.84501212794811,-2.81485048994345,
-2.74936479065764,-2.72860014541299,-2.70550726384004,-2.69191442073332,
-2.65171987798415,-2.62060564968142,-2.60829625257774,-2.59509036618975,
-2.5787768250194,-2.53704972617425,-2.50491961757408,-2.48580264052286,
-2.46389527817565,-2.41044503118838,-2.40854592004315,-2.37584543693753,
-2.3631076293498,-2.35039614146276,-2.30864030969151,-2.26265562533825,
-2.24065874607255,-2.2189837041233,-2.17598350112437,-2.12814508283956,
-2.11720340539568,-2.10450034971466,-2.0627800231029,-2.01672470947108,
-1.99473110567979,-1.97305313935917,-1.92407146269707,-1.88370548692773,
-1.8710864861823,-1.85825247345477,-1.8501917539699,-1.80389052367407,-1.76648864922323,
-1.74748059586703,-1.7253862397806,-1.70125630104755,-1.67382182127231,
-1.63675971082746,-1.62451665716257,-1.61121877010471,-1.59473104313657,
-1.55184116828966,-1.5175512474389,-1.49687579507737,-1.47267773194202,
-1.42440291811256,-1.39168762928195,-1.37914506198586,-1.36622702846646,
-1.35808477458443,-1.3339964509513,-1.27604631115371,-1.25680965980543,
-1.23507815074704,-1.2229784031365,-1.16522997130604,-1.14282866581271,
-1.13232056012668,-1.11874642667915,-1.1017303985035,-1.05507827256674,
-1.02385015226429,-1.00334194709201,-0.978077252158774,-0.935609070481279,
-0.89939383293148,-0.887021411230156,-0.873898687661494,-0.873067260651591,
-0.872019630484148,-0.870687618612639,-0.851714784252702,-0.788620684246302,
-0.766248788602609,-0.758609375565332,-0.739412613818327,-0.713963257522252,
-0.66398644077587,-0.646760463165984,-0.636086158627321,-0.635068227654396,
-0.634063832159682,-0.633021295070353,-0.631896801722091,-0.630646112338921,
-0.629987326553337,-0.629053869885849,-0.627689839121058,-0.625630802015863,
-0.622430342610499,-0.600961522933363,-0.539016431020233,-0.519877953041265,
-0.500527453506894,-0.47854250127256,-0.438115582836877,-0.407363034767613,
-0.395060571615654,-0.393906197711282,-0.380303664839752,-0.367834103227159,
-0.332033843084473,-0.292312088127189,-0.274470994541147,-0.265337195509639,
-0.245997058404553,-0.219525231519165,-0.170112023501597,-0.154024091758782,
-0.143763021626771,-0.128863813576066,-0.123785925501408),.UNSPECIFIED.);
#355=B_SPLINE_CURVE_WITH_KNOTS('',3,(#29229,#29230,#29231,#29232,#29233,
#29234,#29235,#29236,#29237,#29238,#29239,#29240,#29241,#29242,#29243,#29244,
#29245,#29246,#29247,#29248,#29249,#29250,#29251,#29252,#29253,#29254,#29255,
#29256,#29257,#29258,#29259,#29260,#29261,#29262,#29263,#29264,#29265,#29266,
#29267,#29268,#29269,#29270,#29271,#29272,#29273,#29274,#29275,#29276,#29277,
#29278,#29279,#29280,#29281,#29282,#29283,#29284,#29285,#29286,#29287,#29288,
#29289,#29290,#29291,#29292,#29293,#29294,#29295,#29296,#29297,#29298,#29299,
#29300,#29301,#29302,#29303,#29304,#29305,#29306,#29307,#29308,#29309,#29310,
#29311,#29312,#29313,#29314,#29315,#29316,#29317,#29318,#29319,#29320,#29321,
#29322,#29323,#29324,#29325,#29326,#29327,#29328,#29329,#29330,#29331,#29332,
#29333,#29334,#29335,#29336,#29337,#29338,#29339,#29340,#29341,#29342,#29343,
#29344,#29345,#29346,#29347,#29348,#29349,#29350,#29351,#29352,#29353,#29354,
#29355,#29356,#29357,#29358,#29359,#29360,#29361,#29362,#29363,#29364,#29365,
#29366,#29367,#29368,#29369,#29370,#29371,#29372,#29373,#29374,#29375,#29376,
#29377,#29378,#29379,#29380,#29381,#29382,#29383,#29384,#29385,#29386,#29387,
#29388,#29389,#29390,#29391,#29392,#29393,#29394,#29395,#29396,#29397,#29398,
#29399,#29400,#29401,#29402,#29403,#29404,#29405,#29406,#29407,#29408,#29409,
#29410,#29411,#29412,#29413,#29414,#29415,#29416,#29417,#29418,#29419,#29420,
#29421,#29422,#29423,#29424,#29425,#29426,#29427,#29428,#29429,#29430,#29431,
#29432,#29433,#29434,#29435,#29436,#29437,#29438,#29439,#29440,#29441,#29442,
#29443,#29444,#29445,#29446,#29447,#29448,#29449,#29450,#29451,#29452,#29453,
#29454,#29455,#29456,#29457,#29458,#29459,#29460,#29461,#29462,#29463,#29464,
#29465,#29466,#29467,#29468,#29469,#29470,#29471,#29472,#29473,#29474,#29475,
#29476,#29477,#29478,#29479,#29480,#29481,#29482),.UNSPECIFIED.,.F.,.F.,
(4,2,2,2,2,2,2,2,2,2,2,2,2,2,2,2,2,2,2,2,2,2,2,2,2,2,2,2,2,2,2,2,2,2,2,
2,2,2,2,2,2,2,2,2,2,2,2,2,2,2,2,2,2,2,2,2,2,2,2,2,2,2,2,2,2,2,2,2,2,2,2,
2,2,2,2,2,2,2,2,2,2,2,2,2,2,2,2,2,2,2,2,2,2,2,2,2,2,2,2,2,2,2,2,2,2,2,2,
2,2,2,2,2,2,2,2,2,2,2,2,2,2,2,2,2,2,2,4),(-2.97204421563466,-2.96411068123968,
-2.91744367631199,-2.87468121859989,-2.86225627162148,-2.8495052821607,
-2.81643080078128,-2.75973433747324,-2.73844941655722,-2.71645538238226,
-2.69235672589235,-2.63682392554474,-2.6208865987792,-2.61089675711181,
-2.59229885871006,-2.56364055208758,-2.51609147438116,-2.49432403669667,
-2.47285582380535,-2.42766606843871,-2.38273041990521,-2.37044184460446,
-2.3575310111409,-2.34936596508652,-2.3250909908574,-2.26749621386711,-2.24843365123487,
-2.22693735535935,-2.17901952237725,-2.13748589935439,-2.12499437112371,
-2.11231580970935,-2.09693398244242,-2.06060476202399,-2.02122610212621,
-2.00224796063232,-1.98063278146582,-1.9685589308996,-1.91009425903436,
-1.88753569297473,-1.87635206914754,-1.86133426404452,-1.8413472171381,
-1.77340321453001,-1.75288179754832,-1.7299184410829,-1.69747867221596,
-1.64588080607389,-1.63339633250518,-1.62071037317785,-1.61276318198242,
-1.5657548315989,-1.52882260262654,-1.5099769082946,-1.4881460057099,-1.464386274588,
-1.41155957705095,-1.3933451321187,-1.38230270391219,-1.36425463894452,
-1.3370948705326,-1.28698789859071,-1.26525771895218,-1.24375639243774,
-1.18798419266902,-1.17421962352946,-1.15156001482275,-1.14107712158639,
-1.12787039252154,-1.11150211520354,-1.06909793887235,-1.034548961541,-1.01402136076166,
-0.990304325809183,-0.942210960313155,-0.928498812103099,-0.905803140557983,
-0.895315086773724,-0.882120503240361,-0.881753868598437,-0.881287986439464,
-0.880692398365737,-0.879925715301487,-0.861676218366873,-0.804152975018271,
-0.779682918535555,-0.778017706347123,-0.776026791239908,-0.77270629154702,
-0.759036201349059,-0.738529908225396,-0.705360058728234,-0.662588316996233,
-0.650164056121249,-0.639214429830502,-0.638006790607304,-0.636602107646557,
-0.635744690185578,-0.634405220189693,-0.632261065419,-0.612125061447222,
-0.546670820709636,-0.528919190454727,-0.510033755830493,-0.4884871100927,
-0.449947882730136,-0.417237674486417,-0.404645601880206,-0.403780615437516,
-0.391218892841825,-0.390362601025878,-0.386943243723255,-0.37254514149451,
-0.32491051586424,-0.294989975079325,-0.281226405983203,-0.276231233184317,
-0.252655688206253,-0.224716300277075,-0.168762783551146,-0.158197035656233,
-0.151256244051262,-0.130480181326522,-0.053707851031223,-0.0332280819668891,
-0.0177128010838843,-7.60539288497946E-5),.UNSPECIFIED.);
#356=B_SPLINE_CURVE_WITH_KNOTS('',3,(#29483,#29484,#29485,#29486,#29487,
#29488,#29489,#29490,#29491,#29492,#29493,#29494),.UNSPECIFIED.,.F.,.F.,
(4,2,2,2,2,4),(-6.19114003241633,-6.12736564474044,-6.11393757622783,-6.10413348852557,
-6.09157219568023,-6.06743986436456),.UNSPECIFIED.);
#357=B_SPLINE_CURVE_WITH_KNOTS('',3,(#29496,#29497,#29498,#29499,#29500,
#29501,#29502,#29503,#29504,#29505),.UNSPECIFIED.,.F.,.F.,(4,2,2,2,4),(-0.123785925501408,
-0.0778141641564192,-0.0430456999861967,-0.022634408400357,-7.62206233211306E-5),
 .UNSPECIFIED.);
#358=B_SPLINE_CURVE_WITH_KNOTS('',3,(#29506,#29507,#29508,#29509,#29510,
#29511,#29512,#29513,#29514,#29515,#29516,#29517,#29518,#29519,#29520,#29521,
#29522,#29523,#29524,#29525,#29526,#29527,#29528,#29529,#29530,#29531,#29532,
#29533,#29534,#29535,#29536,#29537,#29538,#29539,#29540,#29541,#29542,#29543,
#29544,#29545,#29546,#29547,#29548,#29549,#29550,#29551,#29552,#29553,#29554,
#29555,#29556,#29557,#29558,#29559,#29560,#29561,#29562,#29563,#29564,#29565,
#29566,#29567,#29568,#29569,#29570,#29571,#29572,#29573,#29574,#29575,#29576,
#29577,#29578,#29579,#29580,#29581,#29582,#29583,#29584,#29585,#29586,#29587,
#29588,#29589,#29590,#29591,#29592,#29593,#29594,#29595,#29596,#29597,#29598,
#29599,#29600,#29601,#29602,#29603,#29604,#29605,#29606,#29607,#29608,#29609,
#29610,#29611,#29612,#29613,#29614,#29615,#29616,#29617,#29618,#29619,#29620,
#29621,#29622,#29623,#29624,#29625,#29626,#29627,#29628,#29629,#29630,#29631,
#29632,#29633,#29634,#29635,#29636,#29637,#29638,#29639,#29640,#29641,#29642,
#29643,#29644,#29645,#29646,#29647,#29648,#29649,#29650,#29651,#29652,#29653,
#29654,#29655,#29656,#29657,#29658,#29659,#29660,#29661,#29662,#29663,#29664,
#29665,#29666,#29667,#29668,#29669,#29670,#29671,#29672,#29673,#29674,#29675,
#29676,#29677,#29678,#29679,#29680,#29681,#29682,#29683,#29684,#29685,#29686,
#29687,#29688,#29689,#29690,#29691,#29692,#29693,#29694,#29695,#29696,#29697,
#29698,#29699,#29700,#29701,#29702,#29703,#29704,#29705,#29706,#29707,#29708,
#29709,#29710,#29711,#29712,#29713,#29714,#29715,#29716,#29717,#29718,#29719,
#29720,#29721,#29722,#29723,#29724,#29725),.UNSPECIFIED.,.F.,.F.,(4,3,3,
3,3,3,3,3,3,3,3,3,3,3,3,3,3,3,3,3,3,3,3,3,3,3,3,3,3,3,3,3,3,3,3,3,3,3,3,
3,3,3,3,3,3,3,3,3,3,3,3,3,3,3,3,3,3,3,3,3,3,3,3,3,3,3,3,3,3,3,3,3,3,4),
(116.23892818295,116.329038697768,116.419178925844,116.434028704121,116.521881569694,
116.609716529488,116.697554605367,116.78538751698,116.873242078482,116.933164928812,
117.021017794386,117.108852754181,117.19669083006,117.284523741674,117.372378303176,
117.432301153502,117.520154019075,117.607988978869,117.695827054748,117.783659966361,
117.871514527863,117.931437378193,118.019290243767,118.107125203562,118.194963279442,
118.282796191055,118.370650752558,118.430573602883,118.518426468456,118.60626142825,
118.694099504129,118.781932415742,118.869786977244,118.929709827574,119.017562693148,
119.105397652943,119.193235728823,119.281068640436,119.368923201939,119.428846052264,
119.516698917837,119.604533877631,119.69237195351,119.780204865123,119.868059426624,
119.927982276955,120.015835142529,120.103670102324,120.191508178203,120.279341089816,
120.367195651319,120.427118501645,120.514971367219,120.602806327013,120.690644402893,
120.778477314506,120.866331876008,120.926254726336,121.01410759191,121.101942551705,
121.189780627584,121.277613539197,121.365468100699,121.425390951027,121.513243816601,
121.601078776396,121.688916852275,121.776749763889,121.864604325391,121.924527175717,
122.012384664524,122.100222139734,122.188062354191,122.271017224399),
 .UNSPECIFIED.);
#359=B_SPLINE_CURVE_WITH_KNOTS('',3,(#29730,#29731,#29732,#29733,#29734,
#29735,#29736,#29737,#29738,#29739,#29740,#29741,#29742,#29743,#29744,#29745,
#29746,#29747,#29748,#29749,#29750,#29751,#29752,#29753,#29754,#29755,#29756,
#29757,#29758,#29759,#29760,#29761,#29762,#29763,#29764,#29765,#29766,#29767,
#29768,#29769,#29770,#29771,#29772,#29773,#29774,#29775,#29776,#29777,#29778,
#29779,#29780,#29781,#29782,#29783,#29784,#29785,#29786,#29787,#29788,#29789,
#29790,#29791,#29792,#29793,#29794,#29795,#29796,#29797,#29798,#29799,#29800,
#29801,#29802,#29803,#29804,#29805,#29806,#29807,#29808,#29809,#29810,#29811,
#29812,#29813,#29814,#29815,#29816,#29817,#29818,#29819,#29820,#29821,#29822,
#29823,#29824,#29825,#29826,#29827,#29828,#29829,#29830,#29831,#29832,#29833,
#29834,#29835,#29836,#29837,#29838,#29839,#29840,#29841,#29842,#29843,#29844,
#29845,#29846,#29847,#29848,#29849,#29850,#29851,#29852,#29853,#29854,#29855,
#29856,#29857,#29858,#29859,#29860,#29861,#29862,#29863,#29864,#29865,#29866,
#29867,#29868,#29869,#29870,#29871,#29872,#29873,#29874,#29875,#29876,#29877,
#29878,#29879,#29880,#29881,#29882,#29883,#29884,#29885,#29886,#29887,#29888,
#29889,#29890,#29891,#29892,#29893,#29894,#29895,#29896,#29897,#29898,#29899,
#29900,#29901,#29902,#29903,#29904,#29905,#29906,#29907,#29908,#29909,#29910,
#29911,#29912,#29913,#29914,#29915,#29916,#29917,#29918,#29919,#29920,#29921,
#29922,#29923,#29924,#29925,#29926,#29927,#29928,#29929,#29930,#29931,#29932,
#29933,#29934,#29935,#29936,#29937,#29938,#29939,#29940,#29941,#29942,#29943,
#29944,#29945,#29946,#29947,#29948,#29949,#29950,#29951,#29952,#29953,#29954,
#29955,#29956,#29957,#29958,#29959,#29960,#29961,#29962,#29963,#29964,#29965,
#29966,#29967,#29968,#29969,#29970,#29971,#29972,#29973,#29974,#29975,#29976,
#29977,#29978,#29979,#29980,#29981,#29982,#29983),.UNSPECIFIED.,.F.,.F.,
(4,2,2,2,2,2,2,2,2,2,2,2,2,2,2,2,2,2,2,2,2,2,2,2,2,2,2,2,2,2,2,2,2,2,2,
2,2,2,2,2,2,2,2,2,2,2,2,2,2,2,2,2,2,2,2,2,2,2,2,2,2,2,2,2,2,2,2,2,2,2,2,
2,2,2,2,2,2,2,2,2,2,2,2,2,2,2,2,2,2,2,2,2,2,2,2,2,2,2,2,2,2,2,2,2,2,2,2,
2,2,2,2,2,2,2,2,2,2,2,2,2,2,2,2,2,2,2,4),(-6.0676600479345,-6.06300156311093,
-6.05219138912275,-6.03403505117364,-5.9811424083886,-5.957374965299,-5.93848494184618,
-5.91894324672321,-5.88560449324608,-5.82977515111898,-5.82184467149748,
-5.81203068738065,-5.79950396495754,-5.76678865704346,-5.72458186220645,
-5.7039088418214,-5.68440742435925,-5.66955669263987,-5.62614474751871,
-5.59296482766278,-5.58292490633869,-5.57907136200978,-5.57653037666039,
-5.56664577247056,-5.55435211806181,-5.5296487941202,-5.48562302875605,
-5.46313071623149,-5.44422334845029,-5.42529021711367,-5.35898025850103,
-5.33868196785035,-5.33552159899471,-5.33357451185097,-5.33238166820454,
-5.33164915145285,-5.33119719676992,-5.33006187810181,-5.32022200351016,
-5.30754064128436,-5.2614552314717,-5.23030194993611,-5.21840552167871,
-5.19694943654444,-5.17785616100705,-5.14458295702549,-5.10432752555258,
-5.0882887724177,-5.07525703006934,-5.06469485173655,-5.04146253920956,
-4.98570215921476,-4.97356560109165,-4.95189370903324,-4.93295280603225,
-4.89408631268292,-4.85254758091093,-4.83436404014637,-4.82332165350525,
-4.80524318050571,-4.75225588562127,-4.72005109932547,-4.69965991241476,
-4.67526091300608,-4.61757937635378,-4.6048651217391,-4.58779211111111,
-4.57672729765341,-4.5573502049262,-4.50587958383057,-4.49075616524917,
-4.47927430982784,-4.45818069596309,-4.43590059997698,-4.38819747804384,
-4.34928134021141,-4.33690061662485,-4.32409950450634,-4.28702911913072,
-4.23648030027445,-4.21474189745155,-4.19324787879561,-4.14028149562153,
-4.10501446609073,-4.09203235253466,-4.07980032813057,-4.03211776649508,
-4.00116189355644,-3.97598938722291,-3.95569585114088,-3.92533453810172,
-3.87773444205573,-3.85396001940228,-3.8426434721844,-3.82761558442093,
-3.77926386810471,-3.74005958307201,-3.7192825551871,-3.6963588180046,-3.66530566220567,
-3.62834344211144,-3.61285045469689,-3.6001118404878,-3.58939525630702,
-3.56144954088596,-3.52357197159221,-3.49970923078575,-3.47782862160092,
-3.4590099697934,-3.39306302753264,-3.37841972958564,-3.35987348003764,
-3.34882833151189,-3.33108964336148,-3.27768677201668,-3.25385386610659,
-3.23198759311768,-3.21316118267848,-3.17165229713062,-3.13615376728696,
-3.12092036008069,-3.10832266253643,-3.09575311703086,-3.0562811115272,
-3.00733901118612,-2.98565146539759,-2.97204421563466),.UNSPECIFIED.);
#360=B_SPLINE_CURVE_WITH_KNOTS('',3,(#29985,#29986,#29987,#29988,#29989,
#29990,#29991,#29992,#29993,#29994,#29995,#29996,#29997),.UNSPECIFIED.,
 .F.,.F.,(4,3,3,3,4),(122.271017224399,122.358872260288,122.423663400408,
122.517081472137,122.522113490002),.UNSPECIFIED.);
#361=B_SPLINE_CURVE_WITH_KNOTS('',3,(#29998,#29999,#30000,#30001,#30002,
#30003,#30004,#30005,#30006,#30007,#30008,#30009,#30010,#30011,#30012,#30013),
 .UNSPECIFIED.,.F.,.F.,(4,1,1,1,1,1,1,1,1,1,1,1,1,4),(122.522113505659,
122.922799625098,123.421935849789,123.921072074479,124.42020829917,124.91934452386,
125.418480748551,125.917616973241,126.416753197932,126.915889422622,127.415025647313,
127.914161872003,128.413298096694,128.55424228146),.UNSPECIFIED.);
#362=B_SPLINE_CURVE_WITH_KNOTS('',3,(#30019,#30020,#30021,#30022,#30023,
#30024,#30025,#30026,#30027,#30028,#30029,#30030,#30031,#30032,#30033,#30034),
 .UNSPECIFIED.,.F.,.F.,(4,1,1,1,1,1,1,1,1,1,1,1,1,4),(128.805298812316,
129.032931173078,129.531803108226,130.030675043374,130.529546978522,131.02841891367,
131.527290848818,132.026162783967,132.525034719115,133.023906654263,133.522778589411,
134.021650524559,134.520522459707,134.837383691965),.UNSPECIFIED.);
#363=B_SPLINE_CURVE_WITH_KNOTS('',3,(#30035,#30036,#30037,#30038,#30039,
#30040,#30041,#30042,#30043,#30044,#30045,#30046),.UNSPECIFIED.,.F.,.F.,
(4,2,2,2,2,4),(-6.19136935571345,-6.17837183141341,-6.16428959311484,-6.1316433424487,
-6.07729914642043,-6.0676600479345),.UNSPECIFIED.);
#364=B_SPLINE_CURVE_WITH_KNOTS('',3,(#30048,#30049,#30050,#30051),
 .UNSPECIFIED.,.F.,.F.,(4,4),(128.55424228146,128.805298790277),
 .UNSPECIFIED.);
#365=B_SPLINE_CURVE_WITH_KNOTS('',3,(#30052,#30053,#30054,#30055,#30056,
#30057,#30058,#30059,#30060,#30061,#30062,#30063,#30064,#30065,#30066,#30067,
#30068,#30069,#30070,#30071,#30072,#30073,#30074,#30075,#30076,#30077,#30078,
#30079,#30080,#30081,#30082,#30083,#30084,#30085,#30086,#30087,#30088,#30089,
#30090,#30091,#30092,#30093,#30094,#30095,#30096,#30097,#30098,#30099,#30100,
#30101,#30102,#30103,#30104,#30105,#30106,#30107,#30108,#30109,#30110,#30111,
#30112,#30113,#30114,#30115,#30116,#30117,#30118,#30119,#30120,#30121,#30122,
#30123,#30124,#30125,#30126,#30127,#30128,#30129,#30130,#30131,#30132,#30133,
#30134,#30135,#30136,#30137,#30138,#30139,#30140,#30141,#30142,#30143,#30144,
#30145,#30146,#30147,#30148,#30149,#30150,#30151,#30152,#30153,#30154,#30155,
#30156,#30157,#30158,#30159,#30160,#30161,#30162,#30163,#30164,#30165,#30166,
#30167,#30168,#30169,#30170,#30171,#30172,#30173,#30174,#30175,#30176,#30177,
#30178,#30179,#30180,#30181,#30182,#30183,#30184,#30185,#30186,#30187,#30188,
#30189,#30190,#30191,#30192,#30193,#30194,#30195,#30196,#30197,#30198,#30199,
#30200,#30201,#30202,#30203,#30204,#30205,#30206,#30207,#30208,#30209,#30210,
#30211,#30212,#30213,#30214,#30215,#30216,#30217,#30218,#30219,#30220,#30221,
#30222,#30223,#30224,#30225,#30226,#30227,#30228,#30229,#30230,#30231,#30232,
#30233,#30234,#30235,#30236,#30237,#30238,#30239,#30240,#30241,#30242,#30243,
#30244,#30245,#30246,#30247,#30248,#30249,#30250,#30251,#30252,#30253,#30254,
#30255,#30256,#30257,#30258,#30259,#30260,#30261,#30262,#30263,#30264,#30265,
#30266,#30267,#30268,#30269,#30270,#30271),.UNSPECIFIED.,.F.,.F.,(4,3,3,
3,3,3,3,3,3,3,3,3,3,3,3,3,3,3,3,3,3,3,3,3,3,3,3,3,3,3,3,3,3,3,3,3,3,3,3,
3,3,3,3,3,3,3,3,3,3,3,3,3,3,3,3,3,3,3,3,3,3,3,3,3,3,3,3,3,3,3,3,3,3,4),
(128.805298797182,128.89834684814,128.912434321384,129.000287186958,129.088122146753,
129.175960222633,129.263793134246,129.351647695749,129.411570546075,129.499423411649,
129.587258371443,129.675096447323,129.762929358936,129.850783920438,129.910706770766,
129.99855963634,130.086394596135,130.174232672014,130.262065583628,130.34992014513,
130.409842995456,130.497695861029,130.585530820823,130.673368896702,130.761201808315,
130.849056369816,130.908979220147,130.996832085721,131.084667045516,131.172505121396,
131.260338033009,131.348192594512,131.408115444837,131.49596831041,131.583803270204,
131.671641346083,131.759474257696,131.847328819197,131.907251669528,131.995104535102,
132.082939494897,132.170777570777,132.25861048239,132.346465043893,132.406387894218,
132.494240759791,132.582075719585,132.669913795464,132.757746707077,132.845601268579,
132.905524118909,132.993376984483,133.081211944278,133.169050020158,133.256882931771,
133.344737493274,133.404660343599,133.492513209172,133.580348168967,133.668186244845,
133.756019156458,133.84387371796,133.90379656829,133.991649433864,134.079484393659,
134.167322469539,134.255155381152,134.343009942655,134.40293279298,134.490785003982,
134.578629290641,134.666460879314,134.754307286045,134.837387641181),
 .UNSPECIFIED.);
#366=B_SPLINE_CURVE_WITH_KNOTS('',3,(#30277,#30278,#30279,#30280,#30281,
#30282,#30283,#30284,#30285,#30286,#30287,#30288,#30289,#30290,#30291,#30292,
#30293,#30294,#30295,#30296,#30297,#30298,#30299,#30300,#30301,#30302,#30303,
#30304,#30305,#30306,#30307,#30308,#30309,#30310,#30311,#30312,#30313,#30314,
#30315,#30316,#30317,#30318,#30319,#30320,#30321,#30322,#30323,#30324,#30325,
#30326,#30327,#30328,#30329,#30330,#30331,#30332,#30333,#30334,#30335,#30336,
#30337,#30338,#30339,#30340,#30341,#30342,#30343,#30344,#30345,#30346,#30347,
#30348,#30349,#30350,#30351,#30352,#30353,#30354,#30355,#30356,#30357,#30358,
#30359,#30360,#30361,#30362,#30363,#30364,#30365,#30366,#30367,#30368,#30369,
#30370,#30371,#30372,#30373,#30374,#30375,#30376,#30377,#30378,#30379,#30380,
#30381,#30382,#30383,#30384,#30385,#30386,#30387,#30388,#30389,#30390,#30391,
#30392,#30393,#30394,#30395,#30396,#30397,#30398,#30399,#30400,#30401,#30402,
#30403,#30404,#30405,#30406,#30407,#30408,#30409,#30410,#30411,#30412,#30413,
#30414,#30415,#30416,#30417,#30418,#30419,#30420,#30421,#30422,#30423,#30424,
#30425,#30426,#30427,#30428,#30429,#30430,#30431,#30432,#30433,#30434,#30435,
#30436,#30437,#30438,#30439,#30440,#30441,#30442,#30443,#30444,#30445,#30446,
#30447,#30448,#30449,#30450,#30451,#30452,#30453,#30454,#30455,#30456,#30457,
#30458,#30459,#30460,#30461,#30462,#30463,#30464,#30465,#30466,#30467,#30468,
#30469,#30470,#30471,#30472,#30473,#30474,#30475,#30476,#30477,#30478,#30479,
#30480,#30481,#30482,#30483,#30484,#30485,#30486,#30487,#30488,#30489,#30490,
#30491,#30492,#30493,#30494,#30495,#30496),.UNSPECIFIED.,.F.,.F.,(4,3,3,
3,3,3,3,3,3,3,3,3,3,3,3,3,3,3,3,3,3,3,3,3,3,3,3,3,3,3,3,3,3,3,3,3,3,3,3,
3,3,3,3,3,3,3,3,3,3,3,3,3,3,3,3,3,3,3,3,3,3,3,3,3,3,3,3,3,3,3,3,3,3,4),
(135.088484109301,135.17598699825,135.263487430307,135.350979186156,135.438494599681,
135.518266330003,135.606120703016,135.693957195188,135.781796802318,135.869631257661,
135.957487308412,136.017138265152,136.104992638165,136.192829130337,136.280668737468,
136.368503192812,136.456359243563,136.5160102003,136.603864573313,136.691701065484,
136.779540672614,136.867375127957,136.955231178708,137.014882135448,137.102736508461,
137.190573000633,137.278412607763,137.366247063106,137.454103113857,137.513754070596,
137.601608443609,137.689444935781,137.777284542911,137.865118998254,137.952975049005,
138.012626005744,138.100480378757,138.188316870929,138.276156478059,138.363990933403,
138.451846984154,138.511497940892,138.599352313905,138.687188806077,138.775028413206,
138.86286286855,138.9507189193,139.01036987604,139.098224249053,139.186060741225,
139.273900348355,139.361734803699,139.44959085445,139.509241811188,139.597096184202,
139.684932676373,139.772772283503,139.860606738847,139.948462789598,140.008113746337,
140.095968119351,140.183804611522,140.271644218652,140.359478673996,140.447334724747,
140.506985681485,140.594840054498,140.682676546669,140.770516153799,140.858350609142,
140.946206659893,141.005857616633,141.093483641527,141.120602214731),
 .UNSPECIFIED.);
#367=B_SPLINE_CURVE_WITH_KNOTS('',3,(#30497,#30498,#30499,#30500,#30501),
 .UNSPECIFIED.,.F.,.F.,(4,1,4),(134.837383691965,135.019394394855,135.088484104361),
 .UNSPECIFIED.);
#368=B_SPLINE_CURVE_WITH_KNOTS('',3,(#30503,#30504,#30505,#30506,#30507,
#30508,#30509,#30510,#30511,#30512),.UNSPECIFIED.,.F.,.F.,(4,3,3,4),(134.837387641181,
134.902069017671,134.995276561016,135.088484104361),.UNSPECIFIED.);
#369=B_SPLINE_CURVE_WITH_KNOTS('',3,(#30513,#30514,#30515,#30516,#30517,
#30518,#30519,#30520,#30521,#30522,#30523,#30524,#30525,#30526,#30527,#30528,
#30529,#30530,#30531,#30532,#30533,#30534,#30535,#30536,#30537,#30538,#30539,
#30540,#30541,#30542,#30543,#30544,#30545,#30546,#30547,#30548,#30549,#30550,
#30551,#30552,#30553,#30554,#30555,#30556,#30557,#30558,#30559,#30560,#30561,
#30562,#30563,#30564,#30565,#30566,#30567,#30568,#30569,#30570,#30571,#30572,
#30573,#30574,#30575,#30576,#30577,#30578,#30579,#30580,#30581,#30582,#30583,
#30584,#30585,#30586,#30587,#30588,#30589,#30590,#30591,#30592,#30593,#30594,
#30595,#30596,#30597,#30598,#30599,#30600,#30601,#30602,#30603,#30604,#30605,
#30606,#30607,#30608,#30609,#30610,#30611,#30612,#30613,#30614,#30615,#30616,
#30617,#30618,#30619,#30620,#30621,#30622,#30623,#30624,#30625,#30626,#30627,
#30628,#30629,#30630,#30631,#30632,#30633,#30634,#30635,#30636,#30637,#30638,
#30639,#30640,#30641,#30642,#30643,#30644,#30645,#30646,#30647,#30648,#30649,
#30650,#30651,#30652,#30653,#30654,#30655,#30656,#30657,#30658,#30659,#30660,
#30661,#30662,#30663,#30664,#30665,#30666,#30667,#30668,#30669,#30670,#30671,
#30672,#30673,#30674,#30675,#30676,#30677,#30678,#30679,#30680,#30681,#30682,
#30683,#30684,#30685,#30686,#30687,#30688,#30689,#30690,#30691,#30692,#30693,
#30694,#30695,#30696,#30697,#30698,#30699,#30700,#30701,#30702,#30703,#30704,
#30705,#30706,#30707,#30708,#30709,#30710,#30711,#30712,#30713,#30714,#30715,
#30716,#30717,#30718,#30719,#30720,#30721,#30722,#30723,#30724,#30725,#30726,
#30727,#30728,#30729,#30730,#30731,#30732,#30733,#30734,#30735,#30736,#30737,
#30738,#30739,#30740,#30741,#30742,#30743,#30744,#30745,#30746,#30747,#30748,
#30749,#30750,#30751,#30752,#30753,#30754,#30755,#30756,#30757,#30758),
 .UNSPECIFIED.,.F.,.F.,(4,2,2,2,2,2,2,2,2,2,2,2,2,2,2,2,2,2,2,2,2,2,2,2,
2,2,2,2,2,2,2,2,2,2,2,2,2,2,2,2,2,2,2,2,2,2,2,2,2,2,2,2,2,2,2,2,2,2,2,2,
2,2,2,2,2,2,2,2,2,2,2,2,2,2,2,2,2,2,2,2,2,2,2,2,2,2,2,2,2,2,2,2,2,2,2,2,
2,2,2,2,2,2,2,2,2,2,2,2,2,2,2,2,2,2,2,2,2,2,2,2,2,2,4),(-6.19116494302175,
-6.17703734950308,-6.1642332800254,-6.14380755584216,-6.10914123558922,
-6.05622377563799,-6.04286629535891,-6.03234035590157,-6.01553011095014,
-5.96572983886545,-5.93993559338612,-5.92069483504914,-5.91137080832514,
-5.89411263056373,-5.83723919301332,-5.81279712282643,-5.80555977645213,
-5.79247970631615,-5.79143790586598,-5.77887172285572,-5.75072147711475,
-5.70913847348934,-5.68695422494636,-5.66748676667828,-5.64903922621219,
-5.58356864396798,-5.56338254532162,-5.56088440472294,-5.55928667875535,
-5.55823444449872,-5.55752193230004,-5.55702784204972,-5.54582465351428,
-5.53510838929563,-5.48047347045303,-5.45195674899915,-5.43226314035227,
-5.41650800972621,-5.39213794921603,-5.33402503226821,-5.3156560429689,
-5.31464792868625,-5.31385702723433,-5.31323124398406,-5.30004351817591,
-5.28772132550516,-5.25555507480882,-5.22422777874082,-5.19983214911048,
-5.17761075762797,-5.15866866544375,-5.12229318038202,-5.08286654308721,
-5.06093895062442,-5.04965501464434,-5.03394581732045,-4.98479788555917,
-4.95793185388434,-4.93453184105898,-4.91387810287515,-4.87763843878035,
-4.87327177306261,-4.82703692882799,-4.81119233634939,-4.79987746975932,
-4.78258871437243,-4.73202313732268,-4.7077680272941,-4.6856139534971,-4.66406961199734,
-4.60683893170405,-4.58289912767763,-4.57478799775961,-4.56190224715054,
-4.54933147062396,-4.51660691591032,-4.46832616088545,-4.44416483231003,
-4.42348211844725,-4.38905651192622,-4.34631926662311,-4.32985397789693,
-4.31656819753484,-4.30594248383866,-4.28270749976801,-4.22672921524457,
-4.21454257038949,-4.19273345571192,-4.17355271186985,-4.11536233632143,
-4.09122701256364,-4.07433804594037,-4.06313680873221,-4.04340516322852,
-3.99241158015077,-3.96879773026077,-3.94694950494545,-3.92779502187308,
-3.88016358396155,-3.84944531309101,-3.83009312768414,-3.81892651988141,
-3.80135407367478,-3.74869432044514,-3.72433193807619,-3.70212643137315,
-3.68062105142192,-3.6261521734276,-3.59139947631689,-3.57841366511148,
-3.56593028739867,-3.52291716201066,-3.47629038964963,-3.45459983301622,
-3.43533310475785,-3.40079251087165,-3.36147349575419,-3.33957378120327,
-3.32829141674859,-3.31257031538694,-3.26341318653884,-3.23655984982501,
-3.21935699787793),.UNSPECIFIED.);
#370=B_SPLINE_CURVE_WITH_KNOTS('',3,(#30764,#30765,#30766,#30767,#30768,
#30769,#30770,#30771,#30772,#30773,#30774,#30775,#30776,#30777,#30778,#30779),
 .UNSPECIFIED.,.F.,.F.,(4,1,1,1,1,1,1,1,1,1,1,1,1,4),(141.371669425729,
141.504729551781,142.003601486929,142.502473422077,143.001345357225,143.500217292373,
143.999089227522,144.49796116267,144.996833097818,145.495705032966,145.994576968114,
146.493448903262,146.99232083841,147.403749232517),.UNSPECIFIED.);
#371=B_SPLINE_CURVE_WITH_KNOTS('',3,(#30780,#30781,#30782,#30783,#30784,
#30785,#30786,#30787,#30788,#30789),.UNSPECIFIED.,.F.,.F.,(4,3,3,4),(141.120602214731,
141.208209304607,141.295822961552,141.371669411541),.UNSPECIFIED.);
#372=B_SPLINE_CURVE_WITH_KNOTS('',3,(#30790,#30791,#30792,#30793,#30794,
#30795,#30796,#30797,#30798,#30799,#30800,#30801,#30802,#30803,#30804,#30805,
#30806,#30807,#30808,#30809,#30810,#30811,#30812,#30813,#30814,#30815,#30816,
#30817,#30818,#30819,#30820,#30821,#30822,#30823,#30824,#30825,#30826,#30827,
#30828,#30829,#30830,#30831,#30832,#30833,#30834,#30835,#30836,#30837,#30838,
#30839,#30840,#30841,#30842,#30843,#30844,#30845,#30846,#30847,#30848,#30849,
#30850,#30851,#30852,#30853,#30854,#30855,#30856,#30857,#30858,#30859,#30860,
#30861,#30862,#30863,#30864,#30865,#30866,#30867,#30868,#30869,#30870,#30871,
#30872,#30873,#30874,#30875,#30876,#30877,#30878,#30879,#30880,#30881,#30882,
#30883,#30884,#30885,#30886,#30887,#30888,#30889,#30890,#30891,#30892,#30893,
#30894,#30895,#30896,#30897,#30898,#30899,#30900,#30901,#30902,#30903,#30904,
#30905,#30906,#30907,#30908,#30909,#30910,#30911,#30912,#30913,#30914,#30915,
#30916,#30917,#30918,#30919,#30920,#30921,#30922,#30923,#30924,#30925,#30926,
#30927,#30928,#30929,#30930,#30931,#30932,#30933,#30934,#30935,#30936,#30937,
#30938,#30939,#30940,#30941,#30942,#30943,#30944,#30945,#30946,#30947,#30948,
#30949,#30950,#30951,#30952,#30953,#30954,#30955,#30956,#30957,#30958,#30959,
#30960,#30961,#30962,#30963,#30964,#30965,#30966,#30967,#30968,#30969,#30970,
#30971,#30972,#30973,#30974,#30975,#30976,#30977,#30978,#30979,#30980,#30981,
#30982,#30983,#30984,#30985,#30986,#30987,#30988,#30989,#30990,#30991,#30992,
#30993,#30994,#30995,#30996,#30997,#30998,#30999,#31000,#31001,#31002,#31003,
#31004,#31005,#31006,#31007,#31008,#31009,#31010,#31011,#31012,#31013,#31014,
#31015,#31016,#31017,#31018,#31019,#31020,#31021,#31022,#31023,#31024,#31025,
#31026,#31027,#31028,#31029,#31030,#31031,#31032,#31033,#31034,#31035,#31036,
#31037),.UNSPECIFIED.,.F.,.F.,(4,2,2,2,2,2,2,2,2,2,2,2,2,2,2,2,2,2,2,2,
2,2,2,2,2,2,2,2,2,2,2,2,2,2,2,2,2,2,2,2,2,2,2,2,2,2,2,2,2,2,2,2,2,2,2,2,
2,2,2,2,2,2,2,2,2,2,2,2,2,2,2,2,2,2,2,2,2,2,2,2,2,2,2,2,2,2,2,2,2,2,2,2,
2,2,2,2,2,2,2,2,2,2,2,2,2,2,2,2,2,2,2,2,2,2,2,2,2,2,2,2,2,2,2,4),(-3.21935699787793,
-3.21316574382707,-3.19250989034801,-3.12355310177051,-3.09563748505854,
-3.08510027142359,-3.07160316901746,-3.05473506422643,-3.00917199984596,
-2.97710495108727,-2.95655385603739,-2.93164162185956,-2.86234423940217,
-2.84524819467226,-2.83407987182315,-2.81466375467055,-2.7837549282786,
-2.73647812724851,-2.71731400536239,-2.6954801539321,-2.6518927399594,-2.61669784915749,
-2.59945486001201,-2.58829144305401,-2.56907356360656,-2.53875182401622,
-2.49038352427511,-2.47125139413836,-2.44936880460065,-2.42568237233774,
-2.37415174452258,-2.35468710802651,-2.34351742839056,-2.32603112372484,
-2.2805418421437,-2.24355865422078,-2.22457294543408,-2.20243767323222,
-2.17822174496133,-2.11590501654389,-2.10292696087652,-2.09043678634569,
-2.08270985379705,-2.03723873670129,-1.99764336815913,-1.97865723782612,
-1.95652242097001,-1.93230757697079,-1.87143333557131,-1.85784458764912,
-1.8457888581465,-1.80665611724896,-1.75274959080811,-1.73359806255764,
-1.71174459709267,-1.66793522467079,-1.63617314630175,-1.61685525028106,
-1.60568933672935,-1.58808956392394,-1.56219243683647,-1.50845526340811,
-1.48687994314329,-1.46476418569153,-1.44058927319633,-1.38896356972876,
-1.37044976025338,-1.35929571259066,-1.3409940267418,-1.3132533887721,-1.27213519698725,
-1.24773067096726,-1.2270967831308,-1.19353998525343,-1.13523365967798,
-1.12094698710776,-1.10922956394915,-1.08033236632137,-1.01293362655361,
-0.992227825167441,-0.968978051344675,-0.936899162881563,-0.885268327354135,
-0.872704649199791,-0.862767793654905,-0.86162103217559,-0.861281487285616,
-0.860726587094819,-0.859815351734257,-0.858312056532366,-0.855830139949326,
-0.836649112705669,-0.771835850106395,-0.752167074879882,-0.732844513280138,
-0.711249010258384,-0.672985890047654,-0.666222628819701,-0.637110847403014,
-0.626420749717713,-0.616414869848926,-0.613899412979933,-0.610412801638719,
-0.603823332220953,-0.577022026661718,-0.523311490345541,-0.510886707762487,
-0.490772954721622,-0.470351614673873,-0.412358250096588,-0.390247685735212,
-0.378734878019143,-0.368321278159657,-0.353343782086913,-0.317910129570223,
-0.278198157293771,-0.257791049881306,-0.238679495714611,-0.216170129610846,
-0.172642003635443,-0.157979298938959,-0.140305586474041,-0.129627005635082,
-0.123748402156024),.UNSPECIFIED.);
#373=B_SPLINE_CURVE_WITH_KNOTS('',3,(#31043,#31044,#31045,#31046,#31047,
#31048,#31049,#31050,#31051,#31052,#31053,#31054,#31055,#31056,#31057,#31058,
#31059,#31060,#31061,#31062,#31063,#31064,#31065,#31066,#31067,#31068,#31069,
#31070,#31071,#31072,#31073,#31074,#31075,#31076,#31077,#31078,#31079,#31080,
#31081,#31082,#31083,#31084,#31085,#31086,#31087,#31088,#31089,#31090,#31091,
#31092,#31093,#31094,#31095,#31096,#31097,#31098,#31099,#31100,#31101,#31102,
#31103,#31104,#31105,#31106,#31107,#31108,#31109,#31110,#31111,#31112,#31113,
#31114,#31115,#31116,#31117,#31118,#31119,#31120,#31121,#31122,#31123,#31124,
#31125,#31126,#31127,#31128,#31129,#31130,#31131,#31132,#31133,#31134,#31135,
#31136,#31137,#31138,#31139,#31140,#31141,#31142,#31143,#31144,#31145,#31146,
#31147,#31148,#31149,#31150,#31151,#31152,#31153,#31154,#31155,#31156,#31157,
#31158,#31159,#31160,#31161,#31162,#31163,#31164,#31165,#31166,#31167,#31168,
#31169,#31170,#31171,#31172,#31173,#31174,#31175,#31176,#31177,#31178,#31179,
#31180,#31181,#31182,#31183,#31184,#31185,#31186,#31187,#31188,#31189,#31190,
#31191,#31192,#31193,#31194,#31195,#31196,#31197,#31198,#31199,#31200,#31201,
#31202,#31203,#31204,#31205,#31206,#31207,#31208,#31209,#31210,#31211,#31212,
#31213,#31214,#31215,#31216,#31217,#31218,#31219,#31220,#31221,#31222,#31223,
#31224,#31225,#31226,#31227,#31228,#31229,#31230,#31231,#31232,#31233,#31234,
#31235,#31236,#31237,#31238,#31239,#31240,#31241,#31242,#31243,#31244,#31245,
#31246,#31247,#31248,#31249,#31250,#31251,#31252,#31253,#31254,#31255,#31256,
#31257,#31258,#31259,#31260,#31261,#31262,#31263,#31264,#31265,#31266,#31267,
#31268,#31269,#31270,#31271,#31272,#31273,#31274,#31275,#31276,#31277,#31278,
#31279,#31280,#31281,#31282,#31283,#31284,#31285,#31286,#31287,#31288,#31289,
#31290,#31291,#31292,#31293,#31294,#31295,#31296,#31297,#31298),
 .UNSPECIFIED.,.F.,.F.,(4,2,2,2,2,2,2,2,2,2,2,2,2,2,2,2,2,2,2,2,2,2,2,2,
2,2,2,2,2,2,2,2,2,2,2,2,2,2,2,2,2,2,2,2,2,2,2,2,2,2,2,2,2,2,2,2,2,2,2,2,
2,2,2,2,2,2,2,2,2,2,2,2,2,2,2,2,2,2,2,2,2,2,2,2,2,2,2,2,2,2,2,2,2,2,2,2,
2,2,2,2,2,2,2,2,2,2,2,2,2,2,2,2,2,2,2,2,2,2,2,2,2,2,2,2,2,2,2,4),(-2.97188626525704,
-2.96975074164106,-2.9263303559528,-2.88990303366061,-2.87340634195713,
-2.86233267829574,-2.84269920478538,-2.81100941469992,-2.76533127746046,
-2.7462707140118,-2.7247728406981,-2.6765192930133,-2.635386131538,-2.62287443420638,
-2.61021777327762,-2.59487609980264,-2.55877206357895,-2.53991360842078,
-2.51140177136903,-2.49117954246924,-2.46488356337848,-2.4312244043192,
-2.38954215043325,-2.37705869051714,-2.36437210188408,-2.35642422903556,
-2.31047195879666,-2.27275279109622,-2.25386565246452,-2.23210769488765,
-2.18782021780113,-2.14331501979756,-2.13099759075805,-2.11812258910905,
-2.10999229723689,-2.06358956611743,-2.0266939900833,-2.00785075623836,
-1.98601646118949,-1.96224927075858,-1.90936226198506,-1.89119909313463,
-1.88015696730535,-1.86205912518019,-1.82066704256834,-1.80127060929152,
-1.7734238141848,-1.75321472726857,-1.72638425432589,-1.69136378590274,
-1.65258557915946,-1.63995611764576,-1.62741821724914,-1.61961341288586,
-1.60795796824994,-1.56088506667449,-1.5301409185966,-1.50982903714417,
-1.48484084014843,-1.45430943591898,-1.4049907147059,-1.39415840059693,
-1.38160812315362,-1.34299207442822,-1.29674465774136,-1.27409066376061,
-1.2531973919192,-1.21119472270484,-1.16091106314901,-1.14832539592815,
-1.13574428661718,-1.09577025043834,-1.04753389025392,-1.02580548884736,
-1.0043031330915,-0.992354621862678,-0.954467592238873,-0.915158450992807,
-0.902562234097002,-0.889991637216024,-0.889367716728599,-0.888687303470545,
-0.887941651527501,-0.887710854495311,-0.887415376257045,-0.887035506880723,
-0.869489228676335,-0.818248354178469,-0.790352965228216,-0.77074926593518,
-0.747423812408836,-0.71682537905745,-0.667618776287439,-0.656794343839576,
-0.64596645841836,-0.644924376966577,-0.643727768686432,-0.642324942176007,
-0.641667930139639,-0.640624694724322,-0.638933502496702,-0.619148211900778,
-0.552477596556398,-0.535420404979643,-0.516704037292846,-0.495277012953636,
-0.457382904592064,-0.447636955771573,-0.437768710568182,-0.419477416066318,
-0.408204860698465,-0.393885593098416,-0.383789411424907,-0.349783964485769,
-0.307044322047352,-0.286357470563327,-0.283096889067452,-0.259892285100198,
-0.232620374462148,-0.183926660325592,-0.168550369124722,-0.157585914554883,
-0.137157497631893,-0.0798175246746923,-0.0524557511181905,-0.0336832247805891,
-0.0185010444887893,-4.22433275936514E-5),.UNSPECIFIED.);
#374=B_SPLINE_CURVE_WITH_KNOTS('',3,(#31299,#31300,#31301,#31302,#31303),
 .UNSPECIFIED.,.F.,.F.,(4,1,4),(147.403749232517,147.491192773558,147.65485471872),
 .UNSPECIFIED.);
#375=B_SPLINE_CURVE_WITH_KNOTS('',3,(#31305,#31306,#31307,#31308,#31309,
#31310,#31311,#31312,#31313,#31314,#31315,#31316),.UNSPECIFIED.,.F.,.F.,
(4,2,2,2,2,4),(-0.123748402156024,-0.114490652887485,-0.060891536213952,
-0.0277646115254283,-0.0134254131229336,-4.23462887881731E-5),
 .UNSPECIFIED.);
#376=B_SPLINE_CURVE_WITH_KNOTS('',3,(#31317,#31318,#31319,#31320,#31321,
#31322,#31323,#31324,#31325,#31326,#31327,#31328,#31329,#31330,#31331,#31332),
 .UNSPECIFIED.,.F.,.F.,(4,1,1,1,1,1,1,1,1,1,1,1,1,4),(147.65485471872,147.879610859624,
148.378747084315,148.877883309006,149.377019533696,149.876155758387,150.375291983077,
150.874428207768,151.373564432458,151.872700657149,152.371836881839,152.87097310653,
153.37010933122,153.686939606376),.UNSPECIFIED.);
#377=B_SPLINE_CURVE_WITH_KNOTS('',3,(#31337,#31338,#31339,#31340,#31341,
#31342,#31343,#31344,#31345,#31346,#31347,#31348,#31349,#31350,#31351,#31352,
#31353,#31354,#31355,#31356,#31357,#31358,#31359,#31360,#31361,#31362,#31363,
#31364,#31365,#31366,#31367,#31368,#31369,#31370,#31371,#31372,#31373,#31374,
#31375,#31376,#31377,#31378,#31379,#31380,#31381,#31382,#31383,#31384,#31385,
#31386,#31387,#31388,#31389,#31390,#31391,#31392,#31393,#31394,#31395,#31396,
#31397,#31398,#31399,#31400,#31401,#31402,#31403,#31404,#31405,#31406,#31407,
#31408,#31409,#31410,#31411,#31412,#31413,#31414,#31415,#31416,#31417,#31418,
#31419,#31420,#31421,#31422,#31423,#31424,#31425,#31426,#31427,#31428,#31429,
#31430,#31431,#31432,#31433,#31434,#31435,#31436,#31437,#31438,#31439,#31440,
#31441,#31442,#31443,#31444,#31445,#31446,#31447,#31448,#31449,#31450,#31451,
#31452,#31453,#31454,#31455,#31456,#31457,#31458,#31459,#31460,#31461,#31462,
#31463,#31464,#31465,#31466,#31467,#31468,#31469,#31470,#31471,#31472,#31473,
#31474,#31475,#31476,#31477,#31478,#31479,#31480,#31481,#31482,#31483,#31484,
#31485,#31486,#31487,#31488,#31489,#31490,#31491,#31492,#31493,#31494,#31495,
#31496,#31497,#31498,#31499,#31500,#31501,#31502,#31503,#31504,#31505,#31506,
#31507,#31508,#31509,#31510,#31511,#31512,#31513,#31514,#31515,#31516,#31517,
#31518,#31519,#31520,#31521,#31522,#31523,#31524,#31525,#31526,#31527,#31528,
#31529,#31530,#31531,#31532,#31533,#31534,#31535,#31536,#31537,#31538,#31539,
#31540,#31541,#31542,#31543,#31544,#31545,#31546,#31547,#31548,#31549,#31550,
#31551,#31552,#31553,#31554,#31555,#31556,#31557,#31558,#31559,#31560,#31561,
#31562,#31563,#31564,#31565,#31566,#31567,#31568,#31569,#31570,#31571,#31572,
#31573,#31574,#31575,#31576,#31577,#31578),.UNSPECIFIED.,.F.,.F.,(4,2,2,
2,2,2,2,2,2,2,2,2,2,2,2,2,2,2,2,2,2,2,2,2,2,2,2,2,2,2,2,2,2,2,2,2,2,2,2,
2,2,2,2,2,2,2,2,2,2,2,2,2,2,2,2,2,2,2,2,2,2,2,2,2,2,2,2,2,2,2,2,2,2,2,2,
2,2,2,2,2,2,2,2,2,2,2,2,2,2,2,2,2,2,2,2,2,2,2,2,2,2,2,2,2,2,2,2,2,2,2,2,
2,2,2,2,2,2,2,2,2,4),(-6.06742144176788,-6.06407799162494,-6.05160770778557,
-6.00076330556691,-5.96719222778308,-5.94807689102041,-5.92856945746908,
-5.8995703315435,-5.85057997654442,-5.82899710278286,-5.81902806230131,
-5.80696228986996,-5.78027118837979,-5.73710895416591,-5.71475719531442,
-5.69583550374847,-5.67549401984022,-5.60968635942604,-5.58652077754147,
-5.58175358782967,-5.57180900202197,-5.55887911052905,-5.49637904783472,
-5.47238928580918,-5.45348687153915,-5.43324397326591,-5.39950525275359,
-5.35704058862313,-5.34277395591618,-5.33828548945826,-5.33648887758617,
-5.32666830212619,-5.31416580357581,-5.2728557190283,-5.22483935773843,
-5.2033237088039,-5.18160982529904,-5.13311289189205,-5.10490957464148,
-5.08647600539771,-5.07543234408859,-5.0575923385754,-5.0075628445441,-4.97321891374844,
-4.95270352679775,-4.92893719400904,-4.88640619473629,-4.84749304142301,
-4.83493609505112,-4.82410817003078,-4.77484054846688,-4.7442803950602,
-4.71927959715428,-4.69896904205886,-4.6682523192502,-4.62113809750946,
-4.60947772126166,-4.60167077129116,-4.58913075191011,-4.57829168340389,
-4.52891485914777,-4.49842542666809,-4.4734554650417,-4.45314155836037,
-4.42235805441496,-4.37533382143012,-4.36368350125133,-4.355880850752,-4.34334529813755,
-4.33071340349779,-4.29197294521198,-4.25693850532766,-4.23010269341009,
-4.20989366375154,-4.18205297665057,-4.16264237328303,-4.12124487055019,
-4.10314752183386,-4.09210538235301,-4.07394167222515,-4.02105879477338,
-3.99729280885844,-3.9754589213058,-3.95661537453561,-3.9197173040692,-3.87331234729695,
-3.86518189673572,-3.85230683702556,-3.8399894035144,-3.79548819927903,
-3.75120170888419,-3.72944395152908,-3.71055657791946,-3.67147810328407,
-3.63454558328402,-3.61333364709922,-3.60218240890063,-3.58653869013744,
-3.53749442901179,-3.51071528190879,-3.48743555124862,-3.46701994167282,
-3.43088401605884,-3.39020056885571,-3.37409474727358,-3.3610273876202,
-3.3488603697357,-3.31192271235755,-3.28450178674414,-3.26047044114872,
-3.23850887037474,-3.21973274028817,-3.18374031448609,-3.14406523957616,
-3.12212052596242,-3.11092497889359,-3.09559144875588,-3.05049171530733,
-3.01297771107997,-2.99143257034414,-2.97188626525704),.UNSPECIFIED.);
#378=B_SPLINE_CURVE_WITH_KNOTS('',3,(#31580,#31581,#31582,#31583,#31584),
 .UNSPECIFIED.,.F.,.F.,(4,1,4),(153.686939606376,153.869245555911,153.9380400259),
 .UNSPECIFIED.);
#379=B_SPLINE_CURVE_WITH_KNOTS('',3,(#31585,#31586,#31587,#31588,#31589,
#31590,#31591,#31592,#31593,#31594,#31595,#31596,#31597,#31598,#31599,#31600,
#31601,#31602,#31603,#31604,#31605,#31606,#31607,#31608,#31609,#31610,#31611,
#31612,#31613,#31614,#31615,#31616,#31617,#31618,#31619,#31620,#31621,#31622,
#31623,#31624,#31625,#31626,#31627,#31628,#31629,#31630,#31631,#31632,#31633,
#31634,#31635,#31636,#31637,#31638,#31639,#31640,#31641,#31642,#31643,#31644,
#31645,#31646,#31647,#31648,#31649,#31650,#31651,#31652,#31653,#31654,#31655,
#31656,#31657,#31658,#31659,#31660,#31661,#31662,#31663,#31664,#31665,#31666,
#31667,#31668,#31669,#31670,#31671,#31672,#31673,#31674,#31675,#31676,#31677,
#31678,#31679,#31680,#31681,#31682,#31683,#31684,#31685,#31686,#31687,#31688,
#31689,#31690,#31691,#31692,#31693,#31694,#31695,#31696,#31697,#31698,#31699,
#31700,#31701,#31702,#31703,#31704,#31705,#31706,#31707,#31708,#31709,#31710,
#31711,#31712,#31713,#31714,#31715,#31716,#31717,#31718,#31719,#31720,#31721,
#31722,#31723,#31724,#31725,#31726,#31727,#31728,#31729,#31730,#31731,#31732,
#31733,#31734,#31735,#31736,#31737,#31738,#31739,#31740,#31741,#31742,#31743,
#31744,#31745,#31746,#31747,#31748,#31749,#31750,#31751,#31752,#31753,#31754,
#31755,#31756,#31757,#31758,#31759,#31760,#31761,#31762,#31763,#31764,#31765,
#31766,#31767,#31768,#31769,#31770,#31771,#31772,#31773,#31774,#31775,#31776,
#31777,#31778,#31779,#31780,#31781,#31782,#31783,#31784,#31785,#31786,#31787,
#31788,#31789,#31790,#31791,#31792,#31793,#31794,#31795,#31796,#31797,#31798,
#31799,#31800,#31801,#31802,#31803,#31804,#31805,#31806,#31807,#31808,#31809,
#31810,#31811,#31812),.UNSPECIFIED.,.F.,.F.,(4,2,2,2,2,2,2,2,2,2,2,2,2,
2,2,2,2,2,2,2,2,2,2,2,2,2,2,2,2,2,2,2,2,2,2,2,2,2,2,2,2,2,2,2,2,2,2,2,2,
2,2,2,2,2,2,2,2,2,2,2,2,2,2,2,2,2,2,2,2,2,2,2,2,2,2,2,2,2,2,2,2,2,2,2,2,
2,2,2,2,2,2,2,2,2,2,2,2,2,2,2,2,2,2,2,2,2,2,2,2,2,2,2,2,4),(-6.19115773559391,
-6.13978402677965,-6.11845966752513,-6.0990275018796,-6.07606680140882,
-5.99291711066576,-5.98007377883281,-5.96801237580815,-5.91817766023449,
-5.88788156212622,-5.86342350784108,-5.86107494362402,-5.85703378075258,
-5.83803868019293,-5.80089496545136,-5.76722987174831,-5.74916122623811,
-5.73519303373494,-5.72354786405738,-5.70060780934709,-5.65388679229046,
-5.63087959595418,-5.61074360855692,-5.59432516089233,-5.55844565038033,
-5.51730921859077,-5.50108613413929,-5.48927295805451,-5.48042478322879,
-5.45976688528121,-5.40954548881871,-5.37821958006577,-5.36485326481983,
-5.3621062805176,-5.33949053368747,-5.30630023981983,-5.26967850719128,
-5.25419972746558,-5.24144121841607,-5.22875057949216,-5.18232796356464,
-5.13985381781297,-5.11811868250635,-5.09888515542233,-5.0406312342978,
-5.01670475292962,-5.00859637825522,-4.9957134100255,-4.98313981773564,
-4.94183385068555,-4.89354733171623,-4.87189944529077,-4.84987193614447,
-4.80456775304053,-4.7746441834212,-4.75556279944509,-4.74440222291625,
-4.72661143052049,-4.67310928877592,-4.64916731580293,-4.62716283816976,
-4.60810515271709,-4.56814577675448,-4.53182291078504,-4.51639688490346,
-4.50366698173267,-4.49094816097923,-4.45235122521209,-4.40442178382397,
-4.38211951728747,-4.36068373226232,-4.32663673283387,-4.28716620084722,
-4.26522711649107,-4.2539424061385,-4.23823778546967,-4.18909294237154,
-4.16222147721896,-4.13881880088144,-4.11816565297058,-4.08057407705395,
-4.02470911137608,-4.01192803929309,-4.00103621165331,-3.95160490125583,
-3.92098364477319,-3.90916136641944,-3.88767507509096,-3.86544363208039,
-3.81681490595078,-3.78948868881414,-3.77134135945358,-3.76018651101403,
-3.74151061919928,-3.68907599710731,-3.6652714035854,-3.64333247501297,
-3.6242358333334,-3.56534626076997,-3.54132426486435,-3.53319589924436,
-3.52029236352149,-3.50773736955315,-3.47501829531416,-3.42674253917791,
-3.40256175490641,-3.38188306686002,-3.34753095942292,-3.30470944677134,
-3.28823161662024,-3.27493919060774,-3.2626926804812,-3.22565993154105,
-3.21930413045193),.UNSPECIFIED.);
#380=B_SPLINE_CURVE_WITH_KNOTS('',3,(#31818,#31819,#31820,#31821,#31822,
#31823,#31824,#31825,#31826,#31827,#31828,#31829,#31830,#31831,#31832,#31833,
#31834,#31835,#31836,#31837,#31838,#31839,#31840,#31841,#31842,#31843,#31844,
#31845,#31846,#31847,#31848,#31849,#31850,#31851,#31852,#31853,#31854,#31855,
#31856,#31857,#31858,#31859,#31860,#31861,#31862,#31863,#31864,#31865,#31866,
#31867,#31868,#31869,#31870,#31871,#31872,#31873,#31874,#31875,#31876,#31877,
#31878,#31879,#31880,#31881,#31882,#31883,#31884,#31885,#31886,#31887,#31888,
#31889,#31890,#31891,#31892,#31893,#31894,#31895,#31896,#31897,#31898,#31899,
#31900,#31901,#31902,#31903,#31904,#31905,#31906,#31907,#31908,#31909,#31910,
#31911,#31912,#31913,#31914,#31915,#31916,#31917,#31918,#31919,#31920,#31921,
#31922,#31923,#31924,#31925,#31926,#31927,#31928,#31929,#31930,#31931,#31932,
#31933,#31934,#31935,#31936,#31937,#31938,#31939,#31940,#31941,#31942,#31943,
#31944,#31945,#31946,#31947,#31948,#31949,#31950,#31951,#31952,#31953,#31954,
#31955,#31956,#31957,#31958,#31959,#31960,#31961,#31962,#31963,#31964,#31965,
#31966,#31967,#31968,#31969,#31970,#31971,#31972,#31973,#31974,#31975,#31976,
#31977,#31978,#31979,#31980,#31981,#31982,#31983,#31984,#31985,#31986,#31987,
#31988,#31989,#31990,#31991,#31992,#31993,#31994,#31995,#31996,#31997,#31998,
#31999,#32000,#32001,#32002,#32003,#32004,#32005,#32006,#32007,#32008,#32009,
#32010,#32011,#32012,#32013,#32014,#32015,#32016,#32017,#32018,#32019,#32020,
#32021,#32022,#32023,#32024,#32025,#32026,#32027,#32028,#32029,#32030,#32031,
#32032,#32033,#32034,#32035,#32036,#32037),.UNSPECIFIED.,.F.,.F.,(4,3,3,
3,3,3,3,3,3,3,3,3,3,3,3,3,3,3,3,3,3,3,3,3,3,3,3,3,3,3,3,3,3,3,3,3,3,3,3,
3,3,3,3,3,3,3,3,3,3,3,3,3,3,3,3,3,3,3,3,3,3,3,3,3,3,3,3,3,3,3,3,3,3,4),
(160.22122533308,160.310313635352,160.399431796454,160.46186308741,160.549717460423,
160.637553952595,160.725393559725,160.813228015068,160.901084065819,160.960735022558,
161.048589395571,161.136425887743,161.224265494873,161.312099950217,161.399956000968,
161.459606957706,161.547461330719,161.635297822891,161.723137430021,161.810971885365,
161.898827936115,161.958478892854,162.046333265867,162.134169758039,162.222009365169,
162.309843820512,162.397699871263,162.457350828002,162.545205201015,162.633041693186,
162.720881300316,162.80871575566,162.89657180641,162.95622276315,163.044077136164,
163.131913628335,163.219753235466,163.307587690809,163.395443741561,163.455094698298,
163.542949071311,163.630785563483,163.718625170613,163.806459625957,163.894315676708,
163.953966633447,164.041821006461,164.129657498632,164.217497105763,164.305331561106,
164.393187611858,164.452838568595,164.540692941608,164.628529433779,164.716369040909,
164.804203496252,164.892059547003,164.951710503743,165.039564876756,165.127401368928,
165.215240976058,165.303075431401,165.390931482152,165.450582438891,165.538436811904,
165.626273304076,165.714112911206,165.801947366549,165.8898034173,165.949454374039,
166.037310852933,166.125147748629,166.212980689828,166.253319805291),
 .UNSPECIFIED.);
#381=B_SPLINE_CURVE_WITH_KNOTS('',3,(#32038,#32039,#32040,#32041,#32042,
#32043,#32044,#32045,#32046,#32047,#32048,#32049),.UNSPECIFIED.,.F.,.F.,
(4,2,2,2,2,4),(-6.19113417191044,-6.17867666764163,-6.16455856974076,-6.10126357361464,
-6.07390768735744,-6.06742144176788),.UNSPECIFIED.);
#382=B_SPLINE_CURVE_WITH_KNOTS('',3,(#32050,#32051,#32052,#32053,#32054,
#32055,#32056,#32057,#32058,#32059,#32060,#32061,#32062,#32063,#32064,#32065,
#32066,#32067,#32068,#32069,#32070,#32071,#32072,#32073,#32074,#32075,#32076,
#32077,#32078,#32079,#32080,#32081,#32082,#32083,#32084,#32085,#32086,#32087,
#32088,#32089,#32090,#32091,#32092,#32093,#32094,#32095,#32096,#32097,#32098,
#32099,#32100,#32101,#32102,#32103,#32104,#32105,#32106,#32107,#32108,#32109,
#32110,#32111,#32112,#32113,#32114,#32115,#32116,#32117,#32118,#32119,#32120,
#32121,#32122,#32123,#32124,#32125,#32126,#32127,#32128,#32129,#32130,#32131,
#32132,#32133,#32134,#32135,#32136,#32137,#32138,#32139,#32140,#32141,#32142,
#32143,#32144,#32145,#32146,#32147,#32148,#32149,#32150,#32151,#32152,#32153,
#32154,#32155,#32156,#32157,#32158,#32159,#32160,#32161,#32162,#32163,#32164,
#32165,#32166,#32167,#32168,#32169,#32170,#32171,#32172,#32173,#32174,#32175,
#32176,#32177,#32178,#32179,#32180,#32181,#32182,#32183,#32184,#32185,#32186,
#32187,#32188,#32189,#32190,#32191,#32192,#32193,#32194,#32195,#32196,#32197,
#32198,#32199,#32200,#32201,#32202,#32203,#32204,#32205,#32206,#32207,#32208,
#32209,#32210,#32211,#32212,#32213,#32214,#32215,#32216,#32217,#32218,#32219,
#32220,#32221,#32222,#32223,#32224,#32225,#32226,#32227,#32228,#32229,#32230,
#32231,#32232,#32233,#32234,#32235,#32236,#32237,#32238,#32239,#32240,#32241,
#32242,#32243,#32244,#32245,#32246,#32247,#32248,#32249,#32250,#32251,#32252,
#32253,#32254,#32255,#32256,#32257,#32258,#32259,#32260,#32261,#32262,#32263,
#32264,#32265,#32266,#32267,#32268,#32269,#32270,#32271,#32272,#32273,#32274,
#32275,#32276,#32277,#32278,#32279,#32280,#32281,#32282,#32283,#32284,#32285,
#32286,#32287,#32288,#32289,#32290,#32291),.UNSPECIFIED.,.F.,.F.,(4,2,2,
2,2,2,2,2,2,2,2,2,2,2,2,2,2,2,2,2,2,2,2,2,2,2,2,2,2,2,2,2,2,2,2,2,2,2,2,
2,2,2,2,2,2,2,2,2,2,2,2,2,2,2,2,2,2,2,2,2,2,2,2,2,2,2,2,2,2,2,2,2,2,2,2,
2,2,2,2,2,2,2,2,2,2,2,2,2,2,2,2,2,2,2,2,2,2,2,2,2,2,2,2,2,2,2,2,2,2,2,2,
2,2,2,2,2,2,2,2,2,4),(-3.21930413045193,-3.19821895702288,-3.1740881861233,
-3.1519934702773,-3.1329861388801,-3.09559741316757,-3.04683547256862,-3.03143132293309,
-3.02120633601416,-3.00026928727761,-2.96446516427597,-2.93768636476454,
-2.91244968626192,-2.89213357025697,-2.86111608945007,-2.81330751301519,
-2.79133621896855,-2.77988541746673,-2.76526543280403,-2.74617026192556,
-2.69184569051622,-2.66658055460417,-2.64626772712302,-2.61531223093145,
-2.56773633213867,-2.54556295825083,-2.53408142612529,-2.51955946629205,
-2.46641694638413,-2.43300380847211,-2.41376926903898,-2.39203579458847,
-2.37993361341199,-2.32203045081919,-2.29996395133401,-2.28941826765291,
-2.27594253337349,-2.2591154343958,-2.21384971782128,-2.18154667171162,
-2.16098281960491,-2.13616004489249,-2.12154549557563,-2.06937050746921,
-2.05046942519298,-2.03931198757433,-2.02136752202807,-2.00758778652186,
-1.93815840565377,-1.91751807187727,-1.89407566259905,-1.86609039132995,
-1.81731372016487,-1.801893056179,-1.79167104624693,-1.77077235955525,-1.73510062345755,
-1.69357588818809,-1.67461739439505,-1.65242889811755,-1.62810177210808,
-1.57594166010619,-1.55801231759893,-1.5468545775697,-1.52793599538702,
-1.49848062143119,-1.45228775512562,-1.43030118330118,-1.40861791109259,
-1.3572671430483,-1.31987151883562,-1.30702725153194,-1.29441828303544,
-1.28657514925565,-1.27486898677441,-1.22755557403127,-1.19682110045702,
-1.17633679789597,-1.15083804491047,-1.1193016169689,-1.0753713497353,-1.06194408206572,
-1.04978857394223,-1.0103349893949,-0.959570909841802,-0.93779757711804,
-0.91590899529176,-0.871692638480005,-0.826795365771362,-0.814428911222402,
-0.80524774805795,-0.791748796936568,-0.764859027120126,-0.71174609356172,
-0.690751040529247,-0.670654640740498,-0.666798279841583,-0.64132396660455,
-0.591359115583464,-0.574164225752605,-0.568787224730732,-0.557576671645744,
-0.542983964486431,-0.511066242008585,-0.465564162968799,-0.444623014070843,
-0.430780768429424,-0.39612072132774,-0.346037043878999,-0.328319812056502,
-0.325871641634217,-0.32377308942613,-0.321547822994558,-0.316047485152077,
-0.295953959524207,-0.261702867484532,-0.218977449536296,-0.198162881597824,
-0.179620600092242,-0.128417530992846,-0.123769554268864),.UNSPECIFIED.);
#383=B_SPLINE_CURVE_WITH_KNOTS('',3,(#32297,#32298,#32299,#32300,#32301,
#32302,#32303,#32304,#32305,#32306,#32307,#32308,#32309,#32310,#32311,#32312),
 .UNSPECIFIED.,.F.,.F.,(4,1,1,1,1,1,1,1,1,1,1,1,1,4),(166.504410682989,
166.947198244335,167.446070179483,167.944942114632,168.44381404978,168.942685984928,
169.441557920076,169.940429855224,170.439301790372,170.93817372552,171.437045660668,
171.935917595817,172.434789530965,172.536539600894),.UNSPECIFIED.);
#384=B_SPLINE_CURVE_WITH_KNOTS('',3,(#32313,#32314,#32315,#32316,#32317,
#32318,#32319,#32320,#32321,#32322,#32323,#32324,#32325),.UNSPECIFIED.,
 .F.,.F.,(4,3,3,3,4),(166.253319805291,166.341154624617,166.429008307032,
166.448326309187,166.504410640259),.UNSPECIFIED.);
#385=B_SPLINE_CURVE_WITH_KNOTS('',3,(#32327,#32328,#32329,#32330,#32331,
#32332,#32333,#32334,#32335,#32336,#32337,#32338),.UNSPECIFIED.,.F.,.F.,
(4,2,2,2,2,4),(-0.123769554268864,-0.0900669150748557,-0.0773253769985558,
-0.0674267057802843,-0.0538731003174174,-7.62332589639553E-5),
 .UNSPECIFIED.);
#386=B_SPLINE_CURVE_WITH_KNOTS('',3,(#32339,#32340,#32341,#32342,#32343,
#32344,#32345,#32346,#32347,#32348,#32349,#32350,#32351,#32352,#32353,#32354,
#32355,#32356,#32357,#32358,#32359,#32360,#32361,#32362,#32363,#32364,#32365,
#32366,#32367,#32368,#32369,#32370,#32371,#32372,#32373,#32374,#32375,#32376,
#32377,#32378,#32379,#32380,#32381,#32382,#32383,#32384,#32385,#32386,#32387,
#32388,#32389,#32390,#32391,#32392,#32393,#32394,#32395,#32396,#32397,#32398,
#32399,#32400,#32401,#32402,#32403,#32404,#32405,#32406,#32407,#32408,#32409,
#32410,#32411,#32412,#32413,#32414,#32415,#32416,#32417,#32418,#32419,#32420,
#32421,#32422,#32423,#32424,#32425,#32426,#32427,#32428,#32429,#32430,#32431,
#32432,#32433,#32434,#32435,#32436,#32437,#32438,#32439,#32440,#32441,#32442,
#32443,#32444,#32445,#32446,#32447,#32448,#32449,#32450,#32451,#32452,#32453,
#32454,#32455,#32456,#32457,#32458,#32459,#32460,#32461,#32462,#32463,#32464,
#32465,#32466,#32467,#32468,#32469,#32470,#32471,#32472,#32473,#32474,#32475,
#32476,#32477,#32478,#32479,#32480,#32481,#32482,#32483,#32484,#32485,#32486,
#32487,#32488,#32489,#32490,#32491,#32492,#32493,#32494,#32495,#32496,#32497,
#32498,#32499,#32500,#32501,#32502,#32503,#32504,#32505,#32506,#32507,#32508,
#32509,#32510,#32511,#32512,#32513,#32514,#32515,#32516,#32517,#32518,#32519,
#32520,#32521,#32522,#32523,#32524,#32525,#32526,#32527,#32528,#32529,#32530,
#32531,#32532,#32533,#32534,#32535,#32536,#32537,#32538,#32539,#32540,#32541,
#32542,#32543,#32544,#32545,#32546,#32547,#32548,#32549,#32550,#32551,#32552,
#32553,#32554,#32555,#32556,#32557,#32558,#32559,#32560,#32561,#32562,#32563,
#32564,#32565,#32566,#32567,#32568,#32569,#32570,#32571,#32572,#32573,#32574,
#32575,#32576,#32577,#32578,#32579,#32580,#32581,#32582,#32583,#32584,#32585,
#32586,#32587,#32588,#32589,#32590,#32591,#32592,#32593,#32594,#32595,#32596,
#32597,#32598),.UNSPECIFIED.,.F.,.F.,(4,2,2,2,2,2,2,2,2,2,2,2,2,2,2,2,2,
2,2,2,2,2,2,2,2,2,2,2,2,2,2,2,2,2,2,2,2,2,2,2,2,2,2,2,2,2,2,2,2,2,2,2,2,
2,2,2,2,2,2,2,2,2,2,2,2,2,2,2,2,2,2,2,2,2,2,2,2,2,2,2,2,2,2,2,2,2,2,2,2,
2,2,2,2,2,2,2,2,2,2,2,2,2,2,2,2,2,2,2,2,2,2,2,2,2,2,2,2,2,2,2,2,2,2,2,2,
2,2,2,2,4),(-6.1913800756723,-6.17067857718631,-6.15416759396204,-6.13512852001715,
-6.10714964374355,-6.04949551586851,-6.03016362183847,-6.01891967319071,
-6.00326796720119,-5.9541618387972,-5.92723006119227,-5.9041552920683,-5.90175032429661,
-5.88091883462017,-5.82232469085236,-5.79816404507313,-5.79259327439422,
-5.78840635509426,-5.77651128602982,-5.76362237081052,-5.72658443180081,
-5.69074538006163,-5.66960789853106,-5.65123335961385,-5.62847837269773,
-5.56646749327657,-5.54762456604348,-5.54638106722991,-5.54560174635282,
-5.54414922599148,-5.54291199349935,-5.54183560207732,-5.5408773061103,
-5.54000233814295,-5.53918073069057,-5.53838420729294,-5.53758236675965,
-5.53673646997048,-5.53578598822348,-5.53424078005765,-5.52991557134065,
-5.52547020566476,-5.50737944103455,-5.45424216161364,-5.4303460820723,
-5.41043944490215,-5.39131931290488,-5.39024351151347,-5.38856761065132,
-5.34888773452981,-5.31293204660583,-5.29195093702676,-5.2817224014293,
-5.26633671237753,-5.21759302961125,-5.19016622191713,-5.16650270514723,
-5.14592661328751,-5.10977215236485,-5.06892497233756,-5.05274646572066,
-5.03961231014794,-5.02891469557269,-5.00815101840954,-4.94965303077316,
-4.93753247773549,-4.91578209106171,-4.89386788213271,-4.84622927994932,
-4.8056498008151,-4.79298812978226,-4.78019886188033,-4.74232040976024,
-4.69119755090187,-4.66953995633978,-4.64752228027722,-4.60197564536534,
-4.5721788437998,-4.55314101734022,-4.54198091638866,-4.52415253447887,
-4.47069445505799,-4.44675754364414,-4.42475514701808,-4.40569524574346,
-4.36567533494732,-4.32940011302846,-4.31398225156481,-4.30125663949336,
-4.29032934966841,-4.26252823900804,-4.21151367579109,-4.1994718185711,
-4.17779162477969,-4.15580010543284,-4.10968485517058,-4.06805641973549,
-4.05533418150158,-4.04260688149864,-4.01564954458518,-4.00940163958921,
-3.96100578953942,-3.93719704781849,-3.91642765587057,-3.88046774871173,
-3.83941443783963,-3.82320390186537,-3.81005273822562,-3.79770180725745,
-3.76135166735944,-3.71256196703528,-3.68957869611001,-3.66876907117997,
-3.60481092107409,-3.57358766112734,-3.56175491713929,-3.54773833002112,
-3.48902368787403,-3.46438518463211,-3.44204691870484,-3.42063479565248,
-3.36393472581923,-3.33931306298977,-3.33106022321823,-3.31802873891789,
-3.30558273082634,-3.27667549062873,-3.23535869043582,-3.22158689325656,
-3.21942130955984),.UNSPECIFIED.);
#387=B_SPLINE_CURVE_WITH_KNOTS('',3,(#32604,#32605,#32606,#32607,#32608,
#32609,#32610,#32611,#32612,#32613,#32614,#32615,#32616,#32617,#32618,#32619,
#32620,#32621,#32622,#32623,#32624,#32625,#32626,#32627,#32628,#32629,#32630,
#32631,#32632,#32633,#32634,#32635,#32636,#32637,#32638,#32639,#32640,#32641,
#32642,#32643,#32644,#32645,#32646,#32647,#32648,#32649,#32650,#32651,#32652,
#32653,#32654,#32655,#32656,#32657,#32658,#32659,#32660,#32661,#32662,#32663,
#32664,#32665,#32666,#32667,#32668,#32669,#32670,#32671,#32672,#32673,#32674,
#32675,#32676,#32677,#32678,#32679,#32680,#32681,#32682,#32683,#32684,#32685,
#32686,#32687,#32688,#32689,#32690,#32691,#32692,#32693,#32694,#32695,#32696,
#32697,#32698,#32699,#32700,#32701,#32702,#32703,#32704,#32705,#32706,#32707,
#32708,#32709,#32710,#32711,#32712,#32713,#32714,#32715,#32716,#32717,#32718,
#32719,#32720,#32721,#32722,#32723,#32724,#32725,#32726,#32727,#32728,#32729,
#32730,#32731,#32732,#32733,#32734,#32735,#32736,#32737,#32738,#32739,#32740,
#32741,#32742,#32743,#32744,#32745,#32746,#32747,#32748,#32749,#32750,#32751,
#32752,#32753,#32754,#32755,#32756,#32757,#32758,#32759,#32760,#32761,#32762,
#32763,#32764,#32765,#32766,#32767,#32768,#32769,#32770,#32771,#32772,#32773,
#32774,#32775,#32776,#32777,#32778,#32779,#32780,#32781,#32782,#32783,#32784,
#32785,#32786,#32787,#32788,#32789,#32790,#32791,#32792,#32793,#32794,#32795,
#32796,#32797,#32798,#32799,#32800,#32801,#32802,#32803,#32804,#32805,#32806,
#32807,#32808,#32809,#32810,#32811,#32812,#32813,#32814,#32815,#32816,#32817,
#32818,#32819,#32820,#32821,#32822,#32823),.UNSPECIFIED.,.F.,.F.,(4,2,2,
2,2,2,2,2,2,2,2,2,2,2,2,2,2,2,2,2,2,2,2,2,2,2,2,2,2,2,2,2,2,2,2,2,2,2,2,
2,2,2,2,2,2,2,2,2,2,2,2,2,2,2,2,2,2,2,2,2,2,2,2,2,2,2,2,2,2,2,2,2,2,2,2,
2,2,2,2,2,2,2,2,2,2,2,2,2,2,2,2,2,2,2,2,2,2,2,2,2,2,2,2,2,2,2,2,2,2,4),
(-2.97195484317244,-2.91662865217212,-2.89779221698913,-2.87594479156734,
-2.85215060598283,-2.79905544977423,-2.78106326611344,-2.77002065265098,
-2.7517486240445,-2.73748038139496,-2.66972738674698,-2.6491998397412,-2.62625341290914,
-2.59390865768494,-2.54197864914045,-2.52956362206813,-2.51680173438993,
-2.50878119052095,-2.46264847549782,-2.42524660827217,-2.40637878873055,
-2.38458711743793,-2.36090899197926,-2.30871011669473,-2.28996549946835,
-2.27891731577259,-2.26135111404435,-2.23544820546775,-2.18200971160627,
-2.16056977046165,-2.1387703544922,-2.11507608882696,-2.06275361780042,
-2.04411467823821,-2.03306830190307,-2.01541151946985,-1.9728240407116,
-1.93950174847006,-1.91725144382443,-1.89613997842978,-1.84770133637917,
-1.80460126619897,-1.79219587904024,-1.77942312916082,-1.77139207655314,
-1.72523337505143,-1.68788293721545,-1.66901702230384,-1.64722202762939,
-1.62353698445096,-1.57128523117997,-1.55258587518402,-1.54153849804936,
-1.52393379733011,-1.48166566028458,-1.46176028522242,-1.43418643718348,
-1.41397977858964,-1.38690224658569,-1.35123440070221,-1.31401172667698,
-1.30122886059127,-1.28883238235635,-1.24607249403879,-1.20074254928594,
-1.17886479364796,-1.15749005008917,-1.10922404672469,-1.06745082707563,
-1.05497192320139,-1.04228006357283,-1.00206336059066,-0.954507144778013,
-0.932740322302675,-0.911271940373778,-0.899361565372025,-0.843774282387121,
-0.819627100938718,-0.807903970736283,-0.794527822711242,-0.777573886003473,
-0.73102092646425,-0.699886005324059,-0.681165044986464,-0.657655465997681,
-0.629931284744476,-0.574054015278958,-0.563335241104719,-0.552329466851587,
-0.538041984434196,-0.507398355324752,-0.459860792167081,-0.439130301418296,
-0.428613625985288,-0.400430174505115,-0.360037447653399,-0.329402162777094,
-0.317179450594455,-0.314098720290468,-0.301074285541704,-0.282409168565291,
-0.221416972947329,-0.198456539095972,-0.181117596885108,-0.151828055013685,
-0.106403764995796,-0.082256284976266,-0.0705396952843348,-0.060451715834582,
-4.22977414189134E-5),.UNSPECIFIED.);
#388=B_SPLINE_CURVE_WITH_KNOTS('',3,(#32824,#32825,#32826,#32827),
 .UNSPECIFIED.,.F.,.F.,(4,4),(172.536539600894,172.787595947439),
 .UNSPECIFIED.);
#389=B_SPLINE_CURVE_WITH_KNOTS('',3,(#32828,#32829,#32830,#32831,#32832,
#32833,#32834,#32835,#32836,#32837,#32838,#32839,#32840,#32841,#32842,#32843,
#32844,#32845,#32846,#32847,#32848,#32849,#32850,#32851,#32852,#32853,#32854,
#32855,#32856,#32857,#32858,#32859,#32860,#32861,#32862,#32863,#32864,#32865,
#32866,#32867,#32868,#32869,#32870,#32871,#32872,#32873,#32874,#32875,#32876,
#32877,#32878,#32879,#32880,#32881,#32882,#32883,#32884,#32885,#32886,#32887,
#32888,#32889,#32890,#32891,#32892,#32893,#32894,#32895,#32896,#32897,#32898,
#32899,#32900,#32901,#32902,#32903,#32904,#32905,#32906,#32907,#32908,#32909,
#32910,#32911,#32912,#32913,#32914,#32915,#32916,#32917,#32918,#32919,#32920,
#32921,#32922,#32923,#32924,#32925,#32926,#32927,#32928,#32929,#32930,#32931,
#32932,#32933,#32934,#32935,#32936,#32937,#32938,#32939,#32940,#32941,#32942,
#32943,#32944,#32945,#32946,#32947,#32948,#32949,#32950,#32951,#32952,#32953,
#32954,#32955,#32956,#32957,#32958,#32959,#32960,#32961,#32962,#32963,#32964,
#32965,#32966,#32967,#32968,#32969,#32970,#32971,#32972,#32973,#32974,#32975,
#32976,#32977,#32978,#32979,#32980,#32981,#32982,#32983,#32984,#32985,#32986,
#32987,#32988,#32989,#32990,#32991,#32992,#32993,#32994,#32995,#32996,#32997,
#32998,#32999,#33000,#33001,#33002,#33003,#33004,#33005,#33006,#33007,#33008,
#33009,#33010,#33011,#33012,#33013,#33014,#33015,#33016,#33017,#33018,#33019,
#33020,#33021,#33022,#33023,#33024,#33025,#33026,#33027,#33028,#33029,#33030,
#33031,#33032,#33033,#33034,#33035,#33036,#33037,#33038,#33039,#33040,#33041,
#33042,#33043,#33044,#33045,#33046,#33047,#33048,#33049,#33050,#33051,#33052,
#33053,#33054,#33055,#33056,#33057,#33058,#33059,#33060,#33061,#33062,#33063,
#33064,#33065),.UNSPECIFIED.,.F.,.F.,(4,2,2,2,2,2,2,2,2,2,2,2,2,2,2,2,2,
2,2,2,2,2,2,2,2,2,2,2,2,2,2,2,2,2,2,2,2,2,2,2,2,2,2,2,2,2,2,2,2,2,2,2,2,
2,2,2,2,2,2,2,2,2,2,2,2,2,2,2,2,2,2,2,2,2,2,2,2,2,2,2,2,2,2,2,2,2,2,2,2,
2,2,2,2,2,2,2,2,2,2,2,2,2,2,2,2,2,2,2,2,2,2,2,2,2,2,2,2,2,4),(-3.21942130955984,
-3.19833034902414,-3.17762650184267,-3.11014558210518,-3.09569482555007,
-3.07724916805604,-3.06609500473019,-3.04772563408401,-3.03337871304127,
-2.96560766923414,-2.94491326891506,-2.92162994646329,-2.89501200012371,
-2.83721000537578,-2.82493793371155,-2.81168045364214,-2.79526946799109,
-2.7528974110563,-2.71852469058027,-2.69777890558541,-2.6738800190411,-2.62551292942305,
-2.59292091621499,-2.58003781907883,-2.5674635852813,-2.55965443733128,
-2.51294691049226,-2.47503133312629,-2.45602321221816,-2.43392820613057,
-2.40979720657546,-2.38235965182285,-2.34530555043866,-2.33306108011966,
-2.31976479713902,-2.30328023260175,-2.26041272529873,-2.22610225845176,
-2.20542538814414,-2.18123232240695,-2.13295540228018,-2.10023758091653,
-2.08769067776905,-2.07477717223001,-2.06663937837715,-2.04257261261481,
-1.99812205184573,-1.97287079271416,-1.95240375822785,-1.92206771980915,
-1.8767425879191,-1.8525526563831,-1.84175021003303,-1.82881587347761,-1.82065782583839,
-1.77411730159096,-1.73715011494937,-1.7181649032282,-1.69602695193314,
-1.67180607480177,-1.62033308541774,-1.6018051179295,-1.59065081345178,
-1.57236217177524,-1.55812441006771,-1.4900405960124,-1.46935626724098,
-1.44604437067114,-1.41528159096145,-1.361537654392,-1.34932643446531,-1.33598224872465,
-1.31940661575981,-1.27591647674414,-1.24524050748075,-1.22626532657779,
-1.20410813625716,-1.17984700049751,-1.129196340505,-1.11023378431642,-1.09907506196553,
-1.08118283430355,-1.03344588593146,-1.00061233862785,-0.981429639534398,
-0.959621818298641,-0.91488093336989,-0.870203057459326,-0.857821549539762,
-0.847825809514792,-0.83385618869784,-0.80489481561337,-0.757722448334184,
-0.736150077867063,-0.716967031380558,-0.694876289140778,-0.653843929106904,
-0.624085478754477,-0.611777995185696,-0.601755623568807,-0.587685246213096,
-0.558263117562371,-0.512003339023885,-0.490384880343963,-0.471190597845841,
-0.449150973801902,-0.408412683162301,-0.378046386433222,-0.365784706658776,
-0.355744957157113,-0.341609329660175,-0.311885359069004,-0.26620747556139,
-0.24456176447186,-0.225360727470203,-0.203350675080102,-0.162781426989361,
-0.132226410056128,-0.123804338336763),.UNSPECIFIED.);
#390=B_SPLINE_CURVE_WITH_KNOTS('',3,(#33070,#33071,#33072,#33073,#33074,
#33075,#33076,#33077,#33078,#33079,#33080,#33081,#33082,#33083,#33084,#33085,
#33086,#33087,#33088,#33089,#33090,#33091,#33092,#33093,#33094,#33095,#33096,
#33097,#33098,#33099,#33100,#33101,#33102,#33103,#33104,#33105,#33106,#33107,
#33108,#33109,#33110,#33111,#33112,#33113,#33114,#33115,#33116,#33117,#33118,
#33119,#33120,#33121,#33122,#33123,#33124,#33125,#33126,#33127,#33128,#33129,
#33130,#33131,#33132,#33133,#33134,#33135,#33136,#33137,#33138,#33139,#33140,
#33141,#33142,#33143,#33144,#33145,#33146,#33147,#33148,#33149,#33150,#33151,
#33152,#33153,#33154,#33155,#33156,#33157,#33158,#33159,#33160,#33161,#33162,
#33163,#33164,#33165,#33166,#33167,#33168,#33169,#33170,#33171,#33172,#33173,
#33174,#33175,#33176,#33177,#33178,#33179,#33180,#33181,#33182,#33183,#33184,
#33185,#33186,#33187,#33188,#33189,#33190,#33191,#33192,#33193,#33194,#33195,
#33196,#33197,#33198,#33199,#33200,#33201,#33202,#33203,#33204,#33205,#33206,
#33207,#33208,#33209,#33210,#33211,#33212,#33213,#33214,#33215,#33216,#33217,
#33218,#33219,#33220,#33221,#33222,#33223,#33224,#33225,#33226,#33227,#33228,
#33229,#33230,#33231,#33232,#33233,#33234,#33235,#33236,#33237,#33238,#33239,
#33240,#33241,#33242,#33243,#33244,#33245,#33246,#33247,#33248,#33249,#33250,
#33251,#33252,#33253,#33254,#33255,#33256,#33257,#33258,#33259,#33260,#33261,
#33262,#33263,#33264,#33265,#33266,#33267,#33268,#33269,#33270,#33271,#33272,
#33273,#33274,#33275,#33276,#33277,#33278,#33279,#33280,#33281,#33282,#33283,
#33284,#33285,#33286,#33287,#33288,#33289,#33290,#33291,#33292,#33293,#33294,
#33295,#33296,#33297,#33298,#33299,#33300,#33301,#33302,#33303,#33304,#33305,
#33306,#33307,#33308,#33309,#33310,#33311,#33312,#33313,#33314,#33315),
 .UNSPECIFIED.,.F.,.F.,(4,2,2,2,2,2,2,2,2,2,2,2,2,2,2,2,2,2,2,2,2,2,2,2,
2,2,2,2,2,2,2,2,2,2,2,2,2,2,2,2,2,2,2,2,2,2,2,2,2,2,2,2,2,2,2,2,2,2,2,2,
2,2,2,2,2,2,2,2,2,2,2,2,2,2,2,2,2,2,2,2,2,2,2,2,2,2,2,2,2,2,2,2,2,2,2,2,
2,2,2,2,2,2,2,2,2,2,2,2,2,2,2,2,2,2,2,2,2,2,2,2,2,2,4),(-6.06755362652627,
-6.05425213686216,-5.9830849064687,-5.97100646247755,-5.95853702788697,
-5.91659712697962,-5.88305907004699,-5.85702045100482,-5.84855013099762,
-5.82969106017962,-5.7924834923253,-5.75408554743836,-5.73834870448597,
-5.73452601656187,-5.72349912521049,-5.7097978339891,-5.65078453704456,
-5.62619702201709,-5.6066925109695,-5.58652066833823,-5.55160551748355,
-5.50960878495049,-5.49330134107481,-5.49187061051971,-5.49063994836124,
-5.48955783087141,-5.4798368380119,-5.46771796605209,-5.43677943629094,
-5.39653843997406,-5.37468534001023,-5.35780925693728,-5.35364812642821,
-5.35148633634693,-5.34972684243515,-5.32507578582433,-5.2850888196536,
-5.24601825658349,-5.23345793716701,-5.22263263999495,-5.17340527152829,
-5.13194098576691,-5.1103917655996,-5.09136874074132,-5.03288512778012,
-5.00899166129382,-5.00090619171659,-4.98807745525644,-4.97572097278534,
-4.91136805628013,-4.88751284202727,-4.86563608459446,-4.84426115498006,
-4.78778877308601,-4.76349354303907,-4.75532434027678,-4.74240946153522,
-4.73178958167123,-4.70808231781952,-4.66228049337883,-4.63189861927627,
-4.61160464059256,-4.5864433476347,-4.53224368943837,-4.5188754785911,-4.50128533226249,
-4.49023781017001,-4.47152197139837,-4.41929397560244,-4.39561291713768,
-4.37381979560172,-4.35495310812868,-4.31758174580036,-4.27143105421713,
-4.26340383082188,-4.25063520083035,-4.23822640838169,-4.19519250236425,
-4.14862933391866,-4.12711898315795,-4.10539947610897,-4.05523825915691,
-4.02808240191872,-4.01003595941011,-3.99899371405451,-3.98077824729366,
-3.92795755726902,-3.9041995660234,-3.8823695079746,-3.86352379150114,-3.82572158929199,
-3.77969221120906,-3.76315172386917,-3.7520543681746,-3.73246730981183,
-3.70172711863458,-3.65794559996691,-3.63623187939583,-3.61471603975411,
-3.56193593522228,-3.53583988310811,-3.51819846644601,-3.5071518829171,
-3.48849548200209,-3.4369094832764,-3.41297573958261,-3.39106111371404,
-3.36971608113663,-3.30554325202029,-3.29119801646875,-3.27286929933081,
-3.26182644329393,-3.24388854271475,-3.19073131063413,-3.16692998891198,
-3.14507904537909,-3.12624470346781,-3.09565257879225,-3.03654123665552,
-3.02289998470606,-3.01108952204565,-2.97861413531433,-2.97195484317244),
 .UNSPECIFIED.);
#391=B_SPLINE_CURVE_WITH_KNOTS('',3,(#33317,#33318,#33319,#33320,#33321,
#33322,#33323,#33324,#33325,#33326,#33327,#33328),.UNSPECIFIED.,.F.,.F.,
(4,2,2,2,2,4),(-0.123804338336763,-0.119935359050831,-0.109906915523079,
-0.0958135679357499,-0.0198720624599457,-8.03630370901633E-5),
 .UNSPECIFIED.);
#392=B_SPLINE_CURVE_WITH_KNOTS('',3,(#33329,#33330,#33331,#33332,#33333,
#33334,#33335,#33336,#33337,#33338,#33339,#33340,#33341,#33342,#33343,#33344),
 .UNSPECIFIED.,.F.,.F.,(4,1,1,1,1,1,1,1,1,1,1,1,1,4),(179.070781254618,
179.325193015128,179.824329239818,180.323465464509,180.822601689199,181.32173791389,
181.82087413858,182.320010363271,182.819146587961,183.318282812652,183.817419037342,
184.316555262033,184.815691486723,185.102873615134),.UNSPECIFIED.);
#393=B_SPLINE_CURVE_WITH_KNOTS('',3,(#33347,#33348,#33349,#33350,#33351),
 .UNSPECIFIED.,.F.,.F.,(4,1,4),(185.102873615134,185.314827711414,185.353966561798),
 .UNSPECIFIED.);
#394=B_SPLINE_CURVE_WITH_KNOTS('',3,(#33353,#33354,#33355,#33356,#33357,
#33358,#33359,#33360,#33361,#33362,#33363,#33364,#33365,#33366,#33367,#33368,
#33369,#33370,#33371,#33372,#33373,#33374,#33375,#33376,#33377,#33378,#33379,
#33380,#33381,#33382,#33383,#33384,#33385,#33386,#33387,#33388,#33389,#33390,
#33391,#33392,#33393,#33394,#33395,#33396,#33397,#33398,#33399,#33400,#33401,
#33402,#33403,#33404,#33405,#33406,#33407,#33408,#33409,#33410,#33411,#33412,
#33413,#33414,#33415,#33416,#33417,#33418,#33419,#33420,#33421,#33422,#33423,
#33424,#33425,#33426,#33427,#33428,#33429,#33430,#33431,#33432,#33433,#33434,
#33435,#33436,#33437,#33438,#33439,#33440,#33441,#33442,#33443,#33444,#33445,
#33446,#33447,#33448,#33449,#33450,#33451,#33452,#33453,#33454,#33455,#33456,
#33457,#33458,#33459,#33460,#33461,#33462,#33463,#33464,#33465,#33466,#33467,
#33468,#33469,#33470,#33471,#33472,#33473,#33474,#33475,#33476,#33477,#33478,
#33479,#33480,#33481,#33482,#33483,#33484,#33485,#33486,#33487,#33488,#33489,
#33490,#33491,#33492,#33493,#33494,#33495,#33496,#33497,#33498,#33499,#33500,
#33501,#33502,#33503,#33504,#33505,#33506,#33507,#33508,#33509,#33510,#33511,
#33512,#33513,#33514,#33515,#33516,#33517,#33518,#33519,#33520,#33521,#33522,
#33523,#33524,#33525,#33526,#33527,#33528,#33529,#33530,#33531,#33532,#33533,
#33534,#33535,#33536,#33537,#33538,#33539,#33540,#33541,#33542,#33543,#33544,
#33545,#33546,#33547,#33548,#33549,#33550,#33551,#33552,#33553,#33554,#33555,
#33556,#33557,#33558,#33559,#33560,#33561,#33562,#33563),.UNSPECIFIED.,
 .F.,.F.,(4,3,3,3,3,3,3,3,3,3,3,3,3,3,3,3,3,3,3,3,3,3,3,3,3,3,3,3,3,3,3,
3,3,3,3,3,3,3,3,3,3,3,3,3,3,3,3,3,3,3,3,3,3,3,3,3,3,3,3,3,3,3,3,3,3,3,3,
3,3,3,4),(185.353966567087,185.441561764946,185.529139524043,185.616720093993,
185.704298367222,185.791896369604,185.813963936104,185.901816358879,185.989650873403,
186.077488504696,186.165320973144,186.25317509779,186.313100160795,186.400954277281,
186.488790493292,186.576629820951,186.664463978937,186.75231976687,186.812236385486,
186.900086650938,186.987919001855,187.07575448145,187.163584809882,187.251436832492,
187.311372610176,187.399229623174,187.487068740212,187.57491094705,187.662747965263,
187.750606557437,187.810508834867,187.898357394128,187.986188047343,188.074021858677,
188.161850539207,188.249700960886,188.309645059557,188.397496885361,188.485330768919,
188.573167724538,188.660999493881,188.748852889323,188.808781284248,188.896654168151,
188.984509272561,189.072367483231,189.160220476904,189.248094852537,189.307917508938,
189.395705498216,189.483475293582,189.571248411567,189.659016630357,189.746807507752,
189.807053733629,189.895056832682,189.983042532751,190.071030596453,190.159012711986,
190.247013862932,190.306189958319,190.393765197248,190.481322162753,190.568884375155,
190.656443223482,190.74402903841,190.80532618301,190.893910047384,190.982472415762,
191.071025137546,191.135001724242),.UNSPECIFIED.);
#395=B_SPLINE_CURVE_WITH_KNOTS('',3,(#33567,#33568,#33569,#33570,#33571,
#33572,#33573,#33574,#33575,#33576,#33577,#33578,#33579,#33580,#33581,#33582,
#33583,#33584,#33585,#33586,#33587,#33588,#33589,#33590,#33591,#33592,#33593,
#33594,#33595,#33596,#33597,#33598,#33599,#33600,#33601,#33602,#33603,#33604,
#33605,#33606,#33607,#33608,#33609,#33610,#33611,#33612,#33613,#33614,#33615,
#33616,#33617,#33618,#33619,#33620,#33621,#33622,#33623,#33624,#33625,#33626,
#33627,#33628,#33629,#33630,#33631,#33632,#33633,#33634,#33635,#33636,#33637,
#33638,#33639,#33640,#33641,#33642,#33643,#33644,#33645,#33646,#33647,#33648,
#33649,#33650,#33651,#33652,#33653,#33654,#33655,#33656,#33657,#33658,#33659,
#33660,#33661,#33662,#33663,#33664,#33665,#33666,#33667,#33668,#33669,#33670,
#33671,#33672,#33673,#33674,#33675,#33676,#33677,#33678,#33679,#33680,#33681,
#33682,#33683,#33684,#33685,#33686,#33687,#33688,#33689,#33690,#33691,#33692,
#33693,#33694,#33695,#33696,#33697,#33698,#33699,#33700,#33701,#33702,#33703,
#33704,#33705,#33706,#33707,#33708,#33709,#33710,#33711,#33712,#33713,#33714,
#33715,#33716,#33717,#33718,#33719,#33720,#33721,#33722,#33723,#33724,#33725,
#33726,#33727,#33728,#33729,#33730,#33731,#33732),.UNSPECIFIED.,.F.,.F.,
(4,3,3,3,3,3,3,3,3,3,3,3,3,3,3,3,3,3,3,3,3,3,3,3,3,3,3,3,3,3,3,3,3,3,3,
3,3,3,3,3,3,3,3,3,3,3,3,3,3,3,3,3,3,3,3,4),(185.353966561798,185.405459844816,
185.493311626503,185.581145518636,185.668982538294,185.756814419245,185.844667939728,
185.904331779964,185.99219028366,186.080030916271,186.167874637635,186.25571318292,
186.343573248018,186.403203715112,186.491053804869,186.578886013568,186.666721379097,
186.754551626175,186.842403559431,186.90207565026,186.989928966623,187.077764365727,
187.165602836015,187.253436132681,187.341291001396,187.400947585408,187.488821955081,
187.576678569885,187.664538289577,187.752392804605,187.840268647382,187.899819520556,
187.987609134066,188.075380579373,188.163155346114,188.250925226068,188.338717707918,
188.398691455705,188.486695776435,188.574682721781,188.662672030794,188.750655404904,
188.838657766452,188.897563390853,188.985140605913,189.072699573761,189.160263784227,
189.247824641547,189.335412399295,189.396435326001,189.484832149658,189.57321009574,
189.661583933721,189.749947134336,189.838318291413,189.895307261149),
 .UNSPECIFIED.);
#396=B_SPLINE_CURVE_WITH_KNOTS('',3,(#33733,#33734,#33735,#33736,#33737,
#33738,#33739,#33740,#33741,#33742),.UNSPECIFIED.,.F.,.F.,(4,2,2,2,4),(-6.1912792335152,
-6.12088779730415,-6.10166850366315,-6.08259528877872,-6.06755362652627),
 .UNSPECIFIED.);
#397=B_SPLINE_CURVE_WITH_KNOTS('',3,(#33745,#33746,#33747,#33748,#33749,
#33750,#33751,#33752,#33753,#33754,#33755,#33756,#33757,#33758,#33759),
 .UNSPECIFIED.,.F.,.F.,(4,1,1,1,1,1,1,1,1,1,1,1,4),(170.764858387386,171.113073755807,
171.611945690955,172.110817626103,172.609689561251,173.108561496399,173.607433431547,
174.106305366695,174.605177301843,175.104049236992,175.60292117214,176.101793107288,
176.22808870207),.UNSPECIFIED.);
#398=B_SPLINE_CURVE_WITH_KNOTS('',3,(#33762,#33763,#33764,#33765,#33766,
#33767,#33768,#33769,#33770,#33771,#33772,#33773,#33774,#33775,#33776,#33777,
#33778,#33779,#33780,#33781,#33782,#33783,#33784,#33785,#33786,#33787,#33788,
#33789,#33790,#33791,#33792,#33793,#33794,#33795,#33796,#33797,#33798,#33799,
#33800,#33801,#33802,#33803,#33804,#33805,#33806,#33807,#33808,#33809,#33810,
#33811,#33812,#33813,#33814,#33815,#33816,#33817,#33818,#33819,#33820,#33821,
#33822,#33823,#33824,#33825,#33826,#33827,#33828,#33829,#33830,#33831,#33832,
#33833,#33834,#33835,#33836,#33837,#33838,#33839,#33840,#33841,#33842,#33843,
#33844,#33845,#33846,#33847,#33848,#33849,#33850,#33851,#33852,#33853,#33854,
#33855,#33856,#33857,#33858,#33859,#33860,#33861,#33862,#33863,#33864,#33865,
#33866,#33867,#33868,#33869,#33870,#33871,#33872,#33873,#33874,#33875,#33876,
#33877,#33878,#33879,#33880,#33881,#33882,#33883,#33884,#33885,#33886,#33887,
#33888,#33889,#33890,#33891,#33892,#33893,#33894,#33895,#33896,#33897,#33898,
#33899,#33900,#33901,#33902,#33903,#33904,#33905,#33906,#33907,#33908,#33909,
#33910,#33911,#33912,#33913,#33914,#33915,#33916,#33917,#33918,#33919,#33920,
#33921,#33922,#33923,#33924,#33925,#33926,#33927,#33928,#33929,#33930),
 .UNSPECIFIED.,.F.,.F.,(4,3,3,3,3,3,3,3,3,3,3,3,3,3,3,3,3,3,3,3,3,3,3,3,
3,3,3,3,3,3,3,3,3,3,3,3,3,3,3,3,3,3,3,3,3,3,3,3,3,3,3,3,3,3,3,3,4),(-178.297882100285,
-178.208849797516,-178.191632214518,-178.107807278713,-178.02399957922,
-177.940189246353,-177.856384647973,-177.77255768974,-177.692495989827,
-177.608591418453,-177.524703139297,-177.440811534382,-177.356925446745,
-177.273017416127,-177.193359765137,-177.109475211766,-177.025607135838,
-176.941735826047,-176.857870042694,-176.773982136324,-176.694223540446,
-176.61034181593,-176.526476649979,-176.442608348443,-176.358745621261,
-176.274860821962,-176.195087315756,-176.111197803111,-176.027324727734,
-175.943448404497,-175.859577610181,-175.77568474517,-175.695951091065,
-175.612067842047,-175.528201118133,-175.444331221577,-175.36046688224,
-175.276580457569,-175.196814866375,-175.112928026889,-175.029057665353,
-174.945184093002,-174.861316064346,-174.777425963151,-174.697678641684,
-174.613793388471,-174.529924632591,-174.446052680509,-174.362186276864,
-174.278297793008,-174.198542416994,-174.114899946371,-174.031274766378,
-173.94764864838,-173.864026576569,-173.78038640654,-173.738545042839),
 .UNSPECIFIED.);
#399=B_SPLINE_CURVE_WITH_KNOTS('',3,(#33933,#33934,#33935,#33936,#33937,
#33938,#33939,#33940,#33941,#33942,#33943,#33944,#33945,#33946,#33947,#33948,
#33949,#33950,#33951,#33952,#33953,#33954,#33955,#33956,#33957,#33958,#33959,
#33960,#33961,#33962,#33963,#33964,#33965,#33966,#33967,#33968,#33969,#33970,
#33971,#33972,#33973,#33974,#33975,#33976,#33977,#33978,#33979,#33980,#33981,
#33982,#33983,#33984,#33985,#33986,#33987,#33988,#33989,#33990,#33991,#33992,
#33993,#33994,#33995,#33996,#33997,#33998,#33999,#34000,#34001,#34002,#34003,
#34004,#34005,#34006,#34007,#34008,#34009,#34010,#34011,#34012,#34013,#34014,
#34015,#34016,#34017,#34018,#34019,#34020,#34021,#34022,#34023,#34024,#34025,
#34026,#34027,#34028,#34029,#34030,#34031,#34032,#34033,#34034,#34035,#34036,
#34037,#34038,#34039,#34040,#34041,#34042,#34043,#34044,#34045,#34046,#34047,
#34048,#34049,#34050,#34051,#34052,#34053,#34054,#34055,#34056,#34057,#34058,
#34059,#34060,#34061,#34062,#34063,#34064,#34065,#34066,#34067,#34068,#34069,
#34070,#34071,#34072,#34073,#34074,#34075,#34076,#34077,#34078,#34079,#34080,
#34081,#34082,#34083,#34084,#34085,#34086,#34087,#34088,#34089,#34090,#34091,
#34092,#34093,#34094,#34095,#34096,#34097,#34098,#34099,#34100,#34101,#34102,
#34103,#34104,#34105,#34106,#34107,#34108,#34109,#34110,#34111,#34112,#34113,
#34114,#34115,#34116,#34117,#34118,#34119,#34120,#34121,#34122,#34123,#34124,
#34125,#34126,#34127,#34128,#34129,#34130,#34131,#34132,#34133,#34134,#34135,
#34136,#34137,#34138,#34139,#34140,#34141,#34142,#34143,#34144,#34145,#34146,
#34147,#34148,#34149,#34150,#34151,#34152,#34153,#34154,#34155,#34156,#34157,
#34158,#34159,#34160,#34161,#34162,#34163,#34164,#34165,#34166,#34167,#34168,
#34169,#34170,#34171,#34172,#34173,#34174,#34175,#34176,#34177,#34178,#34179,
#34180,#34181,#34182,#34183,#34184,#34185,#34186,#34187,#34188,#34189,#34190,
#34191,#34192,#34193,#34194,#34195,#34196,#34197,#34198,#34199,#34200,#34201,
#34202,#34203),.UNSPECIFIED.,.F.,.F.,(4,3,3,3,3,3,3,3,3,3,3,3,3,3,3,3,3,
3,3,3,3,3,3,3,3,3,3,3,3,3,3,3,3,3,3,3,3,3,3,3,3,3,3,3,3,3,3,3,3,3,3,3,3,
3,3,3,3,3,3,3,3,3,3,3,3,3,3,3,3,3,3,3,3,3,3,3,3,3,3,3,3,3,3,3,3,3,3,3,3,
3,4),(-2.84993027792945,-2.80581822492884,-2.77529095167904,-2.7639218300317,
-2.75777942373964,-2.71263817698004,-2.68370913192962,-2.63875182487813,
-2.59363222502916,-2.58642105701857,-2.57995978207043,-2.53462721743547,
-2.48902111530139,-2.44364758188306,-2.42724183695243,-2.39465624397139,
-2.38706665961561,-2.38082233194916,-2.33559763534729,-2.289576912667,-2.24355101834038,
-2.20505405572223,-2.18494067399242,-2.17696362392625,-2.16655709310407,
-2.12098494540008,-2.07475303934683,-2.02830225529523,-1.99659238554031,
-1.98209758802444,-1.97566444826943,-1.96991855489481,-1.92303849932432,
-1.90146277627555,-1.85485020732147,-1.80793499832861,-1.78593728731861,
-1.77037557248463,-1.76173309083023,-1.71460089183786,-1.66723806593038,
-1.63195331024862,-1.584641738859,-1.56888373105132,-1.55568481852088,-1.54982255046505,
-1.50191942593017,-1.45410564653405,-1.40615784942979,-1.35821005232553,
-1.34135883462771,-1.33595821079862,-1.28868021166659,-1.24070939844527,
-1.19246502715133,-1.14453907183535,-1.12692320891387,-1.11915523664791,
-1.08026432333022,-1.03220098375255,-0.983614733943928,-0.937169494271226,
-0.918719630218846,-0.904783582288534,-0.898697963027374,-0.848265869140248,
-0.797833775253121,-0.748864203381356,-0.699782475575903,-0.686312324754147,
-0.677639075649963,-0.628355660399474,-0.578788413932711,-0.529454269015081,
-0.511071810597535,-0.474708847474015,-0.461193855367628,-0.452940585084499,
-0.403785746204721,-0.353813383121523,-0.303841691601361,-0.262004898605367,
-0.241086502107369,-0.233148200519642,-0.225480555224177,-0.220168105609372,
-0.17099079510222,-0.120761505811504,-0.070321660673032,-0.0202259151736165,
0.),.UNSPECIFIED.);
#400=B_SPLINE_CURVE_WITH_KNOTS('',3,(#34206,#34207,#34208,#34209,#34210,
#34211,#34212,#34213,#34214,#34215,#34216,#34217,#34218,#34219),
 .UNSPECIFIED.,.F.,.F.,(4,2,2,2,2,2,4),(-1.02378211072902,-0.827714664332123,
-0.640554828731562,-0.390437320911094,-0.289794336115012,-0.139985920865823,
0.),.UNSPECIFIED.);
#401=B_SPLINE_CURVE_WITH_KNOTS('',3,(#35673,#35674,#35675,#35676,#35677,
#35678,#35679,#35680,#35681,#35682,#35683,#35684,#35685,#35686,#35687,#35688,
#35689,#35690,#35691,#35692,#35693,#35694,#35695,#35696,#35697,#35698,#35699,
#35700,#35701,#35702,#35703,#35704,#35705,#35706,#35707,#35708,#35709,#35710,
#35711,#35712,#35713,#35714,#35715,#35716,#35717,#35718,#35719,#35720,#35721,
#35722,#35723,#35724,#35725,#35726,#35727,#35728,#35729,#35730,#35731,#35732,
#35733,#35734,#35735,#35736,#35737,#35738,#35739,#35740,#35741,#35742,#35743,
#35744,#35745,#35746,#35747,#35748,#35749,#35750,#35751,#35752,#35753,#35754,
#35755,#35756,#35757,#35758,#35759,#35760,#35761,#35762,#35763,#35764,#35765,
#35766,#35767,#35768,#35769,#35770,#35771,#35772,#35773,#35774,#35775,#35776,
#35777,#35778),.UNSPECIFIED.,.F.,.F.,(4,3,3,3,3,3,3,3,3,3,3,3,3,3,3,3,3,
3,3,3,3,3,3,3,3,3,3,3,3,3,3,3,3,3,3,4),(-1.12653966532773,-1.08328443004837,
-1.03353709077206,-0.983959868704988,-0.972855476239986,-0.963909412895039,
-0.915025462469927,-0.866807833003593,-0.822978744363957,-0.816869072976604,
-0.795216619847291,-0.747460895965115,-0.69953853011811,-0.652271227547244,
-0.618804187172226,-0.607057707248577,-0.599647258206796,-0.553127126757695,
-0.518403066047171,-0.471676364421963,-0.425384243431735,-0.403792903604889,
-0.397276085507847,-0.390955965366398,-0.345490498978405,-0.299377878107159,
-0.253265257235913,-0.221607100081425,-0.205353593604308,-0.19501215756986,
-0.189043536422963,-0.168481916872947,-0.124214947369948,-0.0802229003350188,
-0.0371763150134234,-7.68796522159327E-15),.UNSPECIFIED.);
#402=B_SPLINE_CURVE_WITH_KNOTS('',3,(#37248,#37249,#37250,#37251,#37252,
#37253,#37254,#37255,#37256,#37257,#37258,#37259,#37260,#37261,#37262,#37263,
#37264,#37265,#37266,#37267,#37268,#37269,#37270,#37271,#37272,#37273,#37274,
#37275,#37276,#37277,#37278,#37279,#37280,#37281,#37282,#37283,#37284,#37285,
#37286,#37287,#37288,#37289,#37290,#37291,#37292,#37293,#37294,#37295,#37296,
#37297,#37298,#37299,#37300,#37301,#37302,#37303,#37304,#37305,#37306,#37307,
#37308,#37309,#37310,#37311,#37312,#37313,#37314,#37315,#37316,#37317,#37318,
#37319,#37320,#37321,#37322,#37323,#37324,#37325,#37326,#37327,#37328,#37329,
#37330,#37331,#37332,#37333,#37334,#37335,#37336,#37337,#37338,#37339,#37340,
#37341,#37342,#37343,#37344,#37345,#37346,#37347,#37348,#37349,#37350,#37351,
#37352,#37353,#37354,#37355,#37356,#37357,#37358,#37359),.UNSPECIFIED.,
 .F.,.F.,(4,3,3,3,3,3,3,3,3,3,3,3,3,3,3,3,3,3,3,3,3,3,3,3,3,3,3,3,3,3,3,
3,3,3,3,3,3,4),(-1.13094109509782,-1.09392182272659,-1.05040682482303,-1.00628645113637,
-0.999731233283575,-0.992626582922596,-0.947774596581187,-0.902652843289582,
-0.870560015591072,-0.859702426029801,-0.838467187892562,-0.793476327210687,
-0.747788564637451,-0.70352361360926,-0.670324900338118,-0.659878430803487,
-0.653412422619991,-0.638475761066728,-0.591272337150695,-0.570728760524689,
-0.52391018670982,-0.482335832098637,-0.461548654793045,-0.449191859151303,
-0.441818134511173,-0.440761477487453,-0.392779311016725,-0.341972967637929,
-0.291166624259132,-0.25477079622674,-0.238847621462569,-0.228959626544373,
-0.221325717796781,-0.172774573159914,-0.123227258018104,-0.0734982443681584,
-0.0241644143980285,0.),.UNSPECIFIED.);
#403=B_SPLINE_CURVE_WITH_KNOTS('',3,(#37360,#37361,#37362,#37363),
 .UNSPECIFIED.,.F.,.F.,(4,4),(-0.000448380443499476,0.),.UNSPECIFIED.);
#404=ELLIPSE('',#4421,2.82842712474618,2.);
#405=ELLIPSE('',#4422,2.82842712474618,2.);
#406=ELLIPSE('',#4424,2.8284271247462,2.);
#407=ELLIPSE('',#4426,2.8284271247462,2.);
#408=ELLIPSE('',#4562,4.28989109945289,3.72791464996848);
#409=ELLIPSE('',#4563,4.42862181409974,3.8415820723178);
#410=SHAPE_REPRESENTATION_RELATIONSHIP('SRR','None',#37779,#428);
#411=SHAPE_REPRESENTATION_RELATIONSHIP('SRR','None',#37780,#429);
#412=SHAPE_REPRESENTATION_RELATIONSHIP('SRR','None',#37781,#430);
#413=SHAPE_REPRESENTATION_RELATIONSHIP('SRR','None',#37782,#431);
#414=SHAPE_REPRESENTATION_RELATIONSHIP('SRR','None',#37783,#432);
#415=SHAPE_REPRESENTATION_RELATIONSHIP('SRR','None',#37784,#433);
#416=SHAPE_REPRESENTATION_RELATIONSHIP('SRR','None',#37785,#434);
#417=SHAPE_REPRESENTATION_RELATIONSHIP('SRR','None',#37786,#435);
#418=SHAPE_REPRESENTATION_RELATIONSHIP('SRR','None',#37787,#436);
#419=SHAPE_REPRESENTATION_RELATIONSHIP('SRR','None',#37788,#437);
#420=SHAPE_REPRESENTATION_RELATIONSHIP('SRR','None',#37789,#438);
#421=SHAPE_REPRESENTATION_RELATIONSHIP('SRR','None',#37790,#439);
#422=SHAPE_REPRESENTATION_RELATIONSHIP('SRR','None',#37791,#440);
#423=SHAPE_REPRESENTATION_RELATIONSHIP('SRR','None',#37792,#441);
#424=SHAPE_REPRESENTATION_RELATIONSHIP('SRR','None',#37793,#442);
#425=SHAPE_REPRESENTATION_RELATIONSHIP('SRR','None',#37794,#443);
#426=SHAPE_REPRESENTATION_RELATIONSHIP('SRR','None',#37795,#444);
#427=SHAPE_REPRESENTATION_RELATIONSHIP('SRR','None',#37796,#445);
#428=ADVANCED_BREP_SHAPE_REPRESENTATION('',(#464),#37683);
#429=ADVANCED_BREP_SHAPE_REPRESENTATION('',(#465),#37684);
#430=ADVANCED_BREP_SHAPE_REPRESENTATION('',(#466),#37685);
#431=ADVANCED_BREP_SHAPE_REPRESENTATION('',(#467),#37686);
#432=ADVANCED_BREP_SHAPE_REPRESENTATION('',(#468),#37687);
#433=ADVANCED_BREP_SHAPE_REPRESENTATION('',(#469),#37688);
#434=ADVANCED_BREP_SHAPE_REPRESENTATION('',(#470),#37689);
#435=ADVANCED_BREP_SHAPE_REPRESENTATION('',(#471),#37690);
#436=ADVANCED_BREP_SHAPE_REPRESENTATION('',(#472),#37691);
#437=ADVANCED_BREP_SHAPE_REPRESENTATION('',(#473),#37692);
#438=ADVANCED_BREP_SHAPE_REPRESENTATION('',(#474),#37693);
#439=ADVANCED_BREP_SHAPE_REPRESENTATION('',(#475),#37694);
#440=ADVANCED_BREP_SHAPE_REPRESENTATION('',(#476),#37695);
#441=ADVANCED_BREP_SHAPE_REPRESENTATION('',(#477),#37696);
#442=ADVANCED_BREP_SHAPE_REPRESENTATION('',(#478),#37697);
#443=ADVANCED_BREP_SHAPE_REPRESENTATION('',(#479),#37698);
#444=ADVANCED_BREP_SHAPE_REPRESENTATION('',(#480),#37699);
#445=ADVANCED_BREP_SHAPE_REPRESENTATION('',(#481),#37700);
#446=STYLED_ITEM('',(#37878),#464);
#447=STYLED_ITEM('',(#37879),#465);
#448=STYLED_ITEM('',(#37880),#466);
#449=STYLED_ITEM('',(#37881),#467);
#450=STYLED_ITEM('',(#37882),#468);
#451=STYLED_ITEM('',(#37878),#469);
#452=STYLED_ITEM('',(#37880),#470);
#453=STYLED_ITEM('',(#37880),#471);
#454=STYLED_ITEM('',(#37883),#472);
#455=STYLED_ITEM('',(#37881),#473);
#456=STYLED_ITEM('',(#37881),#474);
#457=STYLED_ITEM('',(#37880),#475);
#458=STYLED_ITEM('',(#37879),#476);
#459=STYLED_ITEM('',(#37884),#477);
#460=STYLED_ITEM('',(#37882),#478);
#461=STYLED_ITEM('',(#37884),#479);
#462=STYLED_ITEM('',(#37880),#480);
#463=STYLED_ITEM('',(#37883),#481);
#464=MANIFOLD_SOLID_BREP('Body1',#4144);
#465=MANIFOLD_SOLID_BREP('Body1',#4145);
#466=MANIFOLD_SOLID_BREP('Body1',#4146);
#467=MANIFOLD_SOLID_BREP('Body1',#4147);
#468=MANIFOLD_SOLID_BREP('Body1',#4148);
#469=MANIFOLD_SOLID_BREP('Body1',#4149);
#470=MANIFOLD_SOLID_BREP('Body1',#4150);
#471=MANIFOLD_SOLID_BREP('Body1',#4151);
#472=MANIFOLD_SOLID_BREP('Body1',#4152);
#473=MANIFOLD_SOLID_BREP('Body1',#4153);
#474=MANIFOLD_SOLID_BREP('Body1',#4154);
#475=MANIFOLD_SOLID_BREP('Body1',#4155);
#476=MANIFOLD_SOLID_BREP('Body1',#4156);
#477=MANIFOLD_SOLID_BREP('Body1',#4157);
#478=MANIFOLD_SOLID_BREP('Body1',#4158);
#479=MANIFOLD_SOLID_BREP('Body1',#4159);
#480=MANIFOLD_SOLID_BREP('Body1',#4160);
#481=MANIFOLD_SOLID_BREP('Body1',#4161);
#482=FACE_BOUND('',#817,.T.);
#483=FACE_BOUND('',#818,.T.);
#484=FACE_BOUND('',#819,.T.);
#485=FACE_BOUND('',#820,.T.);
#486=FACE_BOUND('',#832,.T.);
#487=FACE_BOUND('',#833,.T.);
#488=FACE_BOUND('',#834,.T.);
#489=FACE_BOUND('',#835,.T.);
#490=FACE_BOUND('',#843,.T.);
#491=FACE_BOUND('',#844,.T.);
#492=FACE_BOUND('',#846,.T.);
#493=FACE_BOUND('',#847,.T.);
#494=FACE_BOUND('',#852,.T.);
#495=FACE_BOUND('',#853,.T.);
#496=FACE_BOUND('',#856,.T.);
#497=FACE_BOUND('',#857,.T.);
#498=FACE_BOUND('',#883,.T.);
#499=FACE_BOUND('',#885,.T.);
#500=FACE_BOUND('',#913,.T.);
#501=FACE_BOUND('',#916,.T.);
#502=FACE_BOUND('',#920,.T.);
#503=FACE_BOUND('',#922,.T.);
#504=FACE_BOUND('',#992,.T.);
#505=FACE_BOUND('',#995,.T.);
#506=FACE_BOUND('',#1000,.T.);
#507=FACE_BOUND('',#1008,.T.);
#508=FACE_BOUND('',#1018,.T.);
#509=FACE_BOUND('',#1020,.T.);
#510=FACE_BOUND('',#1035,.T.);
#511=FACE_BOUND('',#1038,.T.);
#512=FACE_BOUND('',#1040,.T.);
#513=FACE_BOUND('',#1043,.T.);
#514=FACE_BOUND('',#1051,.T.);
#515=FACE_BOUND('',#1053,.T.);
#516=PLANE('',#4366);
#517=PLANE('',#4367);
#518=PLANE('',#4377);
#519=PLANE('',#4380);
#520=PLANE('',#4391);
#521=PLANE('',#4392);
#522=PLANE('',#4400);
#523=PLANE('',#4401);
#524=PLANE('',#4402);
#525=PLANE('',#4403);
#526=PLANE('',#4404);
#527=PLANE('',#4405);
#528=PLANE('',#4413);
#529=PLANE('',#4414);
#530=PLANE('',#4415);
#531=PLANE('',#4416);
#532=PLANE('',#4417);
#533=PLANE('',#4418);
#534=PLANE('',#4428);
#535=PLANE('',#4429);
#536=PLANE('',#4430);
#537=PLANE('',#4431);
#538=PLANE('',#4432);
#539=PLANE('',#4433);
#540=PLANE('',#4435);
#541=PLANE('',#4436);
#542=PLANE('',#4437);
#543=PLANE('',#4438);
#544=PLANE('',#4439);
#545=PLANE('',#4440);
#546=PLANE('',#4445);
#547=PLANE('',#4446);
#548=PLANE('',#4447);
#549=PLANE('',#4448);
#550=PLANE('',#4452);
#551=PLANE('',#4453);
#552=PLANE('',#4483);
#553=PLANE('',#4487);
#554=PLANE('',#4495);
#555=PLANE('',#4496);
#556=PLANE('',#4564);
#557=PLANE('',#4565);
#558=PLANE('',#4566);
#559=PLANE('',#4567);
#560=PLANE('',#4568);
#561=PLANE('',#4569);
#562=PLANE('',#4570);
#563=PLANE('',#4571);
#564=PLANE('',#4575);
#565=PLANE('',#4576);
#566=PLANE('',#4581);
#567=PLANE('',#4582);
#568=PLANE('',#4588);
#569=PLANE('',#4591);
#570=PLANE('',#4594);
#571=PLANE('',#4595);
#572=PLANE('',#4597);
#573=PLANE('',#4598);
#574=PLANE('',#4599);
#575=PLANE('',#4600);
#576=PLANE('',#4601);
#577=PLANE('',#4602);
#578=PLANE('',#4610);
#579=PLANE('',#4611);
#580=PLANE('',#4613);
#581=PLANE('',#4614);
#582=PLANE('',#4615);
#583=PLANE('',#4616);
#584=PLANE('',#4617);
#585=PLANE('',#4618);
#586=PLANE('',#4623);
#587=PLANE('',#4624);
#588=PLANE('',#4626);
#589=PLANE('',#4628);
#590=PLANE('',#4634);
#591=PLANE('',#4639);
#592=PLANE('',#4641);
#593=PLANE('',#4645);
#594=PLANE('',#4650);
#595=PLANE('',#4652);
#596=PLANE('',#4660);
#597=PLANE('',#4661);
#598=PLANE('',#4663);
#599=PLANE('',#4664);
#600=PLANE('',#4665);
#601=PLANE('',#4672);
#602=FACE_OUTER_BOUND('',#814,.T.);
#603=FACE_OUTER_BOUND('',#815,.T.);
#604=FACE_OUTER_BOUND('',#816,.T.);
#605=FACE_OUTER_BOUND('',#821,.T.);
#606=FACE_OUTER_BOUND('',#822,.T.);
#607=FACE_OUTER_BOUND('',#823,.T.);
#608=FACE_OUTER_BOUND('',#824,.T.);
#609=FACE_OUTER_BOUND('',#825,.T.);
#610=FACE_OUTER_BOUND('',#826,.T.);
#611=FACE_OUTER_BOUND('',#827,.T.);
#612=FACE_OUTER_BOUND('',#828,.T.);
#613=FACE_OUTER_BOUND('',#829,.T.);
#614=FACE_OUTER_BOUND('',#830,.T.);
#615=FACE_OUTER_BOUND('',#831,.T.);
#616=FACE_OUTER_BOUND('',#836,.T.);
#617=FACE_OUTER_BOUND('',#837,.T.);
#618=FACE_OUTER_BOUND('',#838,.T.);
#619=FACE_OUTER_BOUND('',#839,.T.);
#620=FACE_OUTER_BOUND('',#840,.T.);
#621=FACE_OUTER_BOUND('',#841,.T.);
#622=FACE_OUTER_BOUND('',#842,.T.);
#623=FACE_OUTER_BOUND('',#845,.T.);
#624=FACE_OUTER_BOUND('',#848,.T.);
#625=FACE_OUTER_BOUND('',#849,.T.);
#626=FACE_OUTER_BOUND('',#850,.T.);
#627=FACE_OUTER_BOUND('',#851,.T.);
#628=FACE_OUTER_BOUND('',#854,.T.);
#629=FACE_OUTER_BOUND('',#855,.T.);
#630=FACE_OUTER_BOUND('',#858,.T.);
#631=FACE_OUTER_BOUND('',#859,.T.);
#632=FACE_OUTER_BOUND('',#860,.T.);
#633=FACE_OUTER_BOUND('',#861,.T.);
#634=FACE_OUTER_BOUND('',#862,.T.);
#635=FACE_OUTER_BOUND('',#863,.T.);
#636=FACE_OUTER_BOUND('',#864,.T.);
#637=FACE_OUTER_BOUND('',#865,.T.);
#638=FACE_OUTER_BOUND('',#866,.T.);
#639=FACE_OUTER_BOUND('',#867,.T.);
#640=FACE_OUTER_BOUND('',#868,.T.);
#641=FACE_OUTER_BOUND('',#869,.T.);
#642=FACE_OUTER_BOUND('',#870,.T.);
#643=FACE_OUTER_BOUND('',#871,.T.);
#644=FACE_OUTER_BOUND('',#872,.T.);
#645=FACE_OUTER_BOUND('',#873,.T.);
#646=FACE_OUTER_BOUND('',#874,.T.);
#647=FACE_OUTER_BOUND('',#875,.T.);
#648=FACE_OUTER_BOUND('',#876,.T.);
#649=FACE_OUTER_BOUND('',#877,.T.);
#650=FACE_OUTER_BOUND('',#878,.T.);
#651=FACE_OUTER_BOUND('',#879,.T.);
#652=FACE_OUTER_BOUND('',#880,.T.);
#653=FACE_OUTER_BOUND('',#881,.T.);
#654=FACE_OUTER_BOUND('',#882,.T.);
#655=FACE_OUTER_BOUND('',#884,.T.);
#656=FACE_OUTER_BOUND('',#886,.T.);
#657=FACE_OUTER_BOUND('',#887,.T.);
#658=FACE_OUTER_BOUND('',#888,.T.);
#659=FACE_OUTER_BOUND('',#889,.T.);
#660=FACE_OUTER_BOUND('',#890,.T.);
#661=FACE_OUTER_BOUND('',#891,.T.);
#662=FACE_OUTER_BOUND('',#892,.T.);
#663=FACE_OUTER_BOUND('',#893,.T.);
#664=FACE_OUTER_BOUND('',#894,.T.);
#665=FACE_OUTER_BOUND('',#895,.T.);
#666=FACE_OUTER_BOUND('',#896,.T.);
#667=FACE_OUTER_BOUND('',#897,.T.);
#668=FACE_OUTER_BOUND('',#898,.T.);
#669=FACE_OUTER_BOUND('',#899,.T.);
#670=FACE_OUTER_BOUND('',#900,.T.);
#671=FACE_OUTER_BOUND('',#901,.T.);
#672=FACE_OUTER_BOUND('',#902,.T.);
#673=FACE_OUTER_BOUND('',#903,.T.);
#674=FACE_OUTER_BOUND('',#904,.T.);
#675=FACE_OUTER_BOUND('',#905,.T.);
#676=FACE_OUTER_BOUND('',#906,.T.);
#677=FACE_OUTER_BOUND('',#907,.T.);
#678=FACE_OUTER_BOUND('',#908,.T.);
#679=FACE_OUTER_BOUND('',#909,.T.);
#680=FACE_OUTER_BOUND('',#910,.T.);
#681=FACE_OUTER_BOUND('',#911,.T.);
#682=FACE_OUTER_BOUND('',#912,.T.);
#683=FACE_OUTER_BOUND('',#914,.T.);
#684=FACE_OUTER_BOUND('',#915,.T.);
#685=FACE_OUTER_BOUND('',#917,.T.);
#686=FACE_OUTER_BOUND('',#918,.T.);
#687=FACE_OUTER_BOUND('',#919,.T.);
#688=FACE_OUTER_BOUND('',#921,.T.);
#689=FACE_OUTER_BOUND('',#923,.T.);
#690=FACE_OUTER_BOUND('',#924,.T.);
#691=FACE_OUTER_BOUND('',#925,.T.);
#692=FACE_OUTER_BOUND('',#926,.T.);
#693=FACE_OUTER_BOUND('',#927,.T.);
#694=FACE_OUTER_BOUND('',#928,.T.);
#695=FACE_OUTER_BOUND('',#929,.T.);
#696=FACE_OUTER_BOUND('',#930,.T.);
#697=FACE_OUTER_BOUND('',#931,.T.);
#698=FACE_OUTER_BOUND('',#932,.T.);
#699=FACE_OUTER_BOUND('',#933,.T.);
#700=FACE_OUTER_BOUND('',#934,.T.);
#701=FACE_OUTER_BOUND('',#935,.T.);
#702=FACE_OUTER_BOUND('',#936,.T.);
#703=FACE_OUTER_BOUND('',#937,.T.);
#704=FACE_OUTER_BOUND('',#938,.T.);
#705=FACE_OUTER_BOUND('',#939,.T.);
#706=FACE_OUTER_BOUND('',#940,.T.);
#707=FACE_OUTER_BOUND('',#941,.T.);
#708=FACE_OUTER_BOUND('',#942,.T.);
#709=FACE_OUTER_BOUND('',#943,.T.);
#710=FACE_OUTER_BOUND('',#944,.T.);
#711=FACE_OUTER_BOUND('',#945,.T.);
#712=FACE_OUTER_BOUND('',#946,.T.);
#713=FACE_OUTER_BOUND('',#947,.T.);
#714=FACE_OUTER_BOUND('',#948,.T.);
#715=FACE_OUTER_BOUND('',#949,.T.);
#716=FACE_OUTER_BOUND('',#950,.T.);
#717=FACE_OUTER_BOUND('',#951,.T.);
#718=FACE_OUTER_BOUND('',#952,.T.);
#719=FACE_OUTER_BOUND('',#953,.T.);
#720=FACE_OUTER_BOUND('',#954,.T.);
#721=FACE_OUTER_BOUND('',#955,.T.);
#722=FACE_OUTER_BOUND('',#956,.T.);
#723=FACE_OUTER_BOUND('',#957,.T.);
#724=FACE_OUTER_BOUND('',#958,.T.);
#725=FACE_OUTER_BOUND('',#959,.T.);
#726=FACE_OUTER_BOUND('',#960,.T.);
#727=FACE_OUTER_BOUND('',#961,.T.);
#728=FACE_OUTER_BOUND('',#962,.T.);
#729=FACE_OUTER_BOUND('',#963,.T.);
#730=FACE_OUTER_BOUND('',#964,.T.);
#731=FACE_OUTER_BOUND('',#965,.T.);
#732=FACE_OUTER_BOUND('',#966,.T.);
#733=FACE_OUTER_BOUND('',#967,.T.);
#734=FACE_OUTER_BOUND('',#968,.T.);
#735=FACE_OUTER_BOUND('',#969,.T.);
#736=FACE_OUTER_BOUND('',#970,.T.);
#737=FACE_OUTER_BOUND('',#971,.T.);
#738=FACE_OUTER_BOUND('',#972,.T.);
#739=FACE_OUTER_BOUND('',#973,.T.);
#740=FACE_OUTER_BOUND('',#974,.T.);
#741=FACE_OUTER_BOUND('',#975,.T.);
#742=FACE_OUTER_BOUND('',#976,.T.);
#743=FACE_OUTER_BOUND('',#977,.T.);
#744=FACE_OUTER_BOUND('',#978,.T.);
#745=FACE_OUTER_BOUND('',#979,.T.);
#746=FACE_OUTER_BOUND('',#980,.T.);
#747=FACE_OUTER_BOUND('',#981,.T.);
#748=FACE_OUTER_BOUND('',#982,.T.);
#749=FACE_OUTER_BOUND('',#983,.T.);
#750=FACE_OUTER_BOUND('',#984,.T.);
#751=FACE_OUTER_BOUND('',#985,.T.);
#752=FACE_OUTER_BOUND('',#986,.T.);
#753=FACE_OUTER_BOUND('',#987,.T.);
#754=FACE_OUTER_BOUND('',#988,.T.);
#755=FACE_OUTER_BOUND('',#989,.T.);
#756=FACE_OUTER_BOUND('',#990,.T.);
#757=FACE_OUTER_BOUND('',#991,.T.);
#758=FACE_OUTER_BOUND('',#993,.T.);
#759=FACE_OUTER_BOUND('',#994,.T.);
#760=FACE_OUTER_BOUND('',#996,.T.);
#761=FACE_OUTER_BOUND('',#997,.T.);
#762=FACE_OUTER_BOUND('',#998,.T.);
#763=FACE_OUTER_BOUND('',#999,.T.);
#764=FACE_OUTER_BOUND('',#1001,.T.);
#765=FACE_OUTER_BOUND('',#1002,.T.);
#766=FACE_OUTER_BOUND('',#1003,.T.);
#767=FACE_OUTER_BOUND('',#1004,.T.);
#768=FACE_OUTER_BOUND('',#1005,.T.);
#769=FACE_OUTER_BOUND('',#1006,.T.);
#770=FACE_OUTER_BOUND('',#1007,.T.);
#771=FACE_OUTER_BOUND('',#1009,.T.);
#772=FACE_OUTER_BOUND('',#1010,.T.);
#773=FACE_OUTER_BOUND('',#1011,.T.);
#774=FACE_OUTER_BOUND('',#1012,.T.);
#775=FACE_OUTER_BOUND('',#1013,.T.);
#776=FACE_OUTER_BOUND('',#1014,.T.);
#777=FACE_OUTER_BOUND('',#1015,.T.);
#778=FACE_OUTER_BOUND('',#1016,.T.);
#779=FACE_OUTER_BOUND('',#1017,.T.);
#780=FACE_OUTER_BOUND('',#1019,.T.);
#781=FACE_OUTER_BOUND('',#1021,.T.);
#782=FACE_OUTER_BOUND('',#1022,.T.);
#783=FACE_OUTER_BOUND('',#1023,.T.);
#784=FACE_OUTER_BOUND('',#1024,.T.);
#785=FACE_OUTER_BOUND('',#1025,.T.);
#786=FACE_OUTER_BOUND('',#1026,.T.);
#787=FACE_OUTER_BOUND('',#1027,.T.);
#788=FACE_OUTER_BOUND('',#1028,.T.);
#789=FACE_OUTER_BOUND('',#1029,.T.);
#790=FACE_OUTER_BOUND('',#1030,.T.);
#791=FACE_OUTER_BOUND('',#1031,.T.);
#792=FACE_OUTER_BOUND('',#1032,.T.);
#793=FACE_OUTER_BOUND('',#1033,.T.);
#794=FACE_OUTER_BOUND('',#1034,.T.);
#795=FACE_OUTER_BOUND('',#1036,.T.);
#796=FACE_OUTER_BOUND('',#1037,.T.);
#797=FACE_OUTER_BOUND('',#1039,.T.);
#798=FACE_OUTER_BOUND('',#1041,.T.);
#799=FACE_OUTER_BOUND('',#1042,.T.);
#800=FACE_OUTER_BOUND('',#1044,.T.);
#801=FACE_OUTER_BOUND('',#1045,.T.);
#802=FACE_OUTER_BOUND('',#1046,.T.);
#803=FACE_OUTER_BOUND('',#1047,.T.);
#804=FACE_OUTER_BOUND('',#1048,.T.);
#805=FACE_OUTER_BOUND('',#1049,.T.);
#806=FACE_OUTER_BOUND('',#1050,.T.);
#807=FACE_OUTER_BOUND('',#1052,.T.);
#808=FACE_OUTER_BOUND('',#1054,.T.);
#809=FACE_OUTER_BOUND('',#1055,.T.);
#810=FACE_OUTER_BOUND('',#1056,.T.);
#811=FACE_OUTER_BOUND('',#1057,.T.);
#812=FACE_OUTER_BOUND('',#1058,.T.);
#813=FACE_OUTER_BOUND('',#1059,.T.);
#814=EDGE_LOOP('',(#2639,#2640,#2641,#2642));
#815=EDGE_LOOP('',(#2643,#2644,#2645,#2646));
#816=EDGE_LOOP('',(#2647,#2648,#2649,#2650,#2651,#2652,#2653,#2654));
#817=EDGE_LOOP('',(#2655));
#818=EDGE_LOOP('',(#2656));
#819=EDGE_LOOP('',(#2657));
#820=EDGE_LOOP('',(#2658));
#821=EDGE_LOOP('',(#2659,#2660,#2661,#2662));
#822=EDGE_LOOP('',(#2663,#2664,#2665,#2666));
#823=EDGE_LOOP('',(#2667,#2668,#2669,#2670));
#824=EDGE_LOOP('',(#2671,#2672,#2673,#2674));
#825=EDGE_LOOP('',(#2675,#2676,#2677,#2678));
#826=EDGE_LOOP('',(#2679,#2680,#2681,#2682));
#827=EDGE_LOOP('',(#2683,#2684,#2685,#2686));
#828=EDGE_LOOP('',(#2687,#2688,#2689,#2690));
#829=EDGE_LOOP('',(#2691,#2692,#2693,#2694));
#830=EDGE_LOOP('',(#2695,#2696,#2697,#2698));
#831=EDGE_LOOP('',(#2699,#2700,#2701,#2702,#2703,#2704,#2705,#2706));
#832=EDGE_LOOP('',(#2707));
#833=EDGE_LOOP('',(#2708));
#834=EDGE_LOOP('',(#2709));
#835=EDGE_LOOP('',(#2710));
#836=EDGE_LOOP('',(#2711,#2712,#2713,#2714));
#837=EDGE_LOOP('',(#2715,#2716,#2717,#2718));
#838=EDGE_LOOP('',(#2719,#2720,#2721,#2722));
#839=EDGE_LOOP('',(#2723,#2724,#2725,#2726));
#840=EDGE_LOOP('',(#2727,#2728,#2729,#2730));
#841=EDGE_LOOP('',(#2731,#2732,#2733,#2734));
#842=EDGE_LOOP('',(#2735,#2736,#2737,#2738));
#843=EDGE_LOOP('',(#2739));
#844=EDGE_LOOP('',(#2740));
#845=EDGE_LOOP('',(#2741,#2742,#2743,#2744));
#846=EDGE_LOOP('',(#2745));
#847=EDGE_LOOP('',(#2746));
#848=EDGE_LOOP('',(#2747,#2748,#2749,#2750));
#849=EDGE_LOOP('',(#2751,#2752,#2753,#2754));
#850=EDGE_LOOP('',(#2755,#2756,#2757,#2758));
#851=EDGE_LOOP('',(#2759,#2760,#2761,#2762));
#852=EDGE_LOOP('',(#2763));
#853=EDGE_LOOP('',(#2764));
#854=EDGE_LOOP('',(#2765,#2766,#2767,#2768));
#855=EDGE_LOOP('',(#2769,#2770,#2771,#2772));
#856=EDGE_LOOP('',(#2773));
#857=EDGE_LOOP('',(#2774));
#858=EDGE_LOOP('',(#2775,#2776,#2777,#2778));
#859=EDGE_LOOP('',(#2779,#2780,#2781,#2782));
#860=EDGE_LOOP('',(#2783,#2784,#2785,#2786));
#861=EDGE_LOOP('',(#2787,#2788,#2789,#2790));
#862=EDGE_LOOP('',(#2791,#2792,#2793,#2794));
#863=EDGE_LOOP('',(#2795,#2796,#2797,#2798));
#864=EDGE_LOOP('',(#2799,#2800,#2801,#2802));
#865=EDGE_LOOP('',(#2803,#2804,#2805,#2806));
#866=EDGE_LOOP('',(#2807,#2808,#2809,#2810));
#867=EDGE_LOOP('',(#2811,#2812,#2813,#2814));
#868=EDGE_LOOP('',(#2815,#2816,#2817,#2818));
#869=EDGE_LOOP('',(#2819,#2820,#2821,#2822));
#870=EDGE_LOOP('',(#2823,#2824,#2825,#2826));
#871=EDGE_LOOP('',(#2827,#2828,#2829,#2830));
#872=EDGE_LOOP('',(#2831,#2832,#2833,#2834));
#873=EDGE_LOOP('',(#2835,#2836,#2837,#2838));
#874=EDGE_LOOP('',(#2839,#2840,#2841,#2842));
#875=EDGE_LOOP('',(#2843,#2844,#2845,#2846));
#876=EDGE_LOOP('',(#2847,#2848,#2849,#2850));
#877=EDGE_LOOP('',(#2851,#2852,#2853,#2854));
#878=EDGE_LOOP('',(#2855,#2856,#2857,#2858));
#879=EDGE_LOOP('',(#2859,#2860,#2861,#2862));
#880=EDGE_LOOP('',(#2863,#2864,#2865,#2866));
#881=EDGE_LOOP('',(#2867,#2868,#2869,#2870));
#882=EDGE_LOOP('',(#2871,#2872,#2873,#2874,#2875));
#883=EDGE_LOOP('',(#2876));
#884=EDGE_LOOP('',(#2877,#2878,#2879,#2880,#2881));
#885=EDGE_LOOP('',(#2882));
#886=EDGE_LOOP('',(#2883,#2884,#2885,#2886,#2887,#2888));
#887=EDGE_LOOP('',(#2889,#2890,#2891,#2892,#2893,#2894));
#888=EDGE_LOOP('',(#2895,#2896,#2897,#2898,#2899,#2900));
#889=EDGE_LOOP('',(#2901,#2902,#2903,#2904,#2905,#2906));
#890=EDGE_LOOP('',(#2907,#2908,#2909,#2910,#2911,#2912));
#891=EDGE_LOOP('',(#2913,#2914,#2915,#2916,#2917,#2918));
#892=EDGE_LOOP('',(#2919,#2920,#2921,#2922,#2923,#2924));
#893=EDGE_LOOP('',(#2925,#2926,#2927,#2928,#2929,#2930));
#894=EDGE_LOOP('',(#2931,#2932,#2933,#2934,#2935,#2936));
#895=EDGE_LOOP('',(#2937,#2938,#2939,#2940,#2941,#2942));
#896=EDGE_LOOP('',(#2943,#2944,#2945,#2946,#2947,#2948));
#897=EDGE_LOOP('',(#2949,#2950,#2951,#2952));
#898=EDGE_LOOP('',(#2953,#2954,#2955,#2956,#2957,#2958));
#899=EDGE_LOOP('',(#2959,#2960,#2961,#2962,#2963,#2964));
#900=EDGE_LOOP('',(#2965,#2966,#2967,#2968,#2969,#2970));
#901=EDGE_LOOP('',(#2971,#2972,#2973,#2974,#2975));
#902=EDGE_LOOP('',(#2976,#2977,#2978,#2979,#2980,#2981));
#903=EDGE_LOOP('',(#2982,#2983,#2984,#2985,#2986));
#904=EDGE_LOOP('',(#2987,#2988,#2989,#2990,#2991,#2992));
#905=EDGE_LOOP('',(#2993,#2994,#2995,#2996));
#906=EDGE_LOOP('',(#2997,#2998,#2999,#3000,#3001,#3002));
#907=EDGE_LOOP('',(#3003,#3004,#3005,#3006));
#908=EDGE_LOOP('',(#3007,#3008,#3009,#3010,#3011));
#909=EDGE_LOOP('',(#3012,#3013,#3014,#3015,#3016,#3017));
#910=EDGE_LOOP('',(#3018,#3019,#3020,#3021,#3022,#3023,#3024,#3025,#3026,
#3027,#3028,#3029,#3030,#3031,#3032,#3033,#3034,#3035,#3036,#3037,#3038,
#3039,#3040,#3041,#3042,#3043,#3044,#3045,#3046,#3047,#3048,#3049,#3050,
#3051,#3052,#3053,#3054,#3055,#3056,#3057,#3058,#3059,#3060,#3061,#3062,
#3063,#3064));
#911=EDGE_LOOP('',(#3065,#3066,#3067,#3068,#3069,#3070,#3071,#3072,#3073,
#3074,#3075,#3076,#3077,#3078,#3079,#3080,#3081,#3082,#3083,#3084,#3085,
#3086,#3087,#3088,#3089,#3090,#3091,#3092,#3093,#3094,#3095,#3096,#3097,
#3098,#3099,#3100,#3101,#3102,#3103,#3104,#3105,#3106,#3107,#3108,#3109,
#3110));
#912=EDGE_LOOP('',(#3111));
#913=EDGE_LOOP('',(#3112,#3113,#3114,#3115,#3116));
#914=EDGE_LOOP('',(#3117,#3118,#3119,#3120));
#915=EDGE_LOOP('',(#3121));
#916=EDGE_LOOP('',(#3122,#3123,#3124,#3125,#3126));
#917=EDGE_LOOP('',(#3127,#3128,#3129,#3130));
#918=EDGE_LOOP('',(#3131,#3132,#3133,#3134));
#919=EDGE_LOOP('',(#3135));
#920=EDGE_LOOP('',(#3136));
#921=EDGE_LOOP('',(#3137));
#922=EDGE_LOOP('',(#3138));
#923=EDGE_LOOP('',(#3139,#3140,#3141,#3142));
#924=EDGE_LOOP('',(#3143,#3144,#3145,#3146));
#925=EDGE_LOOP('',(#3147,#3148,#3149,#3150));
#926=EDGE_LOOP('',(#3151,#3152,#3153,#3154));
#927=EDGE_LOOP('',(#3155,#3156,#3157,#3158));
#928=EDGE_LOOP('',(#3159,#3160,#3161,#3162));
#929=EDGE_LOOP('',(#3163,#3164,#3165,#3166));
#930=EDGE_LOOP('',(#3167,#3168,#3169,#3170));
#931=EDGE_LOOP('',(#3171,#3172,#3173,#3174));
#932=EDGE_LOOP('',(#3175,#3176,#3177,#3178));
#933=EDGE_LOOP('',(#3179,#3180,#3181,#3182));
#934=EDGE_LOOP('',(#3183,#3184,#3185,#3186));
#935=EDGE_LOOP('',(#3187,#3188,#3189,#3190));
#936=EDGE_LOOP('',(#3191,#3192,#3193,#3194));
#937=EDGE_LOOP('',(#3195,#3196,#3197,#3198));
#938=EDGE_LOOP('',(#3199,#3200,#3201,#3202));
#939=EDGE_LOOP('',(#3203,#3204,#3205,#3206));
#940=EDGE_LOOP('',(#3207,#3208,#3209,#3210));
#941=EDGE_LOOP('',(#3211,#3212,#3213,#3214));
#942=EDGE_LOOP('',(#3215,#3216,#3217,#3218));
#943=EDGE_LOOP('',(#3219,#3220,#3221,#3222));
#944=EDGE_LOOP('',(#3223,#3224,#3225,#3226));
#945=EDGE_LOOP('',(#3227,#3228,#3229,#3230));
#946=EDGE_LOOP('',(#3231,#3232,#3233,#3234));
#947=EDGE_LOOP('',(#3235,#3236,#3237,#3238));
#948=EDGE_LOOP('',(#3239,#3240,#3241,#3242));
#949=EDGE_LOOP('',(#3243,#3244,#3245,#3246));
#950=EDGE_LOOP('',(#3247,#3248,#3249,#3250));
#951=EDGE_LOOP('',(#3251,#3252,#3253,#3254));
#952=EDGE_LOOP('',(#3255,#3256,#3257,#3258,#3259));
#953=EDGE_LOOP('',(#3260,#3261,#3262,#3263,#3264,#3265));
#954=EDGE_LOOP('',(#3266,#3267,#3268,#3269,#3270));
#955=EDGE_LOOP('',(#3271,#3272,#3273,#3274,#3275));
#956=EDGE_LOOP('',(#3276,#3277,#3278,#3279,#3280,#3281));
#957=EDGE_LOOP('',(#3282,#3283,#3284,#3285,#3286));
#958=EDGE_LOOP('',(#3287,#3288,#3289,#3290,#3291));
#959=EDGE_LOOP('',(#3292,#3293,#3294,#3295,#3296));
#960=EDGE_LOOP('',(#3297,#3298,#3299,#3300,#3301));
#961=EDGE_LOOP('',(#3302,#3303,#3304,#3305,#3306));
#962=EDGE_LOOP('',(#3307,#3308,#3309,#3310,#3311));
#963=EDGE_LOOP('',(#3312,#3313,#3314,#3315,#3316,#3317));
#964=EDGE_LOOP('',(#3318,#3319,#3320,#3321,#3322,#3323));
#965=EDGE_LOOP('',(#3324,#3325,#3326,#3327,#3328));
#966=EDGE_LOOP('',(#3329,#3330,#3331,#3332,#3333,#3334));
#967=EDGE_LOOP('',(#3335,#3336,#3337,#3338));
#968=EDGE_LOOP('',(#3339,#3340,#3341,#3342,#3343,#3344));
#969=EDGE_LOOP('',(#3345,#3346,#3347,#3348,#3349));
#970=EDGE_LOOP('',(#3350,#3351,#3352,#3353,#3354,#3355));
#971=EDGE_LOOP('',(#3356,#3357,#3358,#3359,#3360,#3361));
#972=EDGE_LOOP('',(#3362,#3363,#3364,#3365,#3366));
#973=EDGE_LOOP('',(#3367,#3368,#3369,#3370,#3371,#3372));
#974=EDGE_LOOP('',(#3373,#3374,#3375,#3376,#3377));
#975=EDGE_LOOP('',(#3378,#3379,#3380,#3381,#3382));
#976=EDGE_LOOP('',(#3383,#3384,#3385,#3386,#3387,#3388));
#977=EDGE_LOOP('',(#3389,#3390,#3391,#3392,#3393));
#978=EDGE_LOOP('',(#3394,#3395,#3396,#3397,#3398));
#979=EDGE_LOOP('',(#3399,#3400,#3401,#3402,#3403,#3404));
#980=EDGE_LOOP('',(#3405,#3406,#3407,#3408));
#981=EDGE_LOOP('',(#3409,#3410,#3411,#3412));
#982=EDGE_LOOP('',(#3413,#3414,#3415,#3416,#3417,#3418,#3419,#3420,#3421,
#3422,#3423,#3424,#3425,#3426,#3427,#3428,#3429,#3430,#3431,#3432,#3433,
#3434,#3435,#3436,#3437,#3438,#3439,#3440,#3441,#3442,#3443,#3444,#3445,
#3446,#3447,#3448,#3449,#3450,#3451,#3452,#3453,#3454,#3455,#3456,#3457,
#3458,#3459,#3460,#3461,#3462,#3463,#3464,#3465,#3466,#3467,#3468,#3469,
#3470,#3471,#3472,#3473,#3474,#3475,#3476,#3477,#3478,#3479,#3480,#3481,
#3482,#3483,#3484,#3485,#3486,#3487,#3488,#3489,#3490,#3491,#3492,#3493));
#983=EDGE_LOOP('',(#3494,#3495,#3496,#3497,#3498,#3499,#3500,#3501,#3502,
#3503,#3504,#3505,#3506,#3507,#3508,#3509,#3510,#3511,#3512,#3513,#3514,
#3515,#3516,#3517,#3518,#3519,#3520,#3521,#3522,#3523,#3524,#3525,#3526,
#3527,#3528,#3529,#3530,#3531,#3532,#3533,#3534,#3535,#3536,#3537,#3538,
#3539,#3540,#3541,#3542,#3543,#3544,#3545,#3546,#3547,#3548,#3549,#3550,
#3551,#3552,#3553,#3554,#3555,#3556,#3557,#3558,#3559,#3560,#3561,#3562,
#3563,#3564,#3565,#3566,#3567,#3568,#3569,#3570,#3571,#3572,#3573));
#984=EDGE_LOOP('',(#3574,#3575,#3576,#3577));
#985=EDGE_LOOP('',(#3578,#3579,#3580,#3581));
#986=EDGE_LOOP('',(#3582,#3583,#3584,#3585));
#987=EDGE_LOOP('',(#3586,#3587,#3588,#3589));
#988=EDGE_LOOP('',(#3590,#3591,#3592,#3593));
#989=EDGE_LOOP('',(#3594,#3595,#3596,#3597));
#990=EDGE_LOOP('',(#3598,#3599,#3600,#3601,#3602,#3603));
#991=EDGE_LOOP('',(#3604));
#992=EDGE_LOOP('',(#3605,#3606,#3607,#3608,#3609));
#993=EDGE_LOOP('',(#3610,#3611,#3612,#3613));
#994=EDGE_LOOP('',(#3614));
#995=EDGE_LOOP('',(#3615,#3616,#3617,#3618,#3619,#3620));
#996=EDGE_LOOP('',(#3621,#3622,#3623,#3624));
#997=EDGE_LOOP('',(#3625,#3626,#3627,#3628));
#998=EDGE_LOOP('',(#3629,#3630,#3631,#3632));
#999=EDGE_LOOP('',(#3633,#3634,#3635,#3636,#3637,#3638,#3639));
#1000=EDGE_LOOP('',(#3640));
#1001=EDGE_LOOP('',(#3641,#3642,#3643,#3644));
#1002=EDGE_LOOP('',(#3645,#3646,#3647,#3648));
#1003=EDGE_LOOP('',(#3649,#3650,#3651,#3652));
#1004=EDGE_LOOP('',(#3653,#3654,#3655,#3656));
#1005=EDGE_LOOP('',(#3657,#3658,#3659,#3660));
#1006=EDGE_LOOP('',(#3661,#3662,#3663,#3664));
#1007=EDGE_LOOP('',(#3665,#3666,#3667,#3668,#3669,#3670,#3671));
#1008=EDGE_LOOP('',(#3672));
#1009=EDGE_LOOP('',(#3673,#3674,#3675,#3676));
#1010=EDGE_LOOP('',(#3677,#3678,#3679,#3680));
#1011=EDGE_LOOP('',(#3681,#3682,#3683,#3684));
#1012=EDGE_LOOP('',(#3685,#3686,#3687,#3688));
#1013=EDGE_LOOP('',(#3689,#3690,#3691,#3692));
#1014=EDGE_LOOP('',(#3693,#3694,#3695,#3696));
#1015=EDGE_LOOP('',(#3697,#3698,#3699,#3700));
#1016=EDGE_LOOP('',(#3701,#3702,#3703,#3704));
#1017=EDGE_LOOP('',(#3705));
#1018=EDGE_LOOP('',(#3706));
#1019=EDGE_LOOP('',(#3707));
#1020=EDGE_LOOP('',(#3708));
#1021=EDGE_LOOP('',(#3709,#3710,#3711,#3712));
#1022=EDGE_LOOP('',(#3713,#3714,#3715,#3716));
#1023=EDGE_LOOP('',(#3717,#3718,#3719,#3720));
#1024=EDGE_LOOP('',(#3721,#3722,#3723,#3724));
#1025=EDGE_LOOP('',(#3725,#3726,#3727,#3728));
#1026=EDGE_LOOP('',(#3729,#3730,#3731,#3732));
#1027=EDGE_LOOP('',(#3733,#3734,#3735,#3736));
#1028=EDGE_LOOP('',(#3737));
#1029=EDGE_LOOP('',(#3738));
#1030=EDGE_LOOP('',(#3739));
#1031=EDGE_LOOP('',(#3740));
#1032=EDGE_LOOP('',(#3741,#3742,#3743,#3744));
#1033=EDGE_LOOP('',(#3745,#3746,#3747,#3748));
#1034=EDGE_LOOP('',(#3749));
#1035=EDGE_LOOP('',(#3750));
#1036=EDGE_LOOP('',(#3751,#3752,#3753,#3754));
#1037=EDGE_LOOP('',(#3755));
#1038=EDGE_LOOP('',(#3756));
#1039=EDGE_LOOP('',(#3757));
#1040=EDGE_LOOP('',(#3758));
#1041=EDGE_LOOP('',(#3759,#3760,#3761,#3762));
#1042=EDGE_LOOP('',(#3763));
#1043=EDGE_LOOP('',(#3764));
#1044=EDGE_LOOP('',(#3765,#3766,#3767,#3768));
#1045=EDGE_LOOP('',(#3769));
#1046=EDGE_LOOP('',(#3770,#3771,#3772,#3773));
#1047=EDGE_LOOP('',(#3774));
#1048=EDGE_LOOP('',(#3775,#3776,#3777,#3778));
#1049=EDGE_LOOP('',(#3779,#3780,#3781,#3782));
#1050=EDGE_LOOP('',(#3783));
#1051=EDGE_LOOP('',(#3784));
#1052=EDGE_LOOP('',(#3785));
#1053=EDGE_LOOP('',(#3786));
#1054=EDGE_LOOP('',(#3787,#3788,#3789,#3790));
#1055=EDGE_LOOP('',(#3791,#3792,#3793,#3794));
#1056=EDGE_LOOP('',(#3795,#3796,#3797,#3798));
#1057=EDGE_LOOP('',(#3799,#3800,#3801,#3802));
#1058=EDGE_LOOP('',(#3803,#3804,#3805,#3806));
#1059=EDGE_LOOP('',(#3807,#3808,#3809,#3810));
#1060=LINE('',#5655,#1309);
#1061=LINE('',#5658,#1310);
#1062=LINE('',#5661,#1311);
#1063=LINE('',#5663,#1312);
#1064=LINE('',#5664,#1313);
#1065=LINE('',#5667,#1314);
#1066=LINE('',#5671,#1315);
#1067=LINE('',#5675,#1316);
#1068=LINE('',#5688,#1317);
#1069=LINE('',#5691,#1318);
#1070=LINE('',#5692,#1319);
#1071=LINE('',#5696,#1320);
#1072=LINE('',#5699,#1321);
#1073=LINE('',#5700,#1322);
#1074=LINE('',#5704,#1323);
#1075=LINE('',#5708,#1324);
#1076=LINE('',#5712,#1325);
#1077=LINE('',#5716,#1326);
#1078=LINE('',#5720,#1327);
#1079=LINE('',#5722,#1328);
#1080=LINE('',#5729,#1329);
#1081=LINE('',#5735,#1330);
#1082=LINE('',#5740,#1331);
#1083=LINE('',#5742,#1332);
#1084=LINE('',#5744,#1333);
#1085=LINE('',#5745,#1334);
#1086=LINE('',#5748,#1335);
#1087=LINE('',#5750,#1336);
#1088=LINE('',#5751,#1337);
#1089=LINE('',#5754,#1338);
#1090=LINE('',#5756,#1339);
#1091=LINE('',#5757,#1340);
#1092=LINE('',#5759,#1341);
#1093=LINE('',#5760,#1342);
#1094=LINE('',#5768,#1343);
#1095=LINE('',#5774,#1344);
#1096=LINE('',#5779,#1345);
#1097=LINE('',#5781,#1346);
#1098=LINE('',#5783,#1347);
#1099=LINE('',#5784,#1348);
#1100=LINE('',#5787,#1349);
#1101=LINE('',#5789,#1350);
#1102=LINE('',#5790,#1351);
#1103=LINE('',#5793,#1352);
#1104=LINE('',#5795,#1353);
#1105=LINE('',#5796,#1354);
#1106=LINE('',#5798,#1355);
#1107=LINE('',#5799,#1356);
#1108=LINE('',#5806,#1357);
#1109=LINE('',#5810,#1358);
#1110=LINE('',#5814,#1359);
#1111=LINE('',#5816,#1360);
#1112=LINE('',#5820,#1361);
#1113=LINE('',#5822,#1362);
#1114=LINE('',#5825,#1363);
#1115=LINE('',#5826,#1364);
#1116=LINE('',#5829,#1365);
#1117=LINE('',#5831,#1366);
#1118=LINE('',#5832,#1367);
#1119=LINE('',#5835,#1368);
#1120=LINE('',#5836,#1369);
#1121=LINE('',#5840,#1370);
#1122=LINE('',#5841,#1371);
#1123=LINE('',#5843,#1372);
#1124=LINE('',#5849,#1373);
#1125=LINE('',#5851,#1374);
#1126=LINE('',#5853,#1375);
#1127=LINE('',#5854,#1376);
#1128=LINE('',#5857,#1377);
#1129=LINE('',#5859,#1378);
#1130=LINE('',#5860,#1379);
#1131=LINE('',#5863,#1380);
#1132=LINE('',#5865,#1381);
#1133=LINE('',#5866,#1382);
#1134=LINE('',#5868,#1383);
#1135=LINE('',#5869,#1384);
#1136=LINE('',#5877,#1385);
#1137=LINE('',#5882,#1386);
#1138=LINE('',#5884,#1387);
#1139=LINE('',#5886,#1388);
#1140=LINE('',#5887,#1389);
#1141=LINE('',#5890,#1390);
#1142=LINE('',#5892,#1391);
#1143=LINE('',#5893,#1392);
#1144=LINE('',#5896,#1393);
#1145=LINE('',#5898,#1394);
#1146=LINE('',#5899,#1395);
#1147=LINE('',#5902,#1396);
#1148=LINE('',#5904,#1397);
#1149=LINE('',#5905,#1398);
#1150=LINE('',#5915,#1399);
#1151=LINE('',#6005,#1400);
#1152=LINE('',#6189,#1401);
#1153=LINE('',#6588,#1402);
#1154=LINE('',#6782,#1403);
#1155=LINE('',#7105,#1404);
#1156=LINE('',#7577,#1405);
#1157=LINE('',#8052,#1406);
#1158=LINE('',#8389,#1407);
#1159=LINE('',#8787,#1408);
#1160=LINE('',#9259,#1409);
#1161=LINE('',#9438,#1410);
#1162=LINE('',#9611,#1411);
#1163=LINE('',#9848,#1412);
#1164=LINE('',#10107,#1413);
#1165=LINE('',#10373,#1414);
#1166=LINE('',#10706,#1415);
#1167=LINE('',#10846,#1416);
#1168=LINE('',#11009,#1417);
#1169=LINE('',#11349,#1418);
#1170=LINE('',#11583,#1419);
#1171=LINE('',#11808,#1420);
#1172=LINE('',#14148,#1421);
#1173=LINE('',#14156,#1422);
#1174=LINE('',#14162,#1423);
#1175=LINE('',#14170,#1424);
#1176=LINE('',#14259,#1425);
#1177=LINE('',#14508,#1426);
#1178=LINE('',#14546,#1427);
#1179=LINE('',#15011,#1428);
#1180=LINE('',#15476,#1429);
#1181=LINE('',#15726,#1430);
#1182=LINE('',#15975,#1431);
#1183=LINE('',#16225,#1432);
#1184=LINE('',#16474,#1433);
#1185=LINE('',#16724,#1434);
#1186=LINE('',#17189,#1435);
#1187=LINE('',#17651,#1436);
#1188=LINE('',#17901,#1437);
#1189=LINE('',#18150,#1438);
#1190=LINE('',#18401,#1439);
#1191=LINE('',#18440,#1440);
#1192=LINE('',#18689,#1441);
#1193=LINE('',#18939,#1442);
#1194=LINE('',#19188,#1443);
#1195=LINE('',#19226,#1444);
#1196=LINE('',#19688,#1445);
#1197=LINE('',#19940,#1446);
#1198=LINE('',#20402,#1447);
#1199=LINE('',#20867,#1448);
#1200=LINE('',#21117,#1449);
#1201=LINE('',#21154,#1450);
#1202=LINE('',#21407,#1451);
#1203=LINE('',#21869,#1452);
#1204=LINE('',#22231,#1453);
#1205=LINE('',#22499,#1454);
#1206=LINE('',#23023,#1455);
#1207=LINE('',#23624,#1456);
#1208=LINE('',#24106,#1457);
#1209=LINE('',#24395,#1458);
#1210=LINE('',#24873,#1459);
#1211=LINE('',#25412,#1460);
#1212=LINE('',#25931,#1461);
#1213=LINE('',#26406,#1462);
#1214=LINE('',#26905,#1463);
#1215=LINE('',#27404,#1464);
#1216=LINE('',#27464,#1465);
#1217=LINE('',#27937,#1466);
#1218=LINE('',#28214,#1467);
#1219=LINE('',#28721,#1468);
#1220=LINE('',#29227,#1469);
#1221=LINE('',#29729,#1470);
#1222=LINE('',#30017,#1471);
#1223=LINE('',#30275,#1472);
#1224=LINE('',#30762,#1473);
#1225=LINE('',#31041,#1474);
#1226=LINE('',#31336,#1475);
#1227=LINE('',#31816,#1476);
#1228=LINE('',#32295,#1477);
#1229=LINE('',#32602,#1478);
#1230=LINE('',#33069,#1479);
#1231=LINE('',#37368,#1480);
#1232=LINE('',#37370,#1481);
#1233=LINE('',#37372,#1482);
#1234=LINE('',#37373,#1483);
#1235=LINE('',#37376,#1484);
#1236=LINE('',#37378,#1485);
#1237=LINE('',#37379,#1486);
#1238=LINE('',#37382,#1487);
#1239=LINE('',#37384,#1488);
#1240=LINE('',#37385,#1489);
#1241=LINE('',#37388,#1490);
#1242=LINE('',#37390,#1491);
#1243=LINE('',#37391,#1492);
#1244=LINE('',#37394,#1493);
#1245=LINE('',#37396,#1494);
#1246=LINE('',#37397,#1495);
#1247=LINE('',#37399,#1496);
#1248=LINE('',#37400,#1497);
#1249=LINE('',#37407,#1498);
#1250=LINE('',#37417,#1499);
#1251=LINE('',#37420,#1500);
#1252=LINE('',#37423,#1501);
#1253=LINE('',#37425,#1502);
#1254=LINE('',#37426,#1503);
#1255=LINE('',#37429,#1504);
#1256=LINE('',#37433,#1505);
#1257=LINE('',#37436,#1506);
#1258=LINE('',#37443,#1507);
#1259=LINE('',#37444,#1508);
#1260=LINE('',#37447,#1509);
#1261=LINE('',#37448,#1510);
#1262=LINE('',#37452,#1511);
#1263=LINE('',#37454,#1512);
#1264=LINE('',#37458,#1513);
#1265=LINE('',#37460,#1514);
#1266=LINE('',#37466,#1515);
#1267=LINE('',#37468,#1516);
#1268=LINE('',#37470,#1517);
#1269=LINE('',#37471,#1518);
#1270=LINE('',#37474,#1519);
#1271=LINE('',#37476,#1520);
#1272=LINE('',#37477,#1521);
#1273=LINE('',#37480,#1522);
#1274=LINE('',#37482,#1523);
#1275=LINE('',#37483,#1524);
#1276=LINE('',#37485,#1525);
#1277=LINE('',#37486,#1526);
#1278=LINE('',#37494,#1527);
#1279=LINE('',#37500,#1528);
#1280=LINE('',#37508,#1529);
#1281=LINE('',#37510,#1530);
#1282=LINE('',#37512,#1531);
#1283=LINE('',#37513,#1532);
#1284=LINE('',#37516,#1533);
#1285=LINE('',#37518,#1534);
#1286=LINE('',#37519,#1535);
#1287=LINE('',#37522,#1536);
#1288=LINE('',#37524,#1537);
#1289=LINE('',#37525,#1538);
#1290=LINE('',#37527,#1539);
#1291=LINE('',#37528,#1540);
#1292=LINE('',#37536,#1541);
#1293=LINE('',#37550,#1542);
#1294=LINE('',#37553,#1543);
#1295=LINE('',#37561,#1544);
#1296=LINE('',#37572,#1545);
#1297=LINE('',#37580,#1546);
#1298=LINE('',#37584,#1547);
#1299=LINE('',#37591,#1548);
#1300=LINE('',#37597,#1549);
#1301=LINE('',#37605,#1550);
#1302=LINE('',#37607,#1551);
#1303=LINE('',#37609,#1552);
#1304=LINE('',#37610,#1553);
#1305=LINE('',#37614,#1554);
#1306=LINE('',#37616,#1555);
#1307=LINE('',#37618,#1556);
#1308=LINE('',#37619,#1557);
#1309=VECTOR('',#4715,10.);
#1310=VECTOR('',#4718,10.);
#1311=VECTOR('',#4721,10.);
#1312=VECTOR('',#4722,10.);
#1313=VECTOR('',#4723,10.);
#1314=VECTOR('',#4726,10.);
#1315=VECTOR('',#4729,10.);
#1316=VECTOR('',#4732,10.);
#1317=VECTOR('',#4747,10.);
#1318=VECTOR('',#4750,10.);
#1319=VECTOR('',#4751,10.);
#1320=VECTOR('',#4756,10.);
#1321=VECTOR('',#4759,10.);
#1322=VECTOR('',#4760,10.);
#1323=VECTOR('',#4765,10.);
#1324=VECTOR('',#4770,4.5);
#1325=VECTOR('',#4775,4.5);
#1326=VECTOR('',#4780,4.5);
#1327=VECTOR('',#4785,4.5);
#1328=VECTOR('',#4788,10.);
#1329=VECTOR('',#4797,6.5);
#1330=VECTOR('',#4804,6.5);
#1331=VECTOR('',#4809,10.);
#1332=VECTOR('',#4810,10.);
#1333=VECTOR('',#4811,10.);
#1334=VECTOR('',#4812,10.);
#1335=VECTOR('',#4815,10.);
#1336=VECTOR('',#4816,10.);
#1337=VECTOR('',#4817,10.);
#1338=VECTOR('',#4820,10.);
#1339=VECTOR('',#4821,10.);
#1340=VECTOR('',#4822,10.);
#1341=VECTOR('',#4825,10.);
#1342=VECTOR('',#4826,10.);
#1343=VECTOR('',#4837,6.5);
#1344=VECTOR('',#4844,6.5);
#1345=VECTOR('',#4849,10.);
#1346=VECTOR('',#4850,10.);
#1347=VECTOR('',#4851,10.);
#1348=VECTOR('',#4852,10.);
#1349=VECTOR('',#4855,10.);
#1350=VECTOR('',#4856,10.);
#1351=VECTOR('',#4857,10.);
#1352=VECTOR('',#4860,10.);
#1353=VECTOR('',#4861,10.);
#1354=VECTOR('',#4862,10.);
#1355=VECTOR('',#4865,10.);
#1356=VECTOR('',#4866,10.);
#1357=VECTOR('',#4875,10.);
#1358=VECTOR('',#4878,10.);
#1359=VECTOR('',#4883,10.);
#1360=VECTOR('',#4884,10.);
#1361=VECTOR('',#4889,10.);
#1362=VECTOR('',#4890,10.);
#1363=VECTOR('',#4895,10.);
#1364=VECTOR('',#4896,10.);
#1365=VECTOR('',#4899,10.);
#1366=VECTOR('',#4900,10.);
#1367=VECTOR('',#4901,10.);
#1368=VECTOR('',#4904,10.);
#1369=VECTOR('',#4905,10.);
#1370=VECTOR('',#4910,10.);
#1371=VECTOR('',#4911,10.);
#1372=VECTOR('',#4914,10.);
#1373=VECTOR('',#4921,10.);
#1374=VECTOR('',#4922,10.);
#1375=VECTOR('',#4923,10.);
#1376=VECTOR('',#4924,10.);
#1377=VECTOR('',#4927,10.);
#1378=VECTOR('',#4928,10.);
#1379=VECTOR('',#4929,10.);
#1380=VECTOR('',#4932,10.);
#1381=VECTOR('',#4933,10.);
#1382=VECTOR('',#4934,10.);
#1383=VECTOR('',#4937,10.);
#1384=VECTOR('',#4938,10.);
#1385=VECTOR('',#4949,6.);
#1386=VECTOR('',#4954,10.);
#1387=VECTOR('',#4955,10.);
#1388=VECTOR('',#4956,10.);
#1389=VECTOR('',#4957,10.);
#1390=VECTOR('',#4960,10.);
#1391=VECTOR('',#4961,10.);
#1392=VECTOR('',#4962,10.);
#1393=VECTOR('',#4965,10.);
#1394=VECTOR('',#4966,10.);
#1395=VECTOR('',#4967,10.);
#1396=VECTOR('',#4970,10.);
#1397=VECTOR('',#4971,10.);
#1398=VECTOR('',#4972,10.);
#1399=VECTOR('',#4987,6.11325);
#1400=VECTOR('',#4992,6.11325);
#1401=VECTOR('',#4995,6.11325);
#1402=VECTOR('',#4998,6.11325);
#1403=VECTOR('',#5001,6.11325);
#1404=VECTOR('',#5004,6.11325);
#1405=VECTOR('',#5007,6.11325);
#1406=VECTOR('',#5010,6.11325);
#1407=VECTOR('',#5013,6.11325);
#1408=VECTOR('',#5016,6.11325);
#1409=VECTOR('',#5019,6.11325);
#1410=VECTOR('',#5024,5.13675);
#1411=VECTOR('',#5029,5.13675);
#1412=VECTOR('',#5032,5.13675);
#1413=VECTOR('',#5035,5.13675);
#1414=VECTOR('',#5038,5.13675);
#1415=VECTOR('',#5041,5.13675);
#1416=VECTOR('',#5044,5.13675);
#1417=VECTOR('',#5047,5.13675);
#1418=VECTOR('',#5050,5.13675);
#1419=VECTOR('',#5053,5.13675);
#1420=VECTOR('',#5056,5.13675);
#1421=VECTOR('',#5069,12.);
#1422=VECTOR('',#5080,6.5);
#1423=VECTOR('',#5087,12.);
#1424=VECTOR('',#5098,5.91675);
#1425=VECTOR('',#5103,5.91675);
#1426=VECTOR('',#5106,5.91675);
#1427=VECTOR('',#5109,5.91675);
#1428=VECTOR('',#5112,5.91675);
#1429=VECTOR('',#5115,5.91675);
#1430=VECTOR('',#5118,5.91675);
#1431=VECTOR('',#5121,5.91675);
#1432=VECTOR('',#5124,5.91675);
#1433=VECTOR('',#5127,5.91675);
#1434=VECTOR('',#5130,5.91675);
#1435=VECTOR('',#5133,5.91675);
#1436=VECTOR('',#5136,5.91675);
#1437=VECTOR('',#5139,5.91675);
#1438=VECTOR('',#5142,5.91675);
#1439=VECTOR('',#5145,5.91675);
#1440=VECTOR('',#5148,5.91675);
#1441=VECTOR('',#5151,5.91675);
#1442=VECTOR('',#5154,5.91675);
#1443=VECTOR('',#5157,5.91675);
#1444=VECTOR('',#5160,5.91675);
#1445=VECTOR('',#5163,5.91675);
#1446=VECTOR('',#5166,5.91675);
#1447=VECTOR('',#5169,5.91675);
#1448=VECTOR('',#5172,5.91675);
#1449=VECTOR('',#5175,5.91675);
#1450=VECTOR('',#5178,5.91675);
#1451=VECTOR('',#5181,5.91675);
#1452=VECTOR('',#5184,4.91825);
#1453=VECTOR('',#5189,4.91825);
#1454=VECTOR('',#5192,4.91825);
#1455=VECTOR('',#5195,4.91825);
#1456=VECTOR('',#5198,4.91825);
#1457=VECTOR('',#5201,4.91825);
#1458=VECTOR('',#5204,4.91825);
#1459=VECTOR('',#5207,4.91825);
#1460=VECTOR('',#5210,4.91825);
#1461=VECTOR('',#5213,4.91825);
#1462=VECTOR('',#5216,4.91825);
#1463=VECTOR('',#5219,4.91825);
#1464=VECTOR('',#5222,4.91825);
#1465=VECTOR('',#5225,4.91825);
#1466=VECTOR('',#5228,4.91825);
#1467=VECTOR('',#5231,4.91825);
#1468=VECTOR('',#5234,4.91825);
#1469=VECTOR('',#5237,4.91825);
#1470=VECTOR('',#5240,4.91825);
#1471=VECTOR('',#5243,4.91825);
#1472=VECTOR('',#5246,4.91825);
#1473=VECTOR('',#5249,4.91825);
#1474=VECTOR('',#5252,4.91825);
#1475=VECTOR('',#5255,4.91825);
#1476=VECTOR('',#5258,4.91825);
#1477=VECTOR('',#5261,4.91825);
#1478=VECTOR('',#5264,4.91825);
#1479=VECTOR('',#5267,4.91825);
#1480=VECTOR('',#5286,10.);
#1481=VECTOR('',#5287,10.);
#1482=VECTOR('',#5288,10.);
#1483=VECTOR('',#5289,10.);
#1484=VECTOR('',#5292,10.);
#1485=VECTOR('',#5293,10.);
#1486=VECTOR('',#5294,10.);
#1487=VECTOR('',#5297,9.99999999999999);
#1488=VECTOR('',#5298,10.);
#1489=VECTOR('',#5299,10.);
#1490=VECTOR('',#5302,10.);
#1491=VECTOR('',#5303,10.);
#1492=VECTOR('',#5304,10.);
#1493=VECTOR('',#5307,10.);
#1494=VECTOR('',#5308,10.);
#1495=VECTOR('',#5309,10.);
#1496=VECTOR('',#5312,10.);
#1497=VECTOR('',#5313,10.);
#1498=VECTOR('',#5322,9.);
#1499=VECTOR('',#5335,10.);
#1500=VECTOR('',#5338,10.);
#1501=VECTOR('',#5341,10.);
#1502=VECTOR('',#5342,10.);
#1503=VECTOR('',#5343,10.);
#1504=VECTOR('',#5346,10.);
#1505=VECTOR('',#5349,10.);
#1506=VECTOR('',#5352,10.);
#1507=VECTOR('',#5359,10.);
#1508=VECTOR('',#5360,10.);
#1509=VECTOR('',#5363,10.);
#1510=VECTOR('',#5364,10.);
#1511=VECTOR('',#5369,8.);
#1512=VECTOR('',#5372,10.);
#1513=VECTOR('',#5377,10.);
#1514=VECTOR('',#5380,10.);
#1515=VECTOR('',#5387,10.);
#1516=VECTOR('',#5388,10.);
#1517=VECTOR('',#5389,10.);
#1518=VECTOR('',#5390,10.);
#1519=VECTOR('',#5393,10.);
#1520=VECTOR('',#5394,10.);
#1521=VECTOR('',#5395,10.);
#1522=VECTOR('',#5398,10.);
#1523=VECTOR('',#5399,10.);
#1524=VECTOR('',#5400,10.);
#1525=VECTOR('',#5403,10.);
#1526=VECTOR('',#5404,10.);
#1527=VECTOR('',#5415,6.);
#1528=VECTOR('',#5422,8.);
#1529=VECTOR('',#5433,10.);
#1530=VECTOR('',#5434,10.);
#1531=VECTOR('',#5435,10.);
#1532=VECTOR('',#5436,10.);
#1533=VECTOR('',#5439,10.);
#1534=VECTOR('',#5440,10.);
#1535=VECTOR('',#5441,10.);
#1536=VECTOR('',#5444,10.);
#1537=VECTOR('',#5445,10.);
#1538=VECTOR('',#5446,10.);
#1539=VECTOR('',#5449,10.);
#1540=VECTOR('',#5450,10.);
#1541=VECTOR('',#5461,8.);
#1542=VECTOR('',#5482,8.);
#1543=VECTOR('',#5485,16.);
#1544=VECTOR('',#5496,5.);
#1545=VECTOR('',#5511,6.);
#1546=VECTOR('',#5520,9.);
#1547=VECTOR('',#5527,6.);
#1548=VECTOR('',#5536,6.);
#1549=VECTOR('',#5543,11.);
#1550=VECTOR('',#5554,10.);
#1551=VECTOR('',#5555,10.);
#1552=VECTOR('',#5556,10.);
#1553=VECTOR('',#5557,10.);
#1554=VECTOR('',#5560,10.);
#1555=VECTOR('',#5561,10.);
#1556=VECTOR('',#5562,10.);
#1557=VECTOR('',#5563,10.);
#1558=CIRCLE('',#4364,10.);
#1559=CIRCLE('',#4365,10.);
#1560=CIRCLE('',#4368,10.);
#1561=CIRCLE('',#4369,10.);
#1562=CIRCLE('',#4370,10.);
#1563=CIRCLE('',#4371,4.5);
#1564=CIRCLE('',#4372,4.5);
#1565=CIRCLE('',#4373,4.5);
#1566=CIRCLE('',#4374,4.5);
#1567=CIRCLE('',#4376,10.);
#1568=CIRCLE('',#4379,10.);
#1569=CIRCLE('',#4382,10.);
#1570=CIRCLE('',#4384,4.5);
#1571=CIRCLE('',#4386,4.5);
#1572=CIRCLE('',#4388,4.5);
#1573=CIRCLE('',#4390,4.5);
#1574=CIRCLE('',#4395,6.5);
#1575=CIRCLE('',#4396,6.5);
#1576=CIRCLE('',#4398,6.5);
#1577=CIRCLE('',#4399,6.5);
#1578=CIRCLE('',#4408,6.5);
#1579=CIRCLE('',#4409,6.5);
#1580=CIRCLE('',#4411,6.5);
#1581=CIRCLE('',#4412,6.5);
#1582=CIRCLE('',#4443,6.);
#1583=CIRCLE('',#4444,6.);
#1584=CIRCLE('',#4450,12.);
#1585=CIRCLE('',#4451,12.);
#1586=CIRCLE('',#4456,6.11325);
#1587=CIRCLE('',#4467,6.11325);
#1588=CIRCLE('',#4469,5.13675);
#1589=CIRCLE('',#4480,5.13675);
#1590=CIRCLE('',#4484,12.);
#1591=CIRCLE('',#4486,12.);
#1592=CIRCLE('',#4490,6.5);
#1593=CIRCLE('',#4491,6.5);
#1594=CIRCLE('',#4493,12.);
#1595=CIRCLE('',#4494,12.);
#1596=CIRCLE('',#4499,5.91675);
#1597=CIRCLE('',#4528,4.91825);
#1598=CIRCLE('',#4557,4.91825);
#1599=CIRCLE('',#4559,5.91675);
#1600=CIRCLE('',#4561,5.);
#1601=CIRCLE('',#4572,9.);
#1602=CIRCLE('',#4574,9.);
#1603=CIRCLE('',#4579,5.);
#1604=CIRCLE('',#4580,5.);
#1605=CIRCLE('',#4583,5.);
#1606=CIRCLE('',#4584,12.);
#1607=CIRCLE('',#4585,8.);
#1608=CIRCLE('',#4587,5.);
#1609=CIRCLE('',#4590,8.);
#1610=CIRCLE('',#4593,12.);
#1611=CIRCLE('',#4605,6.);
#1612=CIRCLE('',#4606,6.);
#1613=CIRCLE('',#4608,8.);
#1614=CIRCLE('',#4609,8.);
#1615=CIRCLE('',#4621,8.);
#1616=CIRCLE('',#4622,8.);
#1617=CIRCLE('',#4627,8.);
#1618=CIRCLE('',#4629,16.);
#1619=CIRCLE('',#4631,8.);
#1620=CIRCLE('',#4633,16.);
#1621=CIRCLE('',#4637,5.);
#1622=CIRCLE('',#4638,5.);
#1623=CIRCLE('',#4640,6.);
#1624=CIRCLE('',#4642,6.);
#1625=CIRCLE('',#4644,6.);
#1626=CIRCLE('',#4646,9.);
#1627=CIRCLE('',#4647,6.);
#1628=CIRCLE('',#4649,9.);
#1629=CIRCLE('',#4655,6.);
#1630=CIRCLE('',#4656,6.);
#1631=CIRCLE('',#4658,11.);
#1632=CIRCLE('',#4659,11.);
#1633=CIRCLE('',#4666,9.);
#1634=CIRCLE('',#4667,5.);
#1635=CIRCLE('',#4669,5.);
#1636=CIRCLE('',#4671,9.);
#1637=VERTEX_POINT('',#5651);
#1638=VERTEX_POINT('',#5652);
#1639=VERTEX_POINT('',#5654);
#1640=VERTEX_POINT('',#5656);
#1641=VERTEX_POINT('',#5660);
#1642=VERTEX_POINT('',#5662);
#1643=VERTEX_POINT('',#5666);
#1644=VERTEX_POINT('',#5668);
#1645=VERTEX_POINT('',#5670);
#1646=VERTEX_POINT('',#5672);
#1647=VERTEX_POINT('',#5674);
#1648=VERTEX_POINT('',#5677);
#1649=VERTEX_POINT('',#5679);
#1650=VERTEX_POINT('',#5681);
#1651=VERTEX_POINT('',#5683);
#1652=VERTEX_POINT('',#5686);
#1653=VERTEX_POINT('',#5690);
#1654=VERTEX_POINT('',#5694);
#1655=VERTEX_POINT('',#5698);
#1656=VERTEX_POINT('',#5702);
#1657=VERTEX_POINT('',#5706);
#1658=VERTEX_POINT('',#5710);
#1659=VERTEX_POINT('',#5714);
#1660=VERTEX_POINT('',#5718);
#1661=VERTEX_POINT('',#5726);
#1662=VERTEX_POINT('',#5728);
#1663=VERTEX_POINT('',#5732);
#1664=VERTEX_POINT('',#5734);
#1665=VERTEX_POINT('',#5738);
#1666=VERTEX_POINT('',#5739);
#1667=VERTEX_POINT('',#5741);
#1668=VERTEX_POINT('',#5743);
#1669=VERTEX_POINT('',#5747);
#1670=VERTEX_POINT('',#5749);
#1671=VERTEX_POINT('',#5753);
#1672=VERTEX_POINT('',#5755);
#1673=VERTEX_POINT('',#5765);
#1674=VERTEX_POINT('',#5767);
#1675=VERTEX_POINT('',#5771);
#1676=VERTEX_POINT('',#5773);
#1677=VERTEX_POINT('',#5777);
#1678=VERTEX_POINT('',#5778);
#1679=VERTEX_POINT('',#5780);
#1680=VERTEX_POINT('',#5782);
#1681=VERTEX_POINT('',#5786);
#1682=VERTEX_POINT('',#5788);
#1683=VERTEX_POINT('',#5792);
#1684=VERTEX_POINT('',#5794);
#1685=VERTEX_POINT('',#5804);
#1686=VERTEX_POINT('',#5805);
#1687=VERTEX_POINT('',#5807);
#1688=VERTEX_POINT('',#5809);
#1689=VERTEX_POINT('',#5813);
#1690=VERTEX_POINT('',#5815);
#1691=VERTEX_POINT('',#5819);
#1692=VERTEX_POINT('',#5821);
#1693=VERTEX_POINT('',#5828);
#1694=VERTEX_POINT('',#5830);
#1695=VERTEX_POINT('',#5834);
#1696=VERTEX_POINT('',#5839);
#1697=VERTEX_POINT('',#5847);
#1698=VERTEX_POINT('',#5848);
#1699=VERTEX_POINT('',#5850);
#1700=VERTEX_POINT('',#5852);
#1701=VERTEX_POINT('',#5856);
#1702=VERTEX_POINT('',#5858);
#1703=VERTEX_POINT('',#5862);
#1704=VERTEX_POINT('',#5864);
#1705=VERTEX_POINT('',#5874);
#1706=VERTEX_POINT('',#5876);
#1707=VERTEX_POINT('',#5880);
#1708=VERTEX_POINT('',#5881);
#1709=VERTEX_POINT('',#5883);
#1710=VERTEX_POINT('',#5885);
#1711=VERTEX_POINT('',#5889);
#1712=VERTEX_POINT('',#5891);
#1713=VERTEX_POINT('',#5895);
#1714=VERTEX_POINT('',#5897);
#1715=VERTEX_POINT('',#5901);
#1716=VERTEX_POINT('',#5903);
#1717=VERTEX_POINT('',#5913);
#1718=VERTEX_POINT('',#5914);
#1719=VERTEX_POINT('',#5916);
#1720=VERTEX_POINT('',#5929);
#1721=VERTEX_POINT('',#5935);
#1722=VERTEX_POINT('',#5937);
#1723=VERTEX_POINT('',#6003);
#1724=VERTEX_POINT('',#6004);
#1725=VERTEX_POINT('',#6006);
#1726=VERTEX_POINT('',#6164);
#1727=VERTEX_POINT('',#6187);
#1728=VERTEX_POINT('',#6188);
#1729=VERTEX_POINT('',#6190);
#1730=VERTEX_POINT('',#6427);
#1731=VERTEX_POINT('',#6586);
#1732=VERTEX_POINT('',#6587);
#1733=VERTEX_POINT('',#6589);
#1734=VERTEX_POINT('',#6684);
#1735=VERTEX_POINT('',#6780);
#1736=VERTEX_POINT('',#6781);
#1737=VERTEX_POINT('',#6783);
#1738=VERTEX_POINT('',#6944);
#1739=VERTEX_POINT('',#7103);
#1740=VERTEX_POINT('',#7104);
#1741=VERTEX_POINT('',#7106);
#1742=VERTEX_POINT('',#7340);
#1743=VERTEX_POINT('',#7575);
#1744=VERTEX_POINT('',#7576);
#1745=VERTEX_POINT('',#7578);
#1746=VERTEX_POINT('',#7812);
#1747=VERTEX_POINT('',#8050);
#1748=VERTEX_POINT('',#8051);
#1749=VERTEX_POINT('',#8053);
#1750=VERTEX_POINT('',#8152);
#1751=VERTEX_POINT('',#8387);
#1752=VERTEX_POINT('',#8388);
#1753=VERTEX_POINT('',#8390);
#1754=VERTEX_POINT('',#8547);
#1755=VERTEX_POINT('',#8785);
#1756=VERTEX_POINT('',#8786);
#1757=VERTEX_POINT('',#8788);
#1758=VERTEX_POINT('',#9025);
#1759=VERTEX_POINT('',#9257);
#1760=VERTEX_POINT('',#9258);
#1761=VERTEX_POINT('',#9260);
#1762=VERTEX_POINT('',#9270);
#1763=VERTEX_POINT('',#9277);
#1764=VERTEX_POINT('',#9279);
#1765=VERTEX_POINT('',#9436);
#1766=VERTEX_POINT('',#9437);
#1767=VERTEX_POINT('',#9439);
#1768=VERTEX_POINT('',#9508);
#1769=VERTEX_POINT('',#9609);
#1770=VERTEX_POINT('',#9610);
#1771=VERTEX_POINT('',#9612);
#1772=VERTEX_POINT('',#9738);
#1773=VERTEX_POINT('',#9846);
#1774=VERTEX_POINT('',#9847);
#1775=VERTEX_POINT('',#9849);
#1776=VERTEX_POINT('',#10066);
#1777=VERTEX_POINT('',#10105);
#1778=VERTEX_POINT('',#10106);
#1779=VERTEX_POINT('',#10108);
#1780=VERTEX_POINT('',#10149);
#1781=VERTEX_POINT('',#10371);
#1782=VERTEX_POINT('',#10372);
#1783=VERTEX_POINT('',#10374);
#1784=VERTEX_POINT('',#10704);
#1785=VERTEX_POINT('',#10705);
#1786=VERTEX_POINT('',#10707);
#1787=VERTEX_POINT('',#10735);
#1788=VERTEX_POINT('',#10844);
#1789=VERTEX_POINT('',#10845);
#1790=VERTEX_POINT('',#10965);
#1791=VERTEX_POINT('',#11007);
#1792=VERTEX_POINT('',#11008);
#1793=VERTEX_POINT('',#11010);
#1794=VERTEX_POINT('',#11125);
#1795=VERTEX_POINT('',#11347);
#1796=VERTEX_POINT('',#11348);
#1797=VERTEX_POINT('',#11581);
#1798=VERTEX_POINT('',#11582);
#1799=VERTEX_POINT('',#11584);
#1800=VERTEX_POINT('',#11701);
#1801=VERTEX_POINT('',#11806);
#1802=VERTEX_POINT('',#11807);
#1803=VERTEX_POINT('',#11809);
#1804=VERTEX_POINT('',#11931);
#1805=VERTEX_POINT('',#12132);
#1806=VERTEX_POINT('',#12175);
#1807=VERTEX_POINT('',#12406);
#1808=VERTEX_POINT('',#13105);
#1809=VERTEX_POINT('',#14032);
#1810=VERTEX_POINT('',#14144);
#1811=VERTEX_POINT('',#14147);
#1812=VERTEX_POINT('',#14153);
#1813=VERTEX_POINT('',#14155);
#1814=VERTEX_POINT('',#14159);
#1815=VERTEX_POINT('',#14161);
#1816=VERTEX_POINT('',#14168);
#1817=VERTEX_POINT('',#14169);
#1818=VERTEX_POINT('',#14171);
#1819=VERTEX_POINT('',#14248);
#1820=VERTEX_POINT('',#14257);
#1821=VERTEX_POINT('',#14258);
#1822=VERTEX_POINT('',#14506);
#1823=VERTEX_POINT('',#14507);
#1824=VERTEX_POINT('',#14544);
#1825=VERTEX_POINT('',#14545);
#1826=VERTEX_POINT('',#15009);
#1827=VERTEX_POINT('',#15010);
#1828=VERTEX_POINT('',#15474);
#1829=VERTEX_POINT('',#15475);
#1830=VERTEX_POINT('',#15724);
#1831=VERTEX_POINT('',#15725);
#1832=VERTEX_POINT('',#15973);
#1833=VERTEX_POINT('',#15974);
#1834=VERTEX_POINT('',#16223);
#1835=VERTEX_POINT('',#16224);
#1836=VERTEX_POINT('',#16472);
#1837=VERTEX_POINT('',#16473);
#1838=VERTEX_POINT('',#16722);
#1839=VERTEX_POINT('',#16723);
#1840=VERTEX_POINT('',#17187);
#1841=VERTEX_POINT('',#17188);
#1842=VERTEX_POINT('',#17649);
#1843=VERTEX_POINT('',#17650);
#1844=VERTEX_POINT('',#17899);
#1845=VERTEX_POINT('',#17900);
#1846=VERTEX_POINT('',#18148);
#1847=VERTEX_POINT('',#18149);
#1848=VERTEX_POINT('',#18399);
#1849=VERTEX_POINT('',#18400);
#1850=VERTEX_POINT('',#18438);
#1851=VERTEX_POINT('',#18439);
#1852=VERTEX_POINT('',#18687);
#1853=VERTEX_POINT('',#18688);
#1854=VERTEX_POINT('',#18937);
#1855=VERTEX_POINT('',#18938);
#1856=VERTEX_POINT('',#19186);
#1857=VERTEX_POINT('',#19187);
#1858=VERTEX_POINT('',#19224);
#1859=VERTEX_POINT('',#19225);
#1860=VERTEX_POINT('',#19686);
#1861=VERTEX_POINT('',#19687);
#1862=VERTEX_POINT('',#19938);
#1863=VERTEX_POINT('',#19939);
#1864=VERTEX_POINT('',#20400);
#1865=VERTEX_POINT('',#20401);
#1866=VERTEX_POINT('',#20865);
#1867=VERTEX_POINT('',#20866);
#1868=VERTEX_POINT('',#21115);
#1869=VERTEX_POINT('',#21116);
#1870=VERTEX_POINT('',#21152);
#1871=VERTEX_POINT('',#21153);
#1872=VERTEX_POINT('',#21405);
#1873=VERTEX_POINT('',#21406);
#1874=VERTEX_POINT('',#21867);
#1875=VERTEX_POINT('',#21868);
#1876=VERTEX_POINT('',#21870);
#1877=VERTEX_POINT('',#22087);
#1878=VERTEX_POINT('',#22229);
#1879=VERTEX_POINT('',#22230);
#1880=VERTEX_POINT('',#22466);
#1881=VERTEX_POINT('',#22497);
#1882=VERTEX_POINT('',#22498);
#1883=VERTEX_POINT('',#22500);
#1884=VERTEX_POINT('',#22795);
#1885=VERTEX_POINT('',#23021);
#1886=VERTEX_POINT('',#23022);
#1887=VERTEX_POINT('',#23326);
#1888=VERTEX_POINT('',#23622);
#1889=VERTEX_POINT('',#23623);
#1890=VERTEX_POINT('',#23625);
#1891=VERTEX_POINT('',#24104);
#1892=VERTEX_POINT('',#24105);
#1893=VERTEX_POINT('',#24107);
#1894=VERTEX_POINT('',#24365);
#1895=VERTEX_POINT('',#24393);
#1896=VERTEX_POINT('',#24394);
#1897=VERTEX_POINT('',#24632);
#1898=VERTEX_POINT('',#24871);
#1899=VERTEX_POINT('',#24872);
#1900=VERTEX_POINT('',#24874);
#1901=VERTEX_POINT('',#25410);
#1902=VERTEX_POINT('',#25411);
#1903=VERTEX_POINT('',#25665);
#1904=VERTEX_POINT('',#25929);
#1905=VERTEX_POINT('',#25930);
#1906=VERTEX_POINT('',#25932);
#1907=VERTEX_POINT('',#26404);
#1908=VERTEX_POINT('',#26405);
#1909=VERTEX_POINT('',#26659);
#1910=VERTEX_POINT('',#26903);
#1911=VERTEX_POINT('',#26904);
#1912=VERTEX_POINT('',#26906);
#1913=VERTEX_POINT('',#27402);
#1914=VERTEX_POINT('',#27403);
#1915=VERTEX_POINT('',#27405);
#1916=VERTEX_POINT('',#27432);
#1917=VERTEX_POINT('',#27462);
#1918=VERTEX_POINT('',#27463);
#1919=VERTEX_POINT('',#27465);
#1920=VERTEX_POINT('',#27708);
#1921=VERTEX_POINT('',#27935);
#1922=VERTEX_POINT('',#27936);
#1923=VERTEX_POINT('',#28184);
#1924=VERTEX_POINT('',#28212);
#1925=VERTEX_POINT('',#28213);
#1926=VERTEX_POINT('',#28215);
#1927=VERTEX_POINT('',#28466);
#1928=VERTEX_POINT('',#28719);
#1929=VERTEX_POINT('',#28720);
#1930=VERTEX_POINT('',#29225);
#1931=VERTEX_POINT('',#29226);
#1932=VERTEX_POINT('',#29228);
#1933=VERTEX_POINT('',#29495);
#1934=VERTEX_POINT('',#29727);
#1935=VERTEX_POINT('',#29728);
#1936=VERTEX_POINT('',#29984);
#1937=VERTEX_POINT('',#30015);
#1938=VERTEX_POINT('',#30016);
#1939=VERTEX_POINT('',#30018);
#1940=VERTEX_POINT('',#30047);
#1941=VERTEX_POINT('',#30273);
#1942=VERTEX_POINT('',#30274);
#1943=VERTEX_POINT('',#30276);
#1944=VERTEX_POINT('',#30502);
#1945=VERTEX_POINT('',#30760);
#1946=VERTEX_POINT('',#30761);
#1947=VERTEX_POINT('',#30763);
#1948=VERTEX_POINT('',#31039);
#1949=VERTEX_POINT('',#31040);
#1950=VERTEX_POINT('',#31042);
#1951=VERTEX_POINT('',#31304);
#1952=VERTEX_POINT('',#31334);
#1953=VERTEX_POINT('',#31335);
#1954=VERTEX_POINT('',#31579);
#1955=VERTEX_POINT('',#31814);
#1956=VERTEX_POINT('',#31815);
#1957=VERTEX_POINT('',#31817);
#1958=VERTEX_POINT('',#32293);
#1959=VERTEX_POINT('',#32294);
#1960=VERTEX_POINT('',#32296);
#1961=VERTEX_POINT('',#32326);
#1962=VERTEX_POINT('',#32600);
#1963=VERTEX_POINT('',#32601);
#1964=VERTEX_POINT('',#32603);
#1965=VERTEX_POINT('',#33067);
#1966=VERTEX_POINT('',#33068);
#1967=VERTEX_POINT('',#33316);
#1968=VERTEX_POINT('',#33346);
#1969=VERTEX_POINT('',#33352);
#1970=VERTEX_POINT('',#33564);
#1971=VERTEX_POINT('',#33566);
#1972=VERTEX_POINT('',#33744);
#1973=VERTEX_POINT('',#33760);
#1974=VERTEX_POINT('',#33932);
#1975=VERTEX_POINT('',#34204);
#1976=VERTEX_POINT('',#37247);
#1977=VERTEX_POINT('',#37366);
#1978=VERTEX_POINT('',#37367);
#1979=VERTEX_POINT('',#37369);
#1980=VERTEX_POINT('',#37371);
#1981=VERTEX_POINT('',#37375);
#1982=VERTEX_POINT('',#37377);
#1983=VERTEX_POINT('',#37381);
#1984=VERTEX_POINT('',#37383);
#1985=VERTEX_POINT('',#37387);
#1986=VERTEX_POINT('',#37389);
#1987=VERTEX_POINT('',#37393);
#1988=VERTEX_POINT('',#37395);
#1989=VERTEX_POINT('',#37403);
#1990=VERTEX_POINT('',#37406);
#1991=VERTEX_POINT('',#37413);
#1992=VERTEX_POINT('',#37414);
#1993=VERTEX_POINT('',#37416);
#1994=VERTEX_POINT('',#37418);
#1995=VERTEX_POINT('',#37422);
#1996=VERTEX_POINT('',#37424);
#1997=VERTEX_POINT('',#37428);
#1998=VERTEX_POINT('',#37430);
#1999=VERTEX_POINT('',#37432);
#2000=VERTEX_POINT('',#37434);
#2001=VERTEX_POINT('',#37437);
#2002=VERTEX_POINT('',#37440);
#2003=VERTEX_POINT('',#37441);
#2004=VERTEX_POINT('',#37446);
#2005=VERTEX_POINT('',#37450);
#2006=VERTEX_POINT('',#37456);
#2007=VERTEX_POINT('',#37464);
#2008=VERTEX_POINT('',#37465);
#2009=VERTEX_POINT('',#37467);
#2010=VERTEX_POINT('',#37469);
#2011=VERTEX_POINT('',#37473);
#2012=VERTEX_POINT('',#37475);
#2013=VERTEX_POINT('',#37479);
#2014=VERTEX_POINT('',#37481);
#2015=VERTEX_POINT('',#37491);
#2016=VERTEX_POINT('',#37493);
#2017=VERTEX_POINT('',#37497);
#2018=VERTEX_POINT('',#37499);
#2019=VERTEX_POINT('',#37506);
#2020=VERTEX_POINT('',#37507);
#2021=VERTEX_POINT('',#37509);
#2022=VERTEX_POINT('',#37511);
#2023=VERTEX_POINT('',#37515);
#2024=VERTEX_POINT('',#37517);
#2025=VERTEX_POINT('',#37521);
#2026=VERTEX_POINT('',#37523);
#2027=VERTEX_POINT('',#37533);
#2028=VERTEX_POINT('',#37535);
#2029=VERTEX_POINT('',#37542);
#2030=VERTEX_POINT('',#37545);
#2031=VERTEX_POINT('',#37548);
#2032=VERTEX_POINT('',#37552);
#2033=VERTEX_POINT('',#37558);
#2034=VERTEX_POINT('',#37560);
#2035=VERTEX_POINT('',#37564);
#2036=VERTEX_POINT('',#37567);
#2037=VERTEX_POINT('',#37570);
#2038=VERTEX_POINT('',#37574);
#2039=VERTEX_POINT('',#37576);
#2040=VERTEX_POINT('',#37579);
#2041=VERTEX_POINT('',#37588);
#2042=VERTEX_POINT('',#37590);
#2043=VERTEX_POINT('',#37594);
#2044=VERTEX_POINT('',#37596);
#2045=VERTEX_POINT('',#37603);
#2046=VERTEX_POINT('',#37604);
#2047=VERTEX_POINT('',#37606);
#2048=VERTEX_POINT('',#37608);
#2049=VERTEX_POINT('',#37612);
#2050=VERTEX_POINT('',#37613);
#2051=VERTEX_POINT('',#37615);
#2052=VERTEX_POINT('',#37617);
#2053=EDGE_CURVE('',#1637,#1638,#1558,.T.);
#2054=EDGE_CURVE('',#1638,#1639,#1060,.T.);
#2055=EDGE_CURVE('',#1639,#1640,#1559,.T.);
#2056=EDGE_CURVE('',#1640,#1637,#1061,.T.);
#2057=EDGE_CURVE('',#1640,#1641,#1062,.F.);
#2058=EDGE_CURVE('',#1642,#1641,#1063,.T.);
#2059=EDGE_CURVE('',#1637,#1642,#1064,.F.);
#2060=EDGE_CURVE('',#1643,#1639,#1065,.F.);
#2061=EDGE_CURVE('',#1644,#1643,#1560,.T.);
#2062=EDGE_CURVE('',#1645,#1644,#1066,.F.);
#2063=EDGE_CURVE('',#1646,#1645,#1561,.T.);
#2064=EDGE_CURVE('',#1647,#1646,#1067,.F.);
#2065=EDGE_CURVE('',#1641,#1647,#1562,.T.);
#2066=EDGE_CURVE('',#1648,#1648,#1563,.T.);
#2067=EDGE_CURVE('',#1649,#1649,#1564,.T.);
#2068=EDGE_CURVE('',#1650,#1650,#1565,.T.);
#2069=EDGE_CURVE('',#1651,#1651,#1566,.T.);
#2070=EDGE_CURVE('',#1652,#1642,#1567,.T.);
#2071=EDGE_CURVE('',#1647,#1652,#1068,.T.);
#2072=EDGE_CURVE('',#1653,#1646,#1069,.T.);
#2073=EDGE_CURVE('',#1652,#1653,#1070,.F.);
#2074=EDGE_CURVE('',#1654,#1653,#1568,.T.);
#2075=EDGE_CURVE('',#1645,#1654,#1071,.T.);
#2076=EDGE_CURVE('',#1655,#1644,#1072,.T.);
#2077=EDGE_CURVE('',#1654,#1655,#1073,.F.);
#2078=EDGE_CURVE('',#1656,#1655,#1569,.T.);
#2079=EDGE_CURVE('',#1643,#1656,#1074,.T.);
#2080=EDGE_CURVE('',#1657,#1657,#1570,.T.);
#2081=EDGE_CURVE('',#1657,#1648,#1075,.T.);
#2082=EDGE_CURVE('',#1658,#1658,#1571,.T.);
#2083=EDGE_CURVE('',#1658,#1649,#1076,.T.);
#2084=EDGE_CURVE('',#1659,#1659,#1572,.T.);
#2085=EDGE_CURVE('',#1659,#1650,#1077,.T.);
#2086=EDGE_CURVE('',#1660,#1660,#1573,.T.);
#2087=EDGE_CURVE('',#1660,#1651,#1078,.T.);
#2088=EDGE_CURVE('',#1656,#1638,#1079,.F.);
#2089=EDGE_CURVE('',#1661,#1661,#1574,.T.);
#2090=EDGE_CURVE('',#1661,#1662,#1080,.T.);
#2091=EDGE_CURVE('',#1662,#1662,#1575,.T.);
#2092=EDGE_CURVE('',#1663,#1663,#1576,.T.);
#2093=EDGE_CURVE('',#1663,#1664,#1081,.T.);
#2094=EDGE_CURVE('',#1664,#1664,#1577,.T.);
#2095=EDGE_CURVE('',#1665,#1666,#1082,.T.);
#2096=EDGE_CURVE('',#1666,#1667,#1083,.T.);
#2097=EDGE_CURVE('',#1668,#1667,#1084,.T.);
#2098=EDGE_CURVE('',#1665,#1668,#1085,.T.);
#2099=EDGE_CURVE('',#1669,#1665,#1086,.T.);
#2100=EDGE_CURVE('',#1670,#1668,#1087,.T.);
#2101=EDGE_CURVE('',#1669,#1670,#1088,.T.);
#2102=EDGE_CURVE('',#1671,#1669,#1089,.T.);
#2103=EDGE_CURVE('',#1672,#1670,#1090,.T.);
#2104=EDGE_CURVE('',#1671,#1672,#1091,.T.);
#2105=EDGE_CURVE('',#1666,#1671,#1092,.T.);
#2106=EDGE_CURVE('',#1667,#1672,#1093,.T.);
#2107=EDGE_CURVE('',#1673,#1673,#1578,.T.);
#2108=EDGE_CURVE('',#1673,#1674,#1094,.T.);
#2109=EDGE_CURVE('',#1674,#1674,#1579,.T.);
#2110=EDGE_CURVE('',#1675,#1675,#1580,.T.);
#2111=EDGE_CURVE('',#1675,#1676,#1095,.T.);
#2112=EDGE_CURVE('',#1676,#1676,#1581,.T.);
#2113=EDGE_CURVE('',#1677,#1678,#1096,.T.);
#2114=EDGE_CURVE('',#1677,#1679,#1097,.T.);
#2115=EDGE_CURVE('',#1680,#1679,#1098,.T.);
#2116=EDGE_CURVE('',#1678,#1680,#1099,.T.);
#2117=EDGE_CURVE('',#1678,#1681,#1100,.T.);
#2118=EDGE_CURVE('',#1682,#1680,#1101,.T.);
#2119=EDGE_CURVE('',#1681,#1682,#1102,.T.);
#2120=EDGE_CURVE('',#1681,#1683,#1103,.T.);
#2121=EDGE_CURVE('',#1684,#1682,#1104,.T.);
#2122=EDGE_CURVE('',#1683,#1684,#1105,.T.);
#2123=EDGE_CURVE('',#1683,#1677,#1106,.T.);
#2124=EDGE_CURVE('',#1679,#1684,#1107,.T.);
#2125=EDGE_CURVE('',#1685,#1686,#1108,.T.);
#2126=EDGE_CURVE('',#1686,#1687,#404,.T.);
#2127=EDGE_CURVE('',#1687,#1688,#1109,.T.);
#2128=EDGE_CURVE('',#1688,#1685,#405,.T.);
#2129=EDGE_CURVE('',#1689,#1687,#1110,.T.);
#2130=EDGE_CURVE('',#1686,#1690,#1111,.T.);
#2131=EDGE_CURVE('',#1690,#1689,#406,.T.);
#2132=EDGE_CURVE('',#1691,#1685,#1112,.T.);
#2133=EDGE_CURVE('',#1688,#1692,#1113,.T.);
#2134=EDGE_CURVE('',#1692,#1691,#407,.T.);
#2135=EDGE_CURVE('',#1692,#1689,#1114,.T.);
#2136=EDGE_CURVE('',#1690,#1691,#1115,.T.);
#2137=EDGE_CURVE('',#1688,#1693,#1116,.T.);
#2138=EDGE_CURVE('',#1693,#1694,#1117,.T.);
#2139=EDGE_CURVE('',#1692,#1694,#1118,.T.);
#2140=EDGE_CURVE('',#1695,#1687,#1119,.T.);
#2141=EDGE_CURVE('',#1693,#1695,#1120,.T.);
#2142=EDGE_CURVE('',#1696,#1689,#1121,.T.);
#2143=EDGE_CURVE('',#1695,#1696,#1122,.T.);
#2144=EDGE_CURVE('',#1694,#1696,#1123,.T.);
#2145=EDGE_CURVE('',#1697,#1698,#1124,.T.);
#2146=EDGE_CURVE('',#1698,#1699,#1125,.T.);
#2147=EDGE_CURVE('',#1700,#1699,#1126,.T.);
#2148=EDGE_CURVE('',#1697,#1700,#1127,.T.);
#2149=EDGE_CURVE('',#1701,#1697,#1128,.T.);
#2150=EDGE_CURVE('',#1702,#1700,#1129,.T.);
#2151=EDGE_CURVE('',#1701,#1702,#1130,.T.);
#2152=EDGE_CURVE('',#1703,#1701,#1131,.T.);
#2153=EDGE_CURVE('',#1704,#1702,#1132,.T.);
#2154=EDGE_CURVE('',#1703,#1704,#1133,.T.);
#2155=EDGE_CURVE('',#1698,#1703,#1134,.T.);
#2156=EDGE_CURVE('',#1699,#1704,#1135,.T.);
#2157=EDGE_CURVE('',#1705,#1705,#1582,.T.);
#2158=EDGE_CURVE('',#1705,#1706,#1136,.T.);
#2159=EDGE_CURVE('',#1706,#1706,#1583,.T.);
#2160=EDGE_CURVE('',#1707,#1708,#1137,.T.);
#2161=EDGE_CURVE('',#1707,#1709,#1138,.T.);
#2162=EDGE_CURVE('',#1710,#1709,#1139,.T.);
#2163=EDGE_CURVE('',#1708,#1710,#1140,.T.);
#2164=EDGE_CURVE('',#1708,#1711,#1141,.T.);
#2165=EDGE_CURVE('',#1712,#1710,#1142,.T.);
#2166=EDGE_CURVE('',#1711,#1712,#1143,.T.);
#2167=EDGE_CURVE('',#1711,#1713,#1144,.T.);
#2168=EDGE_CURVE('',#1714,#1712,#1145,.T.);
#2169=EDGE_CURVE('',#1713,#1714,#1146,.T.);
#2170=EDGE_CURVE('',#1713,#1715,#1147,.T.);
#2171=EDGE_CURVE('',#1716,#1714,#1148,.T.);
#2172=EDGE_CURVE('',#1715,#1716,#1149,.T.);
#2173=EDGE_CURVE('',#1707,#1715,#1584,.T.);
#2174=EDGE_CURVE('',#1709,#1716,#1585,.T.);
#2175=EDGE_CURVE('',#1717,#1718,#1150,.T.);
#2176=EDGE_CURVE('',#1718,#1719,#152,.T.);
#2177=EDGE_CURVE('',#1719,#1720,#153,.T.);
#2178=EDGE_CURVE('',#1721,#1720,#1586,.T.);
#2179=EDGE_CURVE('',#1722,#1721,#154,.T.);
#2180=EDGE_CURVE('',#1717,#1722,#155,.T.);
#2181=EDGE_CURVE('',#1723,#1724,#1151,.T.);
#2182=EDGE_CURVE('',#1724,#1725,#156,.T.);
#2183=EDGE_CURVE('',#1725,#1718,#157,.T.);
#2184=EDGE_CURVE('',#1726,#1717,#158,.T.);
#2185=EDGE_CURVE('',#1723,#1726,#159,.T.);
#2186=EDGE_CURVE('',#1727,#1728,#1152,.T.);
#2187=EDGE_CURVE('',#1728,#1729,#160,.T.);
#2188=EDGE_CURVE('',#1729,#1724,#161,.T.);
#2189=EDGE_CURVE('',#1730,#1723,#162,.T.);
#2190=EDGE_CURVE('',#1727,#1730,#163,.T.);
#2191=EDGE_CURVE('',#1731,#1732,#1153,.T.);
#2192=EDGE_CURVE('',#1732,#1733,#164,.T.);
#2193=EDGE_CURVE('',#1733,#1728,#165,.T.);
#2194=EDGE_CURVE('',#1734,#1727,#166,.T.);
#2195=EDGE_CURVE('',#1731,#1734,#167,.T.);
#2196=EDGE_CURVE('',#1735,#1736,#1154,.T.);
#2197=EDGE_CURVE('',#1736,#1737,#168,.T.);
#2198=EDGE_CURVE('',#1737,#1732,#169,.T.);
#2199=EDGE_CURVE('',#1738,#1731,#170,.T.);
#2200=EDGE_CURVE('',#1735,#1738,#171,.T.);
#2201=EDGE_CURVE('',#1739,#1740,#1155,.T.);
#2202=EDGE_CURVE('',#1740,#1741,#172,.T.);
#2203=EDGE_CURVE('',#1741,#1736,#173,.T.);
#2204=EDGE_CURVE('',#1742,#1735,#174,.T.);
#2205=EDGE_CURVE('',#1739,#1742,#175,.T.);
#2206=EDGE_CURVE('',#1743,#1744,#1156,.T.);
#2207=EDGE_CURVE('',#1744,#1745,#176,.T.);
#2208=EDGE_CURVE('',#1745,#1740,#177,.T.);
#2209=EDGE_CURVE('',#1746,#1739,#178,.T.);
#2210=EDGE_CURVE('',#1743,#1746,#179,.T.);
#2211=EDGE_CURVE('',#1747,#1748,#1157,.T.);
#2212=EDGE_CURVE('',#1748,#1749,#180,.T.);
#2213=EDGE_CURVE('',#1749,#1744,#181,.T.);
#2214=EDGE_CURVE('',#1750,#1743,#182,.T.);
#2215=EDGE_CURVE('',#1747,#1750,#183,.T.);
#2216=EDGE_CURVE('',#1751,#1752,#1158,.T.);
#2217=EDGE_CURVE('',#1752,#1753,#184,.T.);
#2218=EDGE_CURVE('',#1753,#1748,#185,.T.);
#2219=EDGE_CURVE('',#1754,#1747,#186,.T.);
#2220=EDGE_CURVE('',#1751,#1754,#187,.T.);
#2221=EDGE_CURVE('',#1755,#1756,#1159,.T.);
#2222=EDGE_CURVE('',#1756,#1757,#188,.T.);
#2223=EDGE_CURVE('',#1757,#1752,#189,.T.);
#2224=EDGE_CURVE('',#1758,#1751,#190,.T.);
#2225=EDGE_CURVE('',#1755,#1758,#191,.T.);
#2226=EDGE_CURVE('',#1759,#1760,#1160,.T.);
#2227=EDGE_CURVE('',#1761,#1759,#192,.T.);
#2228=EDGE_CURVE('',#1762,#1761,#193,.T.);
#2229=EDGE_CURVE('',#1763,#1762,#1587,.T.);
#2230=EDGE_CURVE('',#1763,#1764,#194,.T.);
#2231=EDGE_CURVE('',#1764,#1760,#195,.T.);
#2232=EDGE_CURVE('',#1765,#1766,#1161,.T.);
#2233=EDGE_CURVE('',#1766,#1767,#196,.F.);
#2234=EDGE_CURVE('',#1768,#1767,#1588,.F.);
#2235=EDGE_CURVE('',#1768,#1765,#197,.T.);
#2236=EDGE_CURVE('',#1769,#1770,#1162,.T.);
#2237=EDGE_CURVE('',#1770,#1771,#198,.T.);
#2238=EDGE_CURVE('',#1771,#1766,#199,.F.);
#2239=EDGE_CURVE('',#1765,#1772,#200,.T.);
#2240=EDGE_CURVE('',#1772,#1769,#201,.T.);
#2241=EDGE_CURVE('',#1773,#1774,#1163,.T.);
#2242=EDGE_CURVE('',#1774,#1775,#202,.T.);
#2243=EDGE_CURVE('',#1775,#1770,#203,.T.);
#2244=EDGE_CURVE('',#1769,#1776,#204,.T.);
#2245=EDGE_CURVE('',#1776,#1773,#205,.T.);
#2246=EDGE_CURVE('',#1777,#1778,#1164,.T.);
#2247=EDGE_CURVE('',#1778,#1779,#206,.T.);
#2248=EDGE_CURVE('',#1779,#1774,#207,.T.);
#2249=EDGE_CURVE('',#1773,#1780,#208,.T.);
#2250=EDGE_CURVE('',#1780,#1777,#209,.T.);
#2251=EDGE_CURVE('',#1781,#1782,#1165,.T.);
#2252=EDGE_CURVE('',#1782,#1783,#210,.T.);
#2253=EDGE_CURVE('',#1783,#1778,#211,.T.);
#2254=EDGE_CURVE('',#1777,#1781,#212,.T.);
#2255=EDGE_CURVE('',#1784,#1785,#1166,.T.);
#2256=EDGE_CURVE('',#1785,#1786,#213,.T.);
#2257=EDGE_CURVE('',#1786,#1782,#214,.T.);
#2258=EDGE_CURVE('',#1781,#1787,#215,.T.);
#2259=EDGE_CURVE('',#1787,#1784,#216,.T.);
#2260=EDGE_CURVE('',#1788,#1789,#1167,.T.);
#2261=EDGE_CURVE('',#1789,#1785,#217,.T.);
#2262=EDGE_CURVE('',#1784,#1790,#218,.T.);
#2263=EDGE_CURVE('',#1790,#1788,#219,.T.);
#2264=EDGE_CURVE('',#1791,#1792,#1168,.T.);
#2265=EDGE_CURVE('',#1792,#1793,#220,.T.);
#2266=EDGE_CURVE('',#1793,#1789,#221,.T.);
#2267=EDGE_CURVE('',#1788,#1794,#222,.T.);
#2268=EDGE_CURVE('',#1794,#1791,#223,.T.);
#2269=EDGE_CURVE('',#1795,#1796,#1169,.T.);
#2270=EDGE_CURVE('',#1796,#1792,#224,.T.);
#2271=EDGE_CURVE('',#1791,#1795,#225,.T.);
#2272=EDGE_CURVE('',#1797,#1798,#1170,.T.);
#2273=EDGE_CURVE('',#1798,#1799,#226,.T.);
#2274=EDGE_CURVE('',#1799,#1796,#227,.T.);
#2275=EDGE_CURVE('',#1795,#1800,#228,.T.);
#2276=EDGE_CURVE('',#1800,#1797,#229,.T.);
#2277=EDGE_CURVE('',#1801,#1802,#1171,.T.);
#2278=EDGE_CURVE('',#1801,#1803,#230,.T.);
#2279=EDGE_CURVE('',#1803,#1804,#1589,.F.);
#2280=EDGE_CURVE('',#1804,#1802,#231,.T.);
#2281=EDGE_CURVE('',#1802,#1798,#232,.T.);
#2282=EDGE_CURVE('',#1797,#1805,#233,.T.);
#2283=EDGE_CURVE('',#1805,#1801,#234,.T.);
#2284=EDGE_CURVE('',#1760,#1806,#235,.T.);
#2285=EDGE_CURVE('',#1806,#1756,#236,.T.);
#2286=EDGE_CURVE('',#1807,#1755,#237,.T.);
#2287=EDGE_CURVE('',#1759,#1807,#238,.T.);
#2288=EDGE_CURVE('',#1720,#1808,#239,.T.);
#2289=EDGE_CURVE('',#1803,#1763,#240,.T.);
#2290=EDGE_CURVE('',#1808,#1768,#241,.T.);
#2291=EDGE_CURVE('',#1767,#1721,#242,.T.);
#2292=EDGE_CURVE('',#1804,#1809,#243,.T.);
#2293=EDGE_CURVE('',#1762,#1809,#244,.T.);
#2294=EDGE_CURVE('',#1810,#1810,#1590,.T.);
#2295=EDGE_CURVE('',#1810,#1811,#1172,.T.);
#2296=EDGE_CURVE('',#1811,#1811,#1591,.T.);
#2297=EDGE_CURVE('',#1812,#1812,#1592,.T.);
#2298=EDGE_CURVE('',#1812,#1813,#1173,.T.);
#2299=EDGE_CURVE('',#1813,#1813,#1593,.T.);
#2300=EDGE_CURVE('',#1814,#1814,#1594,.T.);
#2301=EDGE_CURVE('',#1814,#1815,#1174,.T.);
#2302=EDGE_CURVE('',#1815,#1815,#1595,.T.);
#2303=EDGE_CURVE('',#1816,#1817,#1175,.T.);
#2304=EDGE_CURVE('',#1816,#1818,#245,.T.);
#2305=EDGE_CURVE('',#1818,#1819,#1596,.F.);
#2306=EDGE_CURVE('',#1819,#1817,#246,.T.);
#2307=EDGE_CURVE('',#1820,#1821,#1176,.T.);
#2308=EDGE_CURVE('',#1820,#1816,#247,.T.);
#2309=EDGE_CURVE('',#1817,#1821,#248,.T.);
#2310=EDGE_CURVE('',#1822,#1823,#1177,.T.);
#2311=EDGE_CURVE('',#1822,#1820,#249,.T.);
#2312=EDGE_CURVE('',#1821,#1823,#250,.T.);
#2313=EDGE_CURVE('',#1824,#1825,#1178,.T.);
#2314=EDGE_CURVE('',#1824,#1822,#251,.T.);
#2315=EDGE_CURVE('',#1823,#1825,#252,.T.);
#2316=EDGE_CURVE('',#1826,#1827,#1179,.T.);
#2317=EDGE_CURVE('',#1826,#1824,#253,.T.);
#2318=EDGE_CURVE('',#1825,#1827,#254,.T.);
#2319=EDGE_CURVE('',#1828,#1829,#1180,.T.);
#2320=EDGE_CURVE('',#1828,#1826,#255,.T.);
#2321=EDGE_CURVE('',#1827,#1829,#256,.T.);
#2322=EDGE_CURVE('',#1830,#1831,#1181,.T.);
#2323=EDGE_CURVE('',#1830,#1828,#257,.T.);
#2324=EDGE_CURVE('',#1829,#1831,#258,.T.);
#2325=EDGE_CURVE('',#1832,#1833,#1182,.T.);
#2326=EDGE_CURVE('',#1832,#1830,#259,.T.);
#2327=EDGE_CURVE('',#1831,#1833,#260,.T.);
#2328=EDGE_CURVE('',#1834,#1835,#1183,.T.);
#2329=EDGE_CURVE('',#1834,#1832,#261,.T.);
#2330=EDGE_CURVE('',#1833,#1835,#262,.T.);
#2331=EDGE_CURVE('',#1836,#1837,#1184,.T.);
#2332=EDGE_CURVE('',#1836,#1834,#263,.T.);
#2333=EDGE_CURVE('',#1835,#1837,#264,.T.);
#2334=EDGE_CURVE('',#1838,#1839,#1185,.T.);
#2335=EDGE_CURVE('',#1838,#1836,#265,.T.);
#2336=EDGE_CURVE('',#1837,#1839,#266,.T.);
#2337=EDGE_CURVE('',#1840,#1841,#1186,.T.);
#2338=EDGE_CURVE('',#1840,#1838,#267,.T.);
#2339=EDGE_CURVE('',#1839,#1841,#268,.T.);
#2340=EDGE_CURVE('',#1842,#1843,#1187,.T.);
#2341=EDGE_CURVE('',#1842,#1840,#269,.T.);
#2342=EDGE_CURVE('',#1841,#1843,#270,.T.);
#2343=EDGE_CURVE('',#1844,#1845,#1188,.T.);
#2344=EDGE_CURVE('',#1844,#1842,#271,.T.);
#2345=EDGE_CURVE('',#1843,#1845,#272,.T.);
#2346=EDGE_CURVE('',#1846,#1847,#1189,.T.);
#2347=EDGE_CURVE('',#1846,#1844,#273,.T.);
#2348=EDGE_CURVE('',#1845,#1847,#274,.T.);
#2349=EDGE_CURVE('',#1848,#1849,#1190,.T.);
#2350=EDGE_CURVE('',#1848,#1846,#275,.T.);
#2351=EDGE_CURVE('',#1847,#1849,#276,.T.);
#2352=EDGE_CURVE('',#1850,#1851,#1191,.T.);
#2353=EDGE_CURVE('',#1850,#1848,#277,.T.);
#2354=EDGE_CURVE('',#1849,#1851,#278,.T.);
#2355=EDGE_CURVE('',#1852,#1853,#1192,.T.);
#2356=EDGE_CURVE('',#1852,#1850,#279,.T.);
#2357=EDGE_CURVE('',#1851,#1853,#280,.T.);
#2358=EDGE_CURVE('',#1854,#1855,#1193,.T.);
#2359=EDGE_CURVE('',#1854,#1852,#281,.T.);
#2360=EDGE_CURVE('',#1853,#1855,#282,.T.);
#2361=EDGE_CURVE('',#1856,#1857,#1194,.T.);
#2362=EDGE_CURVE('',#1856,#1854,#283,.T.);
#2363=EDGE_CURVE('',#1855,#1857,#284,.T.);
#2364=EDGE_CURVE('',#1858,#1859,#1195,.T.);
#2365=EDGE_CURVE('',#1858,#1856,#285,.T.);
#2366=EDGE_CURVE('',#1857,#1859,#286,.T.);
#2367=EDGE_CURVE('',#1860,#1861,#1196,.T.);
#2368=EDGE_CURVE('',#1860,#1858,#287,.T.);
#2369=EDGE_CURVE('',#1859,#1861,#288,.T.);
#2370=EDGE_CURVE('',#1862,#1863,#1197,.T.);
#2371=EDGE_CURVE('',#1862,#1860,#289,.T.);
#2372=EDGE_CURVE('',#1861,#1863,#290,.T.);
#2373=EDGE_CURVE('',#1864,#1865,#1198,.T.);
#2374=EDGE_CURVE('',#1864,#1862,#291,.T.);
#2375=EDGE_CURVE('',#1863,#1865,#292,.T.);
#2376=EDGE_CURVE('',#1866,#1867,#1199,.T.);
#2377=EDGE_CURVE('',#1866,#1864,#293,.T.);
#2378=EDGE_CURVE('',#1865,#1867,#294,.T.);
#2379=EDGE_CURVE('',#1868,#1869,#1200,.T.);
#2380=EDGE_CURVE('',#1868,#1866,#295,.T.);
#2381=EDGE_CURVE('',#1867,#1869,#296,.T.);
#2382=EDGE_CURVE('',#1870,#1871,#1201,.T.);
#2383=EDGE_CURVE('',#1870,#1868,#297,.T.);
#2384=EDGE_CURVE('',#1869,#1871,#298,.T.);
#2385=EDGE_CURVE('',#1872,#1873,#1202,.T.);
#2386=EDGE_CURVE('',#1872,#1870,#299,.T.);
#2387=EDGE_CURVE('',#1871,#1873,#300,.T.);
#2388=EDGE_CURVE('',#1874,#1875,#1203,.T.);
#2389=EDGE_CURVE('',#1876,#1874,#301,.F.);
#2390=EDGE_CURVE('',#1877,#1876,#1597,.T.);
#2391=EDGE_CURVE('',#1877,#1875,#302,.T.);
#2392=EDGE_CURVE('',#1878,#1879,#1204,.T.);
#2393=EDGE_CURVE('',#1874,#1878,#303,.F.);
#2394=EDGE_CURVE('',#1875,#1880,#304,.T.);
#2395=EDGE_CURVE('',#1880,#1879,#305,.T.);
#2396=EDGE_CURVE('',#1881,#1882,#1205,.T.);
#2397=EDGE_CURVE('',#1883,#1881,#306,.F.);
#2398=EDGE_CURVE('',#1878,#1883,#307,.F.);
#2399=EDGE_CURVE('',#1879,#1884,#308,.T.);
#2400=EDGE_CURVE('',#1884,#1882,#309,.T.);
#2401=EDGE_CURVE('',#1885,#1886,#1206,.T.);
#2402=EDGE_CURVE('',#1881,#1885,#310,.F.);
#2403=EDGE_CURVE('',#1882,#1887,#311,.T.);
#2404=EDGE_CURVE('',#1887,#1886,#312,.T.);
#2405=EDGE_CURVE('',#1888,#1889,#1207,.T.);
#2406=EDGE_CURVE('',#1890,#1888,#313,.T.);
#2407=EDGE_CURVE('',#1885,#1890,#314,.F.);
#2408=EDGE_CURVE('',#1886,#1889,#315,.T.);
#2409=EDGE_CURVE('',#1891,#1892,#1208,.T.);
#2410=EDGE_CURVE('',#1893,#1891,#316,.F.);
#2411=EDGE_CURVE('',#1888,#1893,#317,.T.);
#2412=EDGE_CURVE('',#1889,#1894,#318,.T.);
#2413=EDGE_CURVE('',#1894,#1892,#319,.T.);
#2414=EDGE_CURVE('',#1895,#1896,#1209,.T.);
#2415=EDGE_CURVE('',#1891,#1895,#320,.F.);
#2416=EDGE_CURVE('',#1892,#1897,#321,.T.);
#2417=EDGE_CURVE('',#1897,#1896,#322,.T.);
#2418=EDGE_CURVE('',#1898,#1899,#1210,.T.);
#2419=EDGE_CURVE('',#1900,#1898,#323,.F.);
#2420=EDGE_CURVE('',#1895,#1900,#324,.F.);
#2421=EDGE_CURVE('',#1896,#1899,#325,.T.);
#2422=EDGE_CURVE('',#1901,#1902,#1211,.T.);
#2423=EDGE_CURVE('',#1898,#1901,#326,.F.);
#2424=EDGE_CURVE('',#1899,#1903,#327,.T.);
#2425=EDGE_CURVE('',#1903,#1902,#328,.T.);
#2426=EDGE_CURVE('',#1904,#1905,#1212,.T.);
#2427=EDGE_CURVE('',#1906,#1904,#329,.F.);
#2428=EDGE_CURVE('',#1901,#1906,#330,.F.);
#2429=EDGE_CURVE('',#1902,#1905,#331,.T.);
#2430=EDGE_CURVE('',#1907,#1908,#1213,.T.);
#2431=EDGE_CURVE('',#1904,#1907,#332,.F.);
#2432=EDGE_CURVE('',#1905,#1909,#333,.T.);
#2433=EDGE_CURVE('',#1909,#1908,#334,.T.);
#2434=EDGE_CURVE('',#1910,#1911,#1214,.T.);
#2435=EDGE_CURVE('',#1912,#1910,#335,.T.);
#2436=EDGE_CURVE('',#1907,#1912,#336,.F.);
#2437=EDGE_CURVE('',#1908,#1911,#337,.T.);
#2438=EDGE_CURVE('',#1913,#1914,#1215,.T.);
#2439=EDGE_CURVE('',#1915,#1913,#338,.T.);
#2440=EDGE_CURVE('',#1910,#1915,#339,.T.);
#2441=EDGE_CURVE('',#1911,#1916,#340,.T.);
#2442=EDGE_CURVE('',#1916,#1914,#341,.T.);
#2443=EDGE_CURVE('',#1917,#1918,#1216,.T.);
#2444=EDGE_CURVE('',#1919,#1917,#342,.F.);
#2445=EDGE_CURVE('',#1913,#1919,#343,.T.);
#2446=EDGE_CURVE('',#1914,#1920,#344,.T.);
#2447=EDGE_CURVE('',#1920,#1918,#345,.T.);
#2448=EDGE_CURVE('',#1921,#1922,#1217,.T.);
#2449=EDGE_CURVE('',#1917,#1921,#346,.F.);
#2450=EDGE_CURVE('',#1918,#1923,#347,.T.);
#2451=EDGE_CURVE('',#1923,#1922,#348,.T.);
#2452=EDGE_CURVE('',#1924,#1925,#1218,.T.);
#2453=EDGE_CURVE('',#1926,#1924,#349,.F.);
#2454=EDGE_CURVE('',#1921,#1926,#350,.F.);
#2455=EDGE_CURVE('',#1922,#1927,#351,.T.);
#2456=EDGE_CURVE('',#1927,#1925,#352,.T.);
#2457=EDGE_CURVE('',#1928,#1929,#1219,.T.);
#2458=EDGE_CURVE('',#1924,#1928,#353,.F.);
#2459=EDGE_CURVE('',#1925,#1929,#354,.T.);
#2460=EDGE_CURVE('',#1930,#1931,#1220,.T.);
#2461=EDGE_CURVE('',#1932,#1930,#355,.F.);
#2462=EDGE_CURVE('',#1928,#1932,#356,.F.);
#2463=EDGE_CURVE('',#1929,#1933,#357,.T.);
#2464=EDGE_CURVE('',#1933,#1931,#358,.T.);
#2465=EDGE_CURVE('',#1934,#1935,#1221,.T.);
#2466=EDGE_CURVE('',#1930,#1934,#359,.F.);
#2467=EDGE_CURVE('',#1931,#1936,#360,.T.);
#2468=EDGE_CURVE('',#1936,#1935,#361,.T.);
#2469=EDGE_CURVE('',#1937,#1938,#1222,.T.);
#2470=EDGE_CURVE('',#1939,#1937,#362,.T.);
#2471=EDGE_CURVE('',#1934,#1939,#363,.F.);
#2472=EDGE_CURVE('',#1935,#1940,#364,.T.);
#2473=EDGE_CURVE('',#1940,#1938,#365,.T.);
#2474=EDGE_CURVE('',#1941,#1942,#1223,.T.);
#2475=EDGE_CURVE('',#1943,#1941,#366,.T.);
#2476=EDGE_CURVE('',#1937,#1943,#367,.T.);
#2477=EDGE_CURVE('',#1938,#1944,#368,.T.);
#2478=EDGE_CURVE('',#1944,#1942,#369,.T.);
#2479=EDGE_CURVE('',#1945,#1946,#1224,.T.);
#2480=EDGE_CURVE('',#1947,#1945,#370,.T.);
#2481=EDGE_CURVE('',#1941,#1947,#371,.T.);
#2482=EDGE_CURVE('',#1942,#1946,#372,.T.);
#2483=EDGE_CURVE('',#1948,#1949,#1225,.T.);
#2484=EDGE_CURVE('',#1950,#1948,#373,.F.);
#2485=EDGE_CURVE('',#1945,#1950,#374,.T.);
#2486=EDGE_CURVE('',#1946,#1951,#375,.T.);
#2487=EDGE_CURVE('',#1951,#1949,#376,.T.);
#2488=EDGE_CURVE('',#1952,#1953,#1226,.T.);
#2489=EDGE_CURVE('',#1948,#1952,#377,.F.);
#2490=EDGE_CURVE('',#1949,#1954,#378,.T.);
#2491=EDGE_CURVE('',#1954,#1953,#379,.T.);
#2492=EDGE_CURVE('',#1955,#1956,#1227,.T.);
#2493=EDGE_CURVE('',#1957,#1955,#380,.T.);
#2494=EDGE_CURVE('',#1952,#1957,#381,.F.);
#2495=EDGE_CURVE('',#1953,#1956,#382,.T.);
#2496=EDGE_CURVE('',#1958,#1959,#1228,.T.);
#2497=EDGE_CURVE('',#1960,#1958,#383,.T.);
#2498=EDGE_CURVE('',#1955,#1960,#384,.T.);
#2499=EDGE_CURVE('',#1956,#1961,#385,.T.);
#2500=EDGE_CURVE('',#1961,#1959,#386,.T.);
#2501=EDGE_CURVE('',#1962,#1963,#1229,.T.);
#2502=EDGE_CURVE('',#1964,#1962,#387,.F.);
#2503=EDGE_CURVE('',#1958,#1964,#388,.T.);
#2504=EDGE_CURVE('',#1959,#1963,#389,.T.);
#2505=EDGE_CURVE('',#1965,#1966,#1230,.T.);
#2506=EDGE_CURVE('',#1962,#1965,#390,.F.);
#2507=EDGE_CURVE('',#1963,#1967,#391,.T.);
#2508=EDGE_CURVE('',#1967,#1966,#392,.T.);
#2509=EDGE_CURVE('',#1966,#1968,#393,.T.);
#2510=EDGE_CURVE('',#1968,#1969,#394,.T.);
#2511=EDGE_CURVE('',#1970,#1969,#1598,.T.);
#2512=EDGE_CURVE('',#1971,#1970,#395,.T.);
#2513=EDGE_CURVE('',#1965,#1971,#396,.F.);
#2514=EDGE_CURVE('',#1873,#1972,#397,.T.);
#2515=EDGE_CURVE('',#1972,#1973,#1599,.T.);
#2516=EDGE_CURVE('',#1973,#1872,#398,.T.);
#2517=EDGE_CURVE('',#1974,#1972,#399,.T.);
#2518=EDGE_CURVE('',#1975,#1974,#1600,.T.);
#2519=EDGE_CURVE('',#1973,#1975,#400,.T.);
#2520=EDGE_CURVE('',#1969,#1975,#408,.T.);
#2521=EDGE_CURVE('',#1818,#1877,#401,.T.);
#2522=EDGE_CURVE('',#1976,#1819,#402,.T.);
#2523=EDGE_CURVE('',#1976,#1876,#403,.T.);
#2524=EDGE_CURVE('',#1974,#1970,#409,.T.);
#2525=EDGE_CURVE('',#1977,#1978,#1231,.T.);
#2526=EDGE_CURVE('',#1977,#1979,#1232,.T.);
#2527=EDGE_CURVE('',#1979,#1980,#1233,.T.);
#2528=EDGE_CURVE('',#1978,#1980,#1234,.T.);
#2529=EDGE_CURVE('',#1981,#1977,#1235,.T.);
#2530=EDGE_CURVE('',#1981,#1982,#1236,.T.);
#2531=EDGE_CURVE('',#1982,#1979,#1237,.T.);
#2532=EDGE_CURVE('',#1983,#1981,#1238,.T.);
#2533=EDGE_CURVE('',#1983,#1984,#1239,.T.);
#2534=EDGE_CURVE('',#1984,#1982,#1240,.T.);
#2535=EDGE_CURVE('',#1985,#1983,#1241,.T.);
#2536=EDGE_CURVE('',#1985,#1986,#1242,.T.);
#2537=EDGE_CURVE('',#1986,#1984,#1243,.T.);
#2538=EDGE_CURVE('',#1987,#1985,#1244,.T.);
#2539=EDGE_CURVE('',#1987,#1988,#1245,.T.);
#2540=EDGE_CURVE('',#1988,#1986,#1246,.T.);
#2541=EDGE_CURVE('',#1978,#1987,#1247,.T.);
#2542=EDGE_CURVE('',#1980,#1988,#1248,.T.);
#2543=EDGE_CURVE('',#1989,#1989,#1601,.T.);
#2544=EDGE_CURVE('',#1989,#1990,#1249,.T.);
#2545=EDGE_CURVE('',#1990,#1990,#1602,.T.);
#2546=EDGE_CURVE('',#1991,#1992,#1603,.T.);
#2547=EDGE_CURVE('',#1992,#1993,#1250,.T.);
#2548=EDGE_CURVE('',#1993,#1994,#1604,.T.);
#2549=EDGE_CURVE('',#1994,#1991,#1251,.T.);
#2550=EDGE_CURVE('',#1994,#1995,#1252,.T.);
#2551=EDGE_CURVE('',#1995,#1996,#1253,.T.);
#2552=EDGE_CURVE('',#1991,#1996,#1254,.T.);
#2553=EDGE_CURVE('',#1997,#1993,#1255,.T.);
#2554=EDGE_CURVE('',#1998,#1997,#1605,.T.);
#2555=EDGE_CURVE('',#1999,#1998,#1256,.T.);
#2556=EDGE_CURVE('',#2000,#1999,#1606,.T.);
#2557=EDGE_CURVE('',#1995,#2000,#1257,.T.);
#2558=EDGE_CURVE('',#2001,#2001,#1607,.T.);
#2559=EDGE_CURVE('',#2002,#2003,#1608,.T.);
#2560=EDGE_CURVE('',#2003,#1998,#1258,.T.);
#2561=EDGE_CURVE('',#1997,#2002,#1259,.T.);
#2562=EDGE_CURVE('',#2004,#2003,#1260,.T.);
#2563=EDGE_CURVE('',#1999,#2004,#1261,.T.);
#2564=EDGE_CURVE('',#2005,#2005,#1609,.T.);
#2565=EDGE_CURVE('',#2005,#2001,#1262,.T.);
#2566=EDGE_CURVE('',#2002,#1992,#1263,.T.);
#2567=EDGE_CURVE('',#2006,#2004,#1610,.T.);
#2568=EDGE_CURVE('',#2000,#2006,#1264,.T.);
#2569=EDGE_CURVE('',#1996,#2006,#1265,.T.);
#2570=EDGE_CURVE('',#2007,#2008,#1266,.T.);
#2571=EDGE_CURVE('',#2008,#2009,#1267,.T.);
#2572=EDGE_CURVE('',#2010,#2009,#1268,.T.);
#2573=EDGE_CURVE('',#2007,#2010,#1269,.T.);
#2574=EDGE_CURVE('',#2011,#2007,#1270,.T.);
#2575=EDGE_CURVE('',#2012,#2010,#1271,.T.);
#2576=EDGE_CURVE('',#2011,#2012,#1272,.T.);
#2577=EDGE_CURVE('',#2013,#2011,#1273,.T.);
#2578=EDGE_CURVE('',#2014,#2012,#1274,.T.);
#2579=EDGE_CURVE('',#2013,#2014,#1275,.T.);
#2580=EDGE_CURVE('',#2008,#2013,#1276,.T.);
#2581=EDGE_CURVE('',#2009,#2014,#1277,.T.);
#2582=EDGE_CURVE('',#2015,#2015,#1611,.T.);
#2583=EDGE_CURVE('',#2015,#2016,#1278,.T.);
#2584=EDGE_CURVE('',#2016,#2016,#1612,.T.);
#2585=EDGE_CURVE('',#2017,#2017,#1613,.T.);
#2586=EDGE_CURVE('',#2017,#2018,#1279,.T.);
#2587=EDGE_CURVE('',#2018,#2018,#1614,.T.);
#2588=EDGE_CURVE('',#2019,#2020,#1280,.T.);
#2589=EDGE_CURVE('',#2020,#2021,#1281,.T.);
#2590=EDGE_CURVE('',#2022,#2021,#1282,.T.);
#2591=EDGE_CURVE('',#2019,#2022,#1283,.T.);
#2592=EDGE_CURVE('',#2023,#2019,#1284,.T.);
#2593=EDGE_CURVE('',#2024,#2022,#1285,.T.);
#2594=EDGE_CURVE('',#2023,#2024,#1286,.T.);
#2595=EDGE_CURVE('',#2025,#2023,#1287,.T.);
#2596=EDGE_CURVE('',#2026,#2024,#1288,.T.);
#2597=EDGE_CURVE('',#2025,#2026,#1289,.T.);
#2598=EDGE_CURVE('',#2020,#2025,#1290,.T.);
#2599=EDGE_CURVE('',#2021,#2026,#1291,.T.);
#2600=EDGE_CURVE('',#2027,#2027,#1615,.T.);
#2601=EDGE_CURVE('',#2027,#2028,#1292,.T.);
#2602=EDGE_CURVE('',#2028,#2028,#1616,.T.);
#2603=EDGE_CURVE('',#2029,#2029,#1617,.T.);
#2604=EDGE_CURVE('',#2030,#2030,#1618,.F.);
#2605=EDGE_CURVE('',#2031,#2031,#1619,.T.);
#2606=EDGE_CURVE('',#2031,#2029,#1293,.T.);
#2607=EDGE_CURVE('',#2030,#2032,#1294,.T.);
#2608=EDGE_CURVE('',#2032,#2032,#1620,.F.);
#2609=EDGE_CURVE('',#2033,#2033,#1621,.T.);
#2610=EDGE_CURVE('',#2033,#2034,#1295,.T.);
#2611=EDGE_CURVE('',#2034,#2034,#1622,.T.);
#2612=EDGE_CURVE('',#2035,#2035,#1623,.T.);
#2613=EDGE_CURVE('',#2036,#2036,#1624,.T.);
#2614=EDGE_CURVE('',#2037,#2037,#1625,.T.);
#2615=EDGE_CURVE('',#2037,#2036,#1296,.T.);
#2616=EDGE_CURVE('',#2038,#2038,#1626,.T.);
#2617=EDGE_CURVE('',#2039,#2039,#1627,.T.);
#2618=EDGE_CURVE('',#2038,#2040,#1297,.T.);
#2619=EDGE_CURVE('',#2040,#2040,#1628,.T.);
#2620=EDGE_CURVE('',#2035,#2039,#1298,.T.);
#2621=EDGE_CURVE('',#2041,#2041,#1629,.T.);
#2622=EDGE_CURVE('',#2041,#2042,#1299,.T.);
#2623=EDGE_CURVE('',#2042,#2042,#1630,.T.);
#2624=EDGE_CURVE('',#2043,#2043,#1631,.T.);
#2625=EDGE_CURVE('',#2043,#2044,#1300,.T.);
#2626=EDGE_CURVE('',#2044,#2044,#1632,.T.);
#2627=EDGE_CURVE('',#2045,#2046,#1301,.T.);
#2628=EDGE_CURVE('',#2047,#2045,#1302,.T.);
#2629=EDGE_CURVE('',#2048,#2047,#1303,.T.);
#2630=EDGE_CURVE('',#2046,#2048,#1304,.T.);
#2631=EDGE_CURVE('',#2049,#2050,#1305,.T.);
#2632=EDGE_CURVE('',#2051,#2049,#1306,.T.);
#2633=EDGE_CURVE('',#2052,#2051,#1307,.T.);
#2634=EDGE_CURVE('',#2050,#2052,#1308,.T.);
#2635=EDGE_CURVE('',#2047,#2052,#1633,.T.);
#2636=EDGE_CURVE('',#2050,#2045,#1634,.T.);
#2637=EDGE_CURVE('',#2049,#2046,#1635,.T.);
#2638=EDGE_CURVE('',#2048,#2051,#1636,.T.);
#2639=ORIENTED_EDGE('',*,*,#2053,.T.);
#2640=ORIENTED_EDGE('',*,*,#2054,.T.);
#2641=ORIENTED_EDGE('',*,*,#2055,.T.);
#2642=ORIENTED_EDGE('',*,*,#2056,.T.);
#2643=ORIENTED_EDGE('',*,*,#2056,.F.);
#2644=ORIENTED_EDGE('',*,*,#2057,.T.);
#2645=ORIENTED_EDGE('',*,*,#2058,.F.);
#2646=ORIENTED_EDGE('',*,*,#2059,.F.);
#2647=ORIENTED_EDGE('',*,*,#2055,.F.);
#2648=ORIENTED_EDGE('',*,*,#2060,.F.);
#2649=ORIENTED_EDGE('',*,*,#2061,.F.);
#2650=ORIENTED_EDGE('',*,*,#2062,.F.);
#2651=ORIENTED_EDGE('',*,*,#2063,.F.);
#2652=ORIENTED_EDGE('',*,*,#2064,.F.);
#2653=ORIENTED_EDGE('',*,*,#2065,.F.);
#2654=ORIENTED_EDGE('',*,*,#2057,.F.);
#2655=ORIENTED_EDGE('',*,*,#2066,.T.);
#2656=ORIENTED_EDGE('',*,*,#2067,.T.);
#2657=ORIENTED_EDGE('',*,*,#2068,.T.);
#2658=ORIENTED_EDGE('',*,*,#2069,.T.);
#2659=ORIENTED_EDGE('',*,*,#2070,.T.);
#2660=ORIENTED_EDGE('',*,*,#2058,.T.);
#2661=ORIENTED_EDGE('',*,*,#2065,.T.);
#2662=ORIENTED_EDGE('',*,*,#2071,.T.);
#2663=ORIENTED_EDGE('',*,*,#2071,.F.);
#2664=ORIENTED_EDGE('',*,*,#2064,.T.);
#2665=ORIENTED_EDGE('',*,*,#2072,.F.);
#2666=ORIENTED_EDGE('',*,*,#2073,.F.);
#2667=ORIENTED_EDGE('',*,*,#2074,.T.);
#2668=ORIENTED_EDGE('',*,*,#2072,.T.);
#2669=ORIENTED_EDGE('',*,*,#2063,.T.);
#2670=ORIENTED_EDGE('',*,*,#2075,.T.);
#2671=ORIENTED_EDGE('',*,*,#2075,.F.);
#2672=ORIENTED_EDGE('',*,*,#2062,.T.);
#2673=ORIENTED_EDGE('',*,*,#2076,.F.);
#2674=ORIENTED_EDGE('',*,*,#2077,.F.);
#2675=ORIENTED_EDGE('',*,*,#2078,.T.);
#2676=ORIENTED_EDGE('',*,*,#2076,.T.);
#2677=ORIENTED_EDGE('',*,*,#2061,.T.);
#2678=ORIENTED_EDGE('',*,*,#2079,.T.);
#2679=ORIENTED_EDGE('',*,*,#2080,.F.);
#2680=ORIENTED_EDGE('',*,*,#2081,.T.);
#2681=ORIENTED_EDGE('',*,*,#2066,.F.);
#2682=ORIENTED_EDGE('',*,*,#2081,.F.);
#2683=ORIENTED_EDGE('',*,*,#2082,.F.);
#2684=ORIENTED_EDGE('',*,*,#2083,.T.);
#2685=ORIENTED_EDGE('',*,*,#2067,.F.);
#2686=ORIENTED_EDGE('',*,*,#2083,.F.);
#2687=ORIENTED_EDGE('',*,*,#2084,.F.);
#2688=ORIENTED_EDGE('',*,*,#2085,.T.);
#2689=ORIENTED_EDGE('',*,*,#2068,.F.);
#2690=ORIENTED_EDGE('',*,*,#2085,.F.);
#2691=ORIENTED_EDGE('',*,*,#2086,.F.);
#2692=ORIENTED_EDGE('',*,*,#2087,.T.);
#2693=ORIENTED_EDGE('',*,*,#2069,.F.);
#2694=ORIENTED_EDGE('',*,*,#2087,.F.);
#2695=ORIENTED_EDGE('',*,*,#2054,.F.);
#2696=ORIENTED_EDGE('',*,*,#2088,.F.);
#2697=ORIENTED_EDGE('',*,*,#2079,.F.);
#2698=ORIENTED_EDGE('',*,*,#2060,.T.);
#2699=ORIENTED_EDGE('',*,*,#2053,.F.);
#2700=ORIENTED_EDGE('',*,*,#2059,.T.);
#2701=ORIENTED_EDGE('',*,*,#2070,.F.);
#2702=ORIENTED_EDGE('',*,*,#2073,.T.);
#2703=ORIENTED_EDGE('',*,*,#2074,.F.);
#2704=ORIENTED_EDGE('',*,*,#2077,.T.);
#2705=ORIENTED_EDGE('',*,*,#2078,.F.);
#2706=ORIENTED_EDGE('',*,*,#2088,.T.);
#2707=ORIENTED_EDGE('',*,*,#2080,.T.);
#2708=ORIENTED_EDGE('',*,*,#2082,.T.);
#2709=ORIENTED_EDGE('',*,*,#2084,.T.);
#2710=ORIENTED_EDGE('',*,*,#2086,.T.);
#2711=ORIENTED_EDGE('',*,*,#2089,.F.);
#2712=ORIENTED_EDGE('',*,*,#2090,.T.);
#2713=ORIENTED_EDGE('',*,*,#2091,.F.);
#2714=ORIENTED_EDGE('',*,*,#2090,.F.);
#2715=ORIENTED_EDGE('',*,*,#2092,.F.);
#2716=ORIENTED_EDGE('',*,*,#2093,.T.);
#2717=ORIENTED_EDGE('',*,*,#2094,.F.);
#2718=ORIENTED_EDGE('',*,*,#2093,.F.);
#2719=ORIENTED_EDGE('',*,*,#2095,.T.);
#2720=ORIENTED_EDGE('',*,*,#2096,.T.);
#2721=ORIENTED_EDGE('',*,*,#2097,.F.);
#2722=ORIENTED_EDGE('',*,*,#2098,.F.);
#2723=ORIENTED_EDGE('',*,*,#2099,.T.);
#2724=ORIENTED_EDGE('',*,*,#2098,.T.);
#2725=ORIENTED_EDGE('',*,*,#2100,.F.);
#2726=ORIENTED_EDGE('',*,*,#2101,.F.);
#2727=ORIENTED_EDGE('',*,*,#2102,.T.);
#2728=ORIENTED_EDGE('',*,*,#2101,.T.);
#2729=ORIENTED_EDGE('',*,*,#2103,.F.);
#2730=ORIENTED_EDGE('',*,*,#2104,.F.);
#2731=ORIENTED_EDGE('',*,*,#2105,.T.);
#2732=ORIENTED_EDGE('',*,*,#2104,.T.);
#2733=ORIENTED_EDGE('',*,*,#2106,.F.);
#2734=ORIENTED_EDGE('',*,*,#2096,.F.);
#2735=ORIENTED_EDGE('',*,*,#2106,.T.);
#2736=ORIENTED_EDGE('',*,*,#2103,.T.);
#2737=ORIENTED_EDGE('',*,*,#2100,.T.);
#2738=ORIENTED_EDGE('',*,*,#2097,.T.);
#2739=ORIENTED_EDGE('',*,*,#2089,.T.);
#2740=ORIENTED_EDGE('',*,*,#2092,.T.);
#2741=ORIENTED_EDGE('',*,*,#2105,.F.);
#2742=ORIENTED_EDGE('',*,*,#2095,.F.);
#2743=ORIENTED_EDGE('',*,*,#2099,.F.);
#2744=ORIENTED_EDGE('',*,*,#2102,.F.);
#2745=ORIENTED_EDGE('',*,*,#2091,.T.);
#2746=ORIENTED_EDGE('',*,*,#2094,.T.);
#2747=ORIENTED_EDGE('',*,*,#2107,.F.);
#2748=ORIENTED_EDGE('',*,*,#2108,.T.);
#2749=ORIENTED_EDGE('',*,*,#2109,.F.);
#2750=ORIENTED_EDGE('',*,*,#2108,.F.);
#2751=ORIENTED_EDGE('',*,*,#2110,.F.);
#2752=ORIENTED_EDGE('',*,*,#2111,.T.);
#2753=ORIENTED_EDGE('',*,*,#2112,.F.);
#2754=ORIENTED_EDGE('',*,*,#2111,.F.);
#2755=ORIENTED_EDGE('',*,*,#2113,.F.);
#2756=ORIENTED_EDGE('',*,*,#2114,.T.);
#2757=ORIENTED_EDGE('',*,*,#2115,.F.);
#2758=ORIENTED_EDGE('',*,*,#2116,.F.);
#2759=ORIENTED_EDGE('',*,*,#2117,.F.);
#2760=ORIENTED_EDGE('',*,*,#2116,.T.);
#2761=ORIENTED_EDGE('',*,*,#2118,.F.);
#2762=ORIENTED_EDGE('',*,*,#2119,.F.);
#2763=ORIENTED_EDGE('',*,*,#2109,.T.);
#2764=ORIENTED_EDGE('',*,*,#2112,.T.);
#2765=ORIENTED_EDGE('',*,*,#2120,.F.);
#2766=ORIENTED_EDGE('',*,*,#2119,.T.);
#2767=ORIENTED_EDGE('',*,*,#2121,.F.);
#2768=ORIENTED_EDGE('',*,*,#2122,.F.);
#2769=ORIENTED_EDGE('',*,*,#2123,.F.);
#2770=ORIENTED_EDGE('',*,*,#2122,.T.);
#2771=ORIENTED_EDGE('',*,*,#2124,.F.);
#2772=ORIENTED_EDGE('',*,*,#2114,.F.);
#2773=ORIENTED_EDGE('',*,*,#2107,.T.);
#2774=ORIENTED_EDGE('',*,*,#2110,.T.);
#2775=ORIENTED_EDGE('',*,*,#2124,.T.);
#2776=ORIENTED_EDGE('',*,*,#2121,.T.);
#2777=ORIENTED_EDGE('',*,*,#2118,.T.);
#2778=ORIENTED_EDGE('',*,*,#2115,.T.);
#2779=ORIENTED_EDGE('',*,*,#2123,.T.);
#2780=ORIENTED_EDGE('',*,*,#2113,.T.);
#2781=ORIENTED_EDGE('',*,*,#2117,.T.);
#2782=ORIENTED_EDGE('',*,*,#2120,.T.);
#2783=ORIENTED_EDGE('',*,*,#2125,.T.);
#2784=ORIENTED_EDGE('',*,*,#2126,.T.);
#2785=ORIENTED_EDGE('',*,*,#2127,.T.);
#2786=ORIENTED_EDGE('',*,*,#2128,.T.);
#2787=ORIENTED_EDGE('',*,*,#2129,.T.);
#2788=ORIENTED_EDGE('',*,*,#2126,.F.);
#2789=ORIENTED_EDGE('',*,*,#2130,.T.);
#2790=ORIENTED_EDGE('',*,*,#2131,.T.);
#2791=ORIENTED_EDGE('',*,*,#2132,.T.);
#2792=ORIENTED_EDGE('',*,*,#2128,.F.);
#2793=ORIENTED_EDGE('',*,*,#2133,.T.);
#2794=ORIENTED_EDGE('',*,*,#2134,.T.);
#2795=ORIENTED_EDGE('',*,*,#2135,.T.);
#2796=ORIENTED_EDGE('',*,*,#2131,.F.);
#2797=ORIENTED_EDGE('',*,*,#2136,.T.);
#2798=ORIENTED_EDGE('',*,*,#2134,.F.);
#2799=ORIENTED_EDGE('',*,*,#2133,.F.);
#2800=ORIENTED_EDGE('',*,*,#2137,.T.);
#2801=ORIENTED_EDGE('',*,*,#2138,.T.);
#2802=ORIENTED_EDGE('',*,*,#2139,.F.);
#2803=ORIENTED_EDGE('',*,*,#2127,.F.);
#2804=ORIENTED_EDGE('',*,*,#2140,.F.);
#2805=ORIENTED_EDGE('',*,*,#2141,.F.);
#2806=ORIENTED_EDGE('',*,*,#2137,.F.);
#2807=ORIENTED_EDGE('',*,*,#2125,.F.);
#2808=ORIENTED_EDGE('',*,*,#2132,.F.);
#2809=ORIENTED_EDGE('',*,*,#2136,.F.);
#2810=ORIENTED_EDGE('',*,*,#2130,.F.);
#2811=ORIENTED_EDGE('',*,*,#2129,.F.);
#2812=ORIENTED_EDGE('',*,*,#2142,.F.);
#2813=ORIENTED_EDGE('',*,*,#2143,.F.);
#2814=ORIENTED_EDGE('',*,*,#2140,.T.);
#2815=ORIENTED_EDGE('',*,*,#2141,.T.);
#2816=ORIENTED_EDGE('',*,*,#2143,.T.);
#2817=ORIENTED_EDGE('',*,*,#2144,.F.);
#2818=ORIENTED_EDGE('',*,*,#2138,.F.);
#2819=ORIENTED_EDGE('',*,*,#2135,.F.);
#2820=ORIENTED_EDGE('',*,*,#2139,.T.);
#2821=ORIENTED_EDGE('',*,*,#2144,.T.);
#2822=ORIENTED_EDGE('',*,*,#2142,.T.);
#2823=ORIENTED_EDGE('',*,*,#2145,.T.);
#2824=ORIENTED_EDGE('',*,*,#2146,.T.);
#2825=ORIENTED_EDGE('',*,*,#2147,.F.);
#2826=ORIENTED_EDGE('',*,*,#2148,.F.);
#2827=ORIENTED_EDGE('',*,*,#2149,.T.);
#2828=ORIENTED_EDGE('',*,*,#2148,.T.);
#2829=ORIENTED_EDGE('',*,*,#2150,.F.);
#2830=ORIENTED_EDGE('',*,*,#2151,.F.);
#2831=ORIENTED_EDGE('',*,*,#2152,.T.);
#2832=ORIENTED_EDGE('',*,*,#2151,.T.);
#2833=ORIENTED_EDGE('',*,*,#2153,.F.);
#2834=ORIENTED_EDGE('',*,*,#2154,.F.);
#2835=ORIENTED_EDGE('',*,*,#2155,.T.);
#2836=ORIENTED_EDGE('',*,*,#2154,.T.);
#2837=ORIENTED_EDGE('',*,*,#2156,.F.);
#2838=ORIENTED_EDGE('',*,*,#2146,.F.);
#2839=ORIENTED_EDGE('',*,*,#2156,.T.);
#2840=ORIENTED_EDGE('',*,*,#2153,.T.);
#2841=ORIENTED_EDGE('',*,*,#2150,.T.);
#2842=ORIENTED_EDGE('',*,*,#2147,.T.);
#2843=ORIENTED_EDGE('',*,*,#2155,.F.);
#2844=ORIENTED_EDGE('',*,*,#2145,.F.);
#2845=ORIENTED_EDGE('',*,*,#2149,.F.);
#2846=ORIENTED_EDGE('',*,*,#2152,.F.);
#2847=ORIENTED_EDGE('',*,*,#2157,.F.);
#2848=ORIENTED_EDGE('',*,*,#2158,.T.);
#2849=ORIENTED_EDGE('',*,*,#2159,.F.);
#2850=ORIENTED_EDGE('',*,*,#2158,.F.);
#2851=ORIENTED_EDGE('',*,*,#2160,.F.);
#2852=ORIENTED_EDGE('',*,*,#2161,.T.);
#2853=ORIENTED_EDGE('',*,*,#2162,.F.);
#2854=ORIENTED_EDGE('',*,*,#2163,.F.);
#2855=ORIENTED_EDGE('',*,*,#2164,.F.);
#2856=ORIENTED_EDGE('',*,*,#2163,.T.);
#2857=ORIENTED_EDGE('',*,*,#2165,.F.);
#2858=ORIENTED_EDGE('',*,*,#2166,.F.);
#2859=ORIENTED_EDGE('',*,*,#2167,.F.);
#2860=ORIENTED_EDGE('',*,*,#2166,.T.);
#2861=ORIENTED_EDGE('',*,*,#2168,.F.);
#2862=ORIENTED_EDGE('',*,*,#2169,.F.);
#2863=ORIENTED_EDGE('',*,*,#2170,.F.);
#2864=ORIENTED_EDGE('',*,*,#2169,.T.);
#2865=ORIENTED_EDGE('',*,*,#2171,.F.);
#2866=ORIENTED_EDGE('',*,*,#2172,.F.);
#2867=ORIENTED_EDGE('',*,*,#2173,.T.);
#2868=ORIENTED_EDGE('',*,*,#2172,.T.);
#2869=ORIENTED_EDGE('',*,*,#2174,.F.);
#2870=ORIENTED_EDGE('',*,*,#2161,.F.);
#2871=ORIENTED_EDGE('',*,*,#2174,.T.);
#2872=ORIENTED_EDGE('',*,*,#2171,.T.);
#2873=ORIENTED_EDGE('',*,*,#2168,.T.);
#2874=ORIENTED_EDGE('',*,*,#2165,.T.);
#2875=ORIENTED_EDGE('',*,*,#2162,.T.);
#2876=ORIENTED_EDGE('',*,*,#2157,.T.);
#2877=ORIENTED_EDGE('',*,*,#2173,.F.);
#2878=ORIENTED_EDGE('',*,*,#2160,.T.);
#2879=ORIENTED_EDGE('',*,*,#2164,.T.);
#2880=ORIENTED_EDGE('',*,*,#2167,.T.);
#2881=ORIENTED_EDGE('',*,*,#2170,.T.);
#2882=ORIENTED_EDGE('',*,*,#2159,.T.);
#2883=ORIENTED_EDGE('',*,*,#2175,.T.);
#2884=ORIENTED_EDGE('',*,*,#2176,.T.);
#2885=ORIENTED_EDGE('',*,*,#2177,.T.);
#2886=ORIENTED_EDGE('',*,*,#2178,.F.);
#2887=ORIENTED_EDGE('',*,*,#2179,.F.);
#2888=ORIENTED_EDGE('',*,*,#2180,.F.);
#2889=ORIENTED_EDGE('',*,*,#2181,.T.);
#2890=ORIENTED_EDGE('',*,*,#2182,.T.);
#2891=ORIENTED_EDGE('',*,*,#2183,.T.);
#2892=ORIENTED_EDGE('',*,*,#2175,.F.);
#2893=ORIENTED_EDGE('',*,*,#2184,.F.);
#2894=ORIENTED_EDGE('',*,*,#2185,.F.);
#2895=ORIENTED_EDGE('',*,*,#2186,.T.);
#2896=ORIENTED_EDGE('',*,*,#2187,.T.);
#2897=ORIENTED_EDGE('',*,*,#2188,.T.);
#2898=ORIENTED_EDGE('',*,*,#2181,.F.);
#2899=ORIENTED_EDGE('',*,*,#2189,.F.);
#2900=ORIENTED_EDGE('',*,*,#2190,.F.);
#2901=ORIENTED_EDGE('',*,*,#2191,.T.);
#2902=ORIENTED_EDGE('',*,*,#2192,.T.);
#2903=ORIENTED_EDGE('',*,*,#2193,.T.);
#2904=ORIENTED_EDGE('',*,*,#2186,.F.);
#2905=ORIENTED_EDGE('',*,*,#2194,.F.);
#2906=ORIENTED_EDGE('',*,*,#2195,.F.);
#2907=ORIENTED_EDGE('',*,*,#2196,.T.);
#2908=ORIENTED_EDGE('',*,*,#2197,.T.);
#2909=ORIENTED_EDGE('',*,*,#2198,.T.);
#2910=ORIENTED_EDGE('',*,*,#2191,.F.);
#2911=ORIENTED_EDGE('',*,*,#2199,.F.);
#2912=ORIENTED_EDGE('',*,*,#2200,.F.);
#2913=ORIENTED_EDGE('',*,*,#2201,.T.);
#2914=ORIENTED_EDGE('',*,*,#2202,.T.);
#2915=ORIENTED_EDGE('',*,*,#2203,.T.);
#2916=ORIENTED_EDGE('',*,*,#2196,.F.);
#2917=ORIENTED_EDGE('',*,*,#2204,.F.);
#2918=ORIENTED_EDGE('',*,*,#2205,.F.);
#2919=ORIENTED_EDGE('',*,*,#2206,.T.);
#2920=ORIENTED_EDGE('',*,*,#2207,.T.);
#2921=ORIENTED_EDGE('',*,*,#2208,.T.);
#2922=ORIENTED_EDGE('',*,*,#2201,.F.);
#2923=ORIENTED_EDGE('',*,*,#2209,.F.);
#2924=ORIENTED_EDGE('',*,*,#2210,.F.);
#2925=ORIENTED_EDGE('',*,*,#2211,.T.);
#2926=ORIENTED_EDGE('',*,*,#2212,.T.);
#2927=ORIENTED_EDGE('',*,*,#2213,.T.);
#2928=ORIENTED_EDGE('',*,*,#2206,.F.);
#2929=ORIENTED_EDGE('',*,*,#2214,.F.);
#2930=ORIENTED_EDGE('',*,*,#2215,.F.);
#2931=ORIENTED_EDGE('',*,*,#2216,.T.);
#2932=ORIENTED_EDGE('',*,*,#2217,.T.);
#2933=ORIENTED_EDGE('',*,*,#2218,.T.);
#2934=ORIENTED_EDGE('',*,*,#2211,.F.);
#2935=ORIENTED_EDGE('',*,*,#2219,.F.);
#2936=ORIENTED_EDGE('',*,*,#2220,.F.);
#2937=ORIENTED_EDGE('',*,*,#2221,.T.);
#2938=ORIENTED_EDGE('',*,*,#2222,.T.);
#2939=ORIENTED_EDGE('',*,*,#2223,.T.);
#2940=ORIENTED_EDGE('',*,*,#2216,.F.);
#2941=ORIENTED_EDGE('',*,*,#2224,.F.);
#2942=ORIENTED_EDGE('',*,*,#2225,.F.);
#2943=ORIENTED_EDGE('',*,*,#2226,.F.);
#2944=ORIENTED_EDGE('',*,*,#2227,.F.);
#2945=ORIENTED_EDGE('',*,*,#2228,.F.);
#2946=ORIENTED_EDGE('',*,*,#2229,.F.);
#2947=ORIENTED_EDGE('',*,*,#2230,.T.);
#2948=ORIENTED_EDGE('',*,*,#2231,.T.);
#2949=ORIENTED_EDGE('',*,*,#2232,.T.);
#2950=ORIENTED_EDGE('',*,*,#2233,.T.);
#2951=ORIENTED_EDGE('',*,*,#2234,.F.);
#2952=ORIENTED_EDGE('',*,*,#2235,.T.);
#2953=ORIENTED_EDGE('',*,*,#2236,.T.);
#2954=ORIENTED_EDGE('',*,*,#2237,.T.);
#2955=ORIENTED_EDGE('',*,*,#2238,.T.);
#2956=ORIENTED_EDGE('',*,*,#2232,.F.);
#2957=ORIENTED_EDGE('',*,*,#2239,.T.);
#2958=ORIENTED_EDGE('',*,*,#2240,.T.);
#2959=ORIENTED_EDGE('',*,*,#2241,.T.);
#2960=ORIENTED_EDGE('',*,*,#2242,.T.);
#2961=ORIENTED_EDGE('',*,*,#2243,.T.);
#2962=ORIENTED_EDGE('',*,*,#2236,.F.);
#2963=ORIENTED_EDGE('',*,*,#2244,.T.);
#2964=ORIENTED_EDGE('',*,*,#2245,.T.);
#2965=ORIENTED_EDGE('',*,*,#2246,.T.);
#2966=ORIENTED_EDGE('',*,*,#2247,.T.);
#2967=ORIENTED_EDGE('',*,*,#2248,.T.);
#2968=ORIENTED_EDGE('',*,*,#2241,.F.);
#2969=ORIENTED_EDGE('',*,*,#2249,.T.);
#2970=ORIENTED_EDGE('',*,*,#2250,.T.);
#2971=ORIENTED_EDGE('',*,*,#2251,.T.);
#2972=ORIENTED_EDGE('',*,*,#2252,.T.);
#2973=ORIENTED_EDGE('',*,*,#2253,.T.);
#2974=ORIENTED_EDGE('',*,*,#2246,.F.);
#2975=ORIENTED_EDGE('',*,*,#2254,.T.);
#2976=ORIENTED_EDGE('',*,*,#2255,.T.);
#2977=ORIENTED_EDGE('',*,*,#2256,.T.);
#2978=ORIENTED_EDGE('',*,*,#2257,.T.);
#2979=ORIENTED_EDGE('',*,*,#2251,.F.);
#2980=ORIENTED_EDGE('',*,*,#2258,.T.);
#2981=ORIENTED_EDGE('',*,*,#2259,.T.);
#2982=ORIENTED_EDGE('',*,*,#2260,.T.);
#2983=ORIENTED_EDGE('',*,*,#2261,.T.);
#2984=ORIENTED_EDGE('',*,*,#2255,.F.);
#2985=ORIENTED_EDGE('',*,*,#2262,.T.);
#2986=ORIENTED_EDGE('',*,*,#2263,.T.);
#2987=ORIENTED_EDGE('',*,*,#2264,.T.);
#2988=ORIENTED_EDGE('',*,*,#2265,.T.);
#2989=ORIENTED_EDGE('',*,*,#2266,.T.);
#2990=ORIENTED_EDGE('',*,*,#2260,.F.);
#2991=ORIENTED_EDGE('',*,*,#2267,.T.);
#2992=ORIENTED_EDGE('',*,*,#2268,.T.);
#2993=ORIENTED_EDGE('',*,*,#2269,.T.);
#2994=ORIENTED_EDGE('',*,*,#2270,.T.);
#2995=ORIENTED_EDGE('',*,*,#2264,.F.);
#2996=ORIENTED_EDGE('',*,*,#2271,.T.);
#2997=ORIENTED_EDGE('',*,*,#2272,.T.);
#2998=ORIENTED_EDGE('',*,*,#2273,.T.);
#2999=ORIENTED_EDGE('',*,*,#2274,.T.);
#3000=ORIENTED_EDGE('',*,*,#2269,.F.);
#3001=ORIENTED_EDGE('',*,*,#2275,.T.);
#3002=ORIENTED_EDGE('',*,*,#2276,.T.);
#3003=ORIENTED_EDGE('',*,*,#2277,.F.);
#3004=ORIENTED_EDGE('',*,*,#2278,.T.);
#3005=ORIENTED_EDGE('',*,*,#2279,.T.);
#3006=ORIENTED_EDGE('',*,*,#2280,.T.);
#3007=ORIENTED_EDGE('',*,*,#2277,.T.);
#3008=ORIENTED_EDGE('',*,*,#2281,.T.);
#3009=ORIENTED_EDGE('',*,*,#2272,.F.);
#3010=ORIENTED_EDGE('',*,*,#2282,.T.);
#3011=ORIENTED_EDGE('',*,*,#2283,.T.);
#3012=ORIENTED_EDGE('',*,*,#2226,.T.);
#3013=ORIENTED_EDGE('',*,*,#2284,.T.);
#3014=ORIENTED_EDGE('',*,*,#2285,.T.);
#3015=ORIENTED_EDGE('',*,*,#2221,.F.);
#3016=ORIENTED_EDGE('',*,*,#2286,.F.);
#3017=ORIENTED_EDGE('',*,*,#2287,.F.);
#3018=ORIENTED_EDGE('',*,*,#2288,.F.);
#3019=ORIENTED_EDGE('',*,*,#2177,.F.);
#3020=ORIENTED_EDGE('',*,*,#2176,.F.);
#3021=ORIENTED_EDGE('',*,*,#2183,.F.);
#3022=ORIENTED_EDGE('',*,*,#2182,.F.);
#3023=ORIENTED_EDGE('',*,*,#2188,.F.);
#3024=ORIENTED_EDGE('',*,*,#2187,.F.);
#3025=ORIENTED_EDGE('',*,*,#2193,.F.);
#3026=ORIENTED_EDGE('',*,*,#2192,.F.);
#3027=ORIENTED_EDGE('',*,*,#2198,.F.);
#3028=ORIENTED_EDGE('',*,*,#2197,.F.);
#3029=ORIENTED_EDGE('',*,*,#2203,.F.);
#3030=ORIENTED_EDGE('',*,*,#2202,.F.);
#3031=ORIENTED_EDGE('',*,*,#2208,.F.);
#3032=ORIENTED_EDGE('',*,*,#2207,.F.);
#3033=ORIENTED_EDGE('',*,*,#2213,.F.);
#3034=ORIENTED_EDGE('',*,*,#2212,.F.);
#3035=ORIENTED_EDGE('',*,*,#2218,.F.);
#3036=ORIENTED_EDGE('',*,*,#2217,.F.);
#3037=ORIENTED_EDGE('',*,*,#2223,.F.);
#3038=ORIENTED_EDGE('',*,*,#2222,.F.);
#3039=ORIENTED_EDGE('',*,*,#2285,.F.);
#3040=ORIENTED_EDGE('',*,*,#2284,.F.);
#3041=ORIENTED_EDGE('',*,*,#2231,.F.);
#3042=ORIENTED_EDGE('',*,*,#2230,.F.);
#3043=ORIENTED_EDGE('',*,*,#2289,.F.);
#3044=ORIENTED_EDGE('',*,*,#2278,.F.);
#3045=ORIENTED_EDGE('',*,*,#2283,.F.);
#3046=ORIENTED_EDGE('',*,*,#2282,.F.);
#3047=ORIENTED_EDGE('',*,*,#2276,.F.);
#3048=ORIENTED_EDGE('',*,*,#2275,.F.);
#3049=ORIENTED_EDGE('',*,*,#2271,.F.);
#3050=ORIENTED_EDGE('',*,*,#2268,.F.);
#3051=ORIENTED_EDGE('',*,*,#2267,.F.);
#3052=ORIENTED_EDGE('',*,*,#2263,.F.);
#3053=ORIENTED_EDGE('',*,*,#2262,.F.);
#3054=ORIENTED_EDGE('',*,*,#2259,.F.);
#3055=ORIENTED_EDGE('',*,*,#2258,.F.);
#3056=ORIENTED_EDGE('',*,*,#2254,.F.);
#3057=ORIENTED_EDGE('',*,*,#2250,.F.);
#3058=ORIENTED_EDGE('',*,*,#2249,.F.);
#3059=ORIENTED_EDGE('',*,*,#2245,.F.);
#3060=ORIENTED_EDGE('',*,*,#2244,.F.);
#3061=ORIENTED_EDGE('',*,*,#2240,.F.);
#3062=ORIENTED_EDGE('',*,*,#2239,.F.);
#3063=ORIENTED_EDGE('',*,*,#2235,.F.);
#3064=ORIENTED_EDGE('',*,*,#2290,.F.);
#3065=ORIENTED_EDGE('',*,*,#2291,.F.);
#3066=ORIENTED_EDGE('',*,*,#2233,.F.);
#3067=ORIENTED_EDGE('',*,*,#2238,.F.);
#3068=ORIENTED_EDGE('',*,*,#2237,.F.);
#3069=ORIENTED_EDGE('',*,*,#2243,.F.);
#3070=ORIENTED_EDGE('',*,*,#2242,.F.);
#3071=ORIENTED_EDGE('',*,*,#2248,.F.);
#3072=ORIENTED_EDGE('',*,*,#2247,.F.);
#3073=ORIENTED_EDGE('',*,*,#2253,.F.);
#3074=ORIENTED_EDGE('',*,*,#2252,.F.);
#3075=ORIENTED_EDGE('',*,*,#2257,.F.);
#3076=ORIENTED_EDGE('',*,*,#2256,.F.);
#3077=ORIENTED_EDGE('',*,*,#2261,.F.);
#3078=ORIENTED_EDGE('',*,*,#2266,.F.);
#3079=ORIENTED_EDGE('',*,*,#2265,.F.);
#3080=ORIENTED_EDGE('',*,*,#2270,.F.);
#3081=ORIENTED_EDGE('',*,*,#2274,.F.);
#3082=ORIENTED_EDGE('',*,*,#2273,.F.);
#3083=ORIENTED_EDGE('',*,*,#2281,.F.);
#3084=ORIENTED_EDGE('',*,*,#2280,.F.);
#3085=ORIENTED_EDGE('',*,*,#2292,.T.);
#3086=ORIENTED_EDGE('',*,*,#2293,.F.);
#3087=ORIENTED_EDGE('',*,*,#2228,.T.);
#3088=ORIENTED_EDGE('',*,*,#2227,.T.);
#3089=ORIENTED_EDGE('',*,*,#2287,.T.);
#3090=ORIENTED_EDGE('',*,*,#2286,.T.);
#3091=ORIENTED_EDGE('',*,*,#2225,.T.);
#3092=ORIENTED_EDGE('',*,*,#2224,.T.);
#3093=ORIENTED_EDGE('',*,*,#2220,.T.);
#3094=ORIENTED_EDGE('',*,*,#2219,.T.);
#3095=ORIENTED_EDGE('',*,*,#2215,.T.);
#3096=ORIENTED_EDGE('',*,*,#2214,.T.);
#3097=ORIENTED_EDGE('',*,*,#2210,.T.);
#3098=ORIENTED_EDGE('',*,*,#2209,.T.);
#3099=ORIENTED_EDGE('',*,*,#2205,.T.);
#3100=ORIENTED_EDGE('',*,*,#2204,.T.);
#3101=ORIENTED_EDGE('',*,*,#2200,.T.);
#3102=ORIENTED_EDGE('',*,*,#2199,.T.);
#3103=ORIENTED_EDGE('',*,*,#2195,.T.);
#3104=ORIENTED_EDGE('',*,*,#2194,.T.);
#3105=ORIENTED_EDGE('',*,*,#2190,.T.);
#3106=ORIENTED_EDGE('',*,*,#2189,.T.);
#3107=ORIENTED_EDGE('',*,*,#2185,.T.);
#3108=ORIENTED_EDGE('',*,*,#2184,.T.);
#3109=ORIENTED_EDGE('',*,*,#2180,.T.);
#3110=ORIENTED_EDGE('',*,*,#2179,.T.);
#3111=ORIENTED_EDGE('',*,*,#2294,.T.);
#3112=ORIENTED_EDGE('',*,*,#2291,.T.);
#3113=ORIENTED_EDGE('',*,*,#2178,.T.);
#3114=ORIENTED_EDGE('',*,*,#2288,.T.);
#3115=ORIENTED_EDGE('',*,*,#2290,.T.);
#3116=ORIENTED_EDGE('',*,*,#2234,.T.);
#3117=ORIENTED_EDGE('',*,*,#2294,.F.);
#3118=ORIENTED_EDGE('',*,*,#2295,.T.);
#3119=ORIENTED_EDGE('',*,*,#2296,.T.);
#3120=ORIENTED_EDGE('',*,*,#2295,.F.);
#3121=ORIENTED_EDGE('',*,*,#2296,.F.);
#3122=ORIENTED_EDGE('',*,*,#2293,.T.);
#3123=ORIENTED_EDGE('',*,*,#2292,.F.);
#3124=ORIENTED_EDGE('',*,*,#2279,.F.);
#3125=ORIENTED_EDGE('',*,*,#2289,.T.);
#3126=ORIENTED_EDGE('',*,*,#2229,.T.);
#3127=ORIENTED_EDGE('',*,*,#2297,.T.);
#3128=ORIENTED_EDGE('',*,*,#2298,.T.);
#3129=ORIENTED_EDGE('',*,*,#2299,.F.);
#3130=ORIENTED_EDGE('',*,*,#2298,.F.);
#3131=ORIENTED_EDGE('',*,*,#2300,.F.);
#3132=ORIENTED_EDGE('',*,*,#2301,.T.);
#3133=ORIENTED_EDGE('',*,*,#2302,.T.);
#3134=ORIENTED_EDGE('',*,*,#2301,.F.);
#3135=ORIENTED_EDGE('',*,*,#2300,.T.);
#3136=ORIENTED_EDGE('',*,*,#2299,.T.);
#3137=ORIENTED_EDGE('',*,*,#2302,.F.);
#3138=ORIENTED_EDGE('',*,*,#2297,.F.);
#3139=ORIENTED_EDGE('',*,*,#2303,.F.);
#3140=ORIENTED_EDGE('',*,*,#2304,.T.);
#3141=ORIENTED_EDGE('',*,*,#2305,.T.);
#3142=ORIENTED_EDGE('',*,*,#2306,.T.);
#3143=ORIENTED_EDGE('',*,*,#2307,.F.);
#3144=ORIENTED_EDGE('',*,*,#2308,.T.);
#3145=ORIENTED_EDGE('',*,*,#2303,.T.);
#3146=ORIENTED_EDGE('',*,*,#2309,.T.);
#3147=ORIENTED_EDGE('',*,*,#2310,.F.);
#3148=ORIENTED_EDGE('',*,*,#2311,.T.);
#3149=ORIENTED_EDGE('',*,*,#2307,.T.);
#3150=ORIENTED_EDGE('',*,*,#2312,.T.);
#3151=ORIENTED_EDGE('',*,*,#2313,.F.);
#3152=ORIENTED_EDGE('',*,*,#2314,.T.);
#3153=ORIENTED_EDGE('',*,*,#2310,.T.);
#3154=ORIENTED_EDGE('',*,*,#2315,.T.);
#3155=ORIENTED_EDGE('',*,*,#2316,.F.);
#3156=ORIENTED_EDGE('',*,*,#2317,.T.);
#3157=ORIENTED_EDGE('',*,*,#2313,.T.);
#3158=ORIENTED_EDGE('',*,*,#2318,.T.);
#3159=ORIENTED_EDGE('',*,*,#2319,.F.);
#3160=ORIENTED_EDGE('',*,*,#2320,.T.);
#3161=ORIENTED_EDGE('',*,*,#2316,.T.);
#3162=ORIENTED_EDGE('',*,*,#2321,.T.);
#3163=ORIENTED_EDGE('',*,*,#2322,.F.);
#3164=ORIENTED_EDGE('',*,*,#2323,.T.);
#3165=ORIENTED_EDGE('',*,*,#2319,.T.);
#3166=ORIENTED_EDGE('',*,*,#2324,.T.);
#3167=ORIENTED_EDGE('',*,*,#2325,.F.);
#3168=ORIENTED_EDGE('',*,*,#2326,.T.);
#3169=ORIENTED_EDGE('',*,*,#2322,.T.);
#3170=ORIENTED_EDGE('',*,*,#2327,.T.);
#3171=ORIENTED_EDGE('',*,*,#2328,.F.);
#3172=ORIENTED_EDGE('',*,*,#2329,.T.);
#3173=ORIENTED_EDGE('',*,*,#2325,.T.);
#3174=ORIENTED_EDGE('',*,*,#2330,.T.);
#3175=ORIENTED_EDGE('',*,*,#2331,.F.);
#3176=ORIENTED_EDGE('',*,*,#2332,.T.);
#3177=ORIENTED_EDGE('',*,*,#2328,.T.);
#3178=ORIENTED_EDGE('',*,*,#2333,.T.);
#3179=ORIENTED_EDGE('',*,*,#2334,.F.);
#3180=ORIENTED_EDGE('',*,*,#2335,.T.);
#3181=ORIENTED_EDGE('',*,*,#2331,.T.);
#3182=ORIENTED_EDGE('',*,*,#2336,.T.);
#3183=ORIENTED_EDGE('',*,*,#2337,.F.);
#3184=ORIENTED_EDGE('',*,*,#2338,.T.);
#3185=ORIENTED_EDGE('',*,*,#2334,.T.);
#3186=ORIENTED_EDGE('',*,*,#2339,.T.);
#3187=ORIENTED_EDGE('',*,*,#2340,.F.);
#3188=ORIENTED_EDGE('',*,*,#2341,.T.);
#3189=ORIENTED_EDGE('',*,*,#2337,.T.);
#3190=ORIENTED_EDGE('',*,*,#2342,.T.);
#3191=ORIENTED_EDGE('',*,*,#2343,.F.);
#3192=ORIENTED_EDGE('',*,*,#2344,.T.);
#3193=ORIENTED_EDGE('',*,*,#2340,.T.);
#3194=ORIENTED_EDGE('',*,*,#2345,.T.);
#3195=ORIENTED_EDGE('',*,*,#2346,.F.);
#3196=ORIENTED_EDGE('',*,*,#2347,.T.);
#3197=ORIENTED_EDGE('',*,*,#2343,.T.);
#3198=ORIENTED_EDGE('',*,*,#2348,.T.);
#3199=ORIENTED_EDGE('',*,*,#2349,.F.);
#3200=ORIENTED_EDGE('',*,*,#2350,.T.);
#3201=ORIENTED_EDGE('',*,*,#2346,.T.);
#3202=ORIENTED_EDGE('',*,*,#2351,.T.);
#3203=ORIENTED_EDGE('',*,*,#2352,.F.);
#3204=ORIENTED_EDGE('',*,*,#2353,.T.);
#3205=ORIENTED_EDGE('',*,*,#2349,.T.);
#3206=ORIENTED_EDGE('',*,*,#2354,.T.);
#3207=ORIENTED_EDGE('',*,*,#2355,.F.);
#3208=ORIENTED_EDGE('',*,*,#2356,.T.);
#3209=ORIENTED_EDGE('',*,*,#2352,.T.);
#3210=ORIENTED_EDGE('',*,*,#2357,.T.);
#3211=ORIENTED_EDGE('',*,*,#2358,.F.);
#3212=ORIENTED_EDGE('',*,*,#2359,.T.);
#3213=ORIENTED_EDGE('',*,*,#2355,.T.);
#3214=ORIENTED_EDGE('',*,*,#2360,.T.);
#3215=ORIENTED_EDGE('',*,*,#2361,.F.);
#3216=ORIENTED_EDGE('',*,*,#2362,.T.);
#3217=ORIENTED_EDGE('',*,*,#2358,.T.);
#3218=ORIENTED_EDGE('',*,*,#2363,.T.);
#3219=ORIENTED_EDGE('',*,*,#2364,.F.);
#3220=ORIENTED_EDGE('',*,*,#2365,.T.);
#3221=ORIENTED_EDGE('',*,*,#2361,.T.);
#3222=ORIENTED_EDGE('',*,*,#2366,.T.);
#3223=ORIENTED_EDGE('',*,*,#2367,.F.);
#3224=ORIENTED_EDGE('',*,*,#2368,.T.);
#3225=ORIENTED_EDGE('',*,*,#2364,.T.);
#3226=ORIENTED_EDGE('',*,*,#2369,.T.);
#3227=ORIENTED_EDGE('',*,*,#2370,.F.);
#3228=ORIENTED_EDGE('',*,*,#2371,.T.);
#3229=ORIENTED_EDGE('',*,*,#2367,.T.);
#3230=ORIENTED_EDGE('',*,*,#2372,.T.);
#3231=ORIENTED_EDGE('',*,*,#2373,.F.);
#3232=ORIENTED_EDGE('',*,*,#2374,.T.);
#3233=ORIENTED_EDGE('',*,*,#2370,.T.);
#3234=ORIENTED_EDGE('',*,*,#2375,.T.);
#3235=ORIENTED_EDGE('',*,*,#2376,.F.);
#3236=ORIENTED_EDGE('',*,*,#2377,.T.);
#3237=ORIENTED_EDGE('',*,*,#2373,.T.);
#3238=ORIENTED_EDGE('',*,*,#2378,.T.);
#3239=ORIENTED_EDGE('',*,*,#2379,.F.);
#3240=ORIENTED_EDGE('',*,*,#2380,.T.);
#3241=ORIENTED_EDGE('',*,*,#2376,.T.);
#3242=ORIENTED_EDGE('',*,*,#2381,.T.);
#3243=ORIENTED_EDGE('',*,*,#2382,.F.);
#3244=ORIENTED_EDGE('',*,*,#2383,.T.);
#3245=ORIENTED_EDGE('',*,*,#2379,.T.);
#3246=ORIENTED_EDGE('',*,*,#2384,.T.);
#3247=ORIENTED_EDGE('',*,*,#2385,.F.);
#3248=ORIENTED_EDGE('',*,*,#2386,.T.);
#3249=ORIENTED_EDGE('',*,*,#2382,.T.);
#3250=ORIENTED_EDGE('',*,*,#2387,.T.);
#3251=ORIENTED_EDGE('',*,*,#2388,.F.);
#3252=ORIENTED_EDGE('',*,*,#2389,.F.);
#3253=ORIENTED_EDGE('',*,*,#2390,.F.);
#3254=ORIENTED_EDGE('',*,*,#2391,.T.);
#3255=ORIENTED_EDGE('',*,*,#2392,.F.);
#3256=ORIENTED_EDGE('',*,*,#2393,.F.);
#3257=ORIENTED_EDGE('',*,*,#2388,.T.);
#3258=ORIENTED_EDGE('',*,*,#2394,.T.);
#3259=ORIENTED_EDGE('',*,*,#2395,.T.);
#3260=ORIENTED_EDGE('',*,*,#2396,.F.);
#3261=ORIENTED_EDGE('',*,*,#2397,.F.);
#3262=ORIENTED_EDGE('',*,*,#2398,.F.);
#3263=ORIENTED_EDGE('',*,*,#2392,.T.);
#3264=ORIENTED_EDGE('',*,*,#2399,.T.);
#3265=ORIENTED_EDGE('',*,*,#2400,.T.);
#3266=ORIENTED_EDGE('',*,*,#2401,.F.);
#3267=ORIENTED_EDGE('',*,*,#2402,.F.);
#3268=ORIENTED_EDGE('',*,*,#2396,.T.);
#3269=ORIENTED_EDGE('',*,*,#2403,.T.);
#3270=ORIENTED_EDGE('',*,*,#2404,.T.);
#3271=ORIENTED_EDGE('',*,*,#2405,.F.);
#3272=ORIENTED_EDGE('',*,*,#2406,.F.);
#3273=ORIENTED_EDGE('',*,*,#2407,.F.);
#3274=ORIENTED_EDGE('',*,*,#2401,.T.);
#3275=ORIENTED_EDGE('',*,*,#2408,.T.);
#3276=ORIENTED_EDGE('',*,*,#2409,.F.);
#3277=ORIENTED_EDGE('',*,*,#2410,.F.);
#3278=ORIENTED_EDGE('',*,*,#2411,.F.);
#3279=ORIENTED_EDGE('',*,*,#2405,.T.);
#3280=ORIENTED_EDGE('',*,*,#2412,.T.);
#3281=ORIENTED_EDGE('',*,*,#2413,.T.);
#3282=ORIENTED_EDGE('',*,*,#2414,.F.);
#3283=ORIENTED_EDGE('',*,*,#2415,.F.);
#3284=ORIENTED_EDGE('',*,*,#2409,.T.);
#3285=ORIENTED_EDGE('',*,*,#2416,.T.);
#3286=ORIENTED_EDGE('',*,*,#2417,.T.);
#3287=ORIENTED_EDGE('',*,*,#2418,.F.);
#3288=ORIENTED_EDGE('',*,*,#2419,.F.);
#3289=ORIENTED_EDGE('',*,*,#2420,.F.);
#3290=ORIENTED_EDGE('',*,*,#2414,.T.);
#3291=ORIENTED_EDGE('',*,*,#2421,.T.);
#3292=ORIENTED_EDGE('',*,*,#2422,.F.);
#3293=ORIENTED_EDGE('',*,*,#2423,.F.);
#3294=ORIENTED_EDGE('',*,*,#2418,.T.);
#3295=ORIENTED_EDGE('',*,*,#2424,.T.);
#3296=ORIENTED_EDGE('',*,*,#2425,.T.);
#3297=ORIENTED_EDGE('',*,*,#2426,.F.);
#3298=ORIENTED_EDGE('',*,*,#2427,.F.);
#3299=ORIENTED_EDGE('',*,*,#2428,.F.);
#3300=ORIENTED_EDGE('',*,*,#2422,.T.);
#3301=ORIENTED_EDGE('',*,*,#2429,.T.);
#3302=ORIENTED_EDGE('',*,*,#2430,.F.);
#3303=ORIENTED_EDGE('',*,*,#2431,.F.);
#3304=ORIENTED_EDGE('',*,*,#2426,.T.);
#3305=ORIENTED_EDGE('',*,*,#2432,.T.);
#3306=ORIENTED_EDGE('',*,*,#2433,.T.);
#3307=ORIENTED_EDGE('',*,*,#2434,.F.);
#3308=ORIENTED_EDGE('',*,*,#2435,.F.);
#3309=ORIENTED_EDGE('',*,*,#2436,.F.);
#3310=ORIENTED_EDGE('',*,*,#2430,.T.);
#3311=ORIENTED_EDGE('',*,*,#2437,.T.);
#3312=ORIENTED_EDGE('',*,*,#2438,.F.);
#3313=ORIENTED_EDGE('',*,*,#2439,.F.);
#3314=ORIENTED_EDGE('',*,*,#2440,.F.);
#3315=ORIENTED_EDGE('',*,*,#2434,.T.);
#3316=ORIENTED_EDGE('',*,*,#2441,.T.);
#3317=ORIENTED_EDGE('',*,*,#2442,.T.);
#3318=ORIENTED_EDGE('',*,*,#2443,.F.);
#3319=ORIENTED_EDGE('',*,*,#2444,.F.);
#3320=ORIENTED_EDGE('',*,*,#2445,.F.);
#3321=ORIENTED_EDGE('',*,*,#2438,.T.);
#3322=ORIENTED_EDGE('',*,*,#2446,.T.);
#3323=ORIENTED_EDGE('',*,*,#2447,.T.);
#3324=ORIENTED_EDGE('',*,*,#2448,.F.);
#3325=ORIENTED_EDGE('',*,*,#2449,.F.);
#3326=ORIENTED_EDGE('',*,*,#2443,.T.);
#3327=ORIENTED_EDGE('',*,*,#2450,.T.);
#3328=ORIENTED_EDGE('',*,*,#2451,.T.);
#3329=ORIENTED_EDGE('',*,*,#2452,.F.);
#3330=ORIENTED_EDGE('',*,*,#2453,.F.);
#3331=ORIENTED_EDGE('',*,*,#2454,.F.);
#3332=ORIENTED_EDGE('',*,*,#2448,.T.);
#3333=ORIENTED_EDGE('',*,*,#2455,.T.);
#3334=ORIENTED_EDGE('',*,*,#2456,.T.);
#3335=ORIENTED_EDGE('',*,*,#2457,.F.);
#3336=ORIENTED_EDGE('',*,*,#2458,.F.);
#3337=ORIENTED_EDGE('',*,*,#2452,.T.);
#3338=ORIENTED_EDGE('',*,*,#2459,.T.);
#3339=ORIENTED_EDGE('',*,*,#2460,.F.);
#3340=ORIENTED_EDGE('',*,*,#2461,.F.);
#3341=ORIENTED_EDGE('',*,*,#2462,.F.);
#3342=ORIENTED_EDGE('',*,*,#2457,.T.);
#3343=ORIENTED_EDGE('',*,*,#2463,.T.);
#3344=ORIENTED_EDGE('',*,*,#2464,.T.);
#3345=ORIENTED_EDGE('',*,*,#2465,.F.);
#3346=ORIENTED_EDGE('',*,*,#2466,.F.);
#3347=ORIENTED_EDGE('',*,*,#2460,.T.);
#3348=ORIENTED_EDGE('',*,*,#2467,.T.);
#3349=ORIENTED_EDGE('',*,*,#2468,.T.);
#3350=ORIENTED_EDGE('',*,*,#2469,.F.);
#3351=ORIENTED_EDGE('',*,*,#2470,.F.);
#3352=ORIENTED_EDGE('',*,*,#2471,.F.);
#3353=ORIENTED_EDGE('',*,*,#2465,.T.);
#3354=ORIENTED_EDGE('',*,*,#2472,.T.);
#3355=ORIENTED_EDGE('',*,*,#2473,.T.);
#3356=ORIENTED_EDGE('',*,*,#2474,.F.);
#3357=ORIENTED_EDGE('',*,*,#2475,.F.);
#3358=ORIENTED_EDGE('',*,*,#2476,.F.);
#3359=ORIENTED_EDGE('',*,*,#2469,.T.);
#3360=ORIENTED_EDGE('',*,*,#2477,.T.);
#3361=ORIENTED_EDGE('',*,*,#2478,.T.);
#3362=ORIENTED_EDGE('',*,*,#2479,.F.);
#3363=ORIENTED_EDGE('',*,*,#2480,.F.);
#3364=ORIENTED_EDGE('',*,*,#2481,.F.);
#3365=ORIENTED_EDGE('',*,*,#2474,.T.);
#3366=ORIENTED_EDGE('',*,*,#2482,.T.);
#3367=ORIENTED_EDGE('',*,*,#2483,.F.);
#3368=ORIENTED_EDGE('',*,*,#2484,.F.);
#3369=ORIENTED_EDGE('',*,*,#2485,.F.);
#3370=ORIENTED_EDGE('',*,*,#2479,.T.);
#3371=ORIENTED_EDGE('',*,*,#2486,.T.);
#3372=ORIENTED_EDGE('',*,*,#2487,.T.);
#3373=ORIENTED_EDGE('',*,*,#2488,.F.);
#3374=ORIENTED_EDGE('',*,*,#2489,.F.);
#3375=ORIENTED_EDGE('',*,*,#2483,.T.);
#3376=ORIENTED_EDGE('',*,*,#2490,.T.);
#3377=ORIENTED_EDGE('',*,*,#2491,.T.);
#3378=ORIENTED_EDGE('',*,*,#2492,.F.);
#3379=ORIENTED_EDGE('',*,*,#2493,.F.);
#3380=ORIENTED_EDGE('',*,*,#2494,.F.);
#3381=ORIENTED_EDGE('',*,*,#2488,.T.);
#3382=ORIENTED_EDGE('',*,*,#2495,.T.);
#3383=ORIENTED_EDGE('',*,*,#2496,.F.);
#3384=ORIENTED_EDGE('',*,*,#2497,.F.);
#3385=ORIENTED_EDGE('',*,*,#2498,.F.);
#3386=ORIENTED_EDGE('',*,*,#2492,.T.);
#3387=ORIENTED_EDGE('',*,*,#2499,.T.);
#3388=ORIENTED_EDGE('',*,*,#2500,.T.);
#3389=ORIENTED_EDGE('',*,*,#2501,.F.);
#3390=ORIENTED_EDGE('',*,*,#2502,.F.);
#3391=ORIENTED_EDGE('',*,*,#2503,.F.);
#3392=ORIENTED_EDGE('',*,*,#2496,.T.);
#3393=ORIENTED_EDGE('',*,*,#2504,.T.);
#3394=ORIENTED_EDGE('',*,*,#2505,.F.);
#3395=ORIENTED_EDGE('',*,*,#2506,.F.);
#3396=ORIENTED_EDGE('',*,*,#2501,.T.);
#3397=ORIENTED_EDGE('',*,*,#2507,.T.);
#3398=ORIENTED_EDGE('',*,*,#2508,.T.);
#3399=ORIENTED_EDGE('',*,*,#2505,.T.);
#3400=ORIENTED_EDGE('',*,*,#2509,.T.);
#3401=ORIENTED_EDGE('',*,*,#2510,.T.);
#3402=ORIENTED_EDGE('',*,*,#2511,.F.);
#3403=ORIENTED_EDGE('',*,*,#2512,.F.);
#3404=ORIENTED_EDGE('',*,*,#2513,.F.);
#3405=ORIENTED_EDGE('',*,*,#2385,.T.);
#3406=ORIENTED_EDGE('',*,*,#2514,.T.);
#3407=ORIENTED_EDGE('',*,*,#2515,.T.);
#3408=ORIENTED_EDGE('',*,*,#2516,.T.);
#3409=ORIENTED_EDGE('',*,*,#2517,.F.);
#3410=ORIENTED_EDGE('',*,*,#2518,.F.);
#3411=ORIENTED_EDGE('',*,*,#2519,.F.);
#3412=ORIENTED_EDGE('',*,*,#2515,.F.);
#3413=ORIENTED_EDGE('',*,*,#2519,.T.);
#3414=ORIENTED_EDGE('',*,*,#2520,.F.);
#3415=ORIENTED_EDGE('',*,*,#2510,.F.);
#3416=ORIENTED_EDGE('',*,*,#2509,.F.);
#3417=ORIENTED_EDGE('',*,*,#2508,.F.);
#3418=ORIENTED_EDGE('',*,*,#2507,.F.);
#3419=ORIENTED_EDGE('',*,*,#2504,.F.);
#3420=ORIENTED_EDGE('',*,*,#2500,.F.);
#3421=ORIENTED_EDGE('',*,*,#2499,.F.);
#3422=ORIENTED_EDGE('',*,*,#2495,.F.);
#3423=ORIENTED_EDGE('',*,*,#2491,.F.);
#3424=ORIENTED_EDGE('',*,*,#2490,.F.);
#3425=ORIENTED_EDGE('',*,*,#2487,.F.);
#3426=ORIENTED_EDGE('',*,*,#2486,.F.);
#3427=ORIENTED_EDGE('',*,*,#2482,.F.);
#3428=ORIENTED_EDGE('',*,*,#2478,.F.);
#3429=ORIENTED_EDGE('',*,*,#2477,.F.);
#3430=ORIENTED_EDGE('',*,*,#2473,.F.);
#3431=ORIENTED_EDGE('',*,*,#2472,.F.);
#3432=ORIENTED_EDGE('',*,*,#2468,.F.);
#3433=ORIENTED_EDGE('',*,*,#2467,.F.);
#3434=ORIENTED_EDGE('',*,*,#2464,.F.);
#3435=ORIENTED_EDGE('',*,*,#2463,.F.);
#3436=ORIENTED_EDGE('',*,*,#2459,.F.);
#3437=ORIENTED_EDGE('',*,*,#2456,.F.);
#3438=ORIENTED_EDGE('',*,*,#2455,.F.);
#3439=ORIENTED_EDGE('',*,*,#2451,.F.);
#3440=ORIENTED_EDGE('',*,*,#2450,.F.);
#3441=ORIENTED_EDGE('',*,*,#2447,.F.);
#3442=ORIENTED_EDGE('',*,*,#2446,.F.);
#3443=ORIENTED_EDGE('',*,*,#2442,.F.);
#3444=ORIENTED_EDGE('',*,*,#2441,.F.);
#3445=ORIENTED_EDGE('',*,*,#2437,.F.);
#3446=ORIENTED_EDGE('',*,*,#2433,.F.);
#3447=ORIENTED_EDGE('',*,*,#2432,.F.);
#3448=ORIENTED_EDGE('',*,*,#2429,.F.);
#3449=ORIENTED_EDGE('',*,*,#2425,.F.);
#3450=ORIENTED_EDGE('',*,*,#2424,.F.);
#3451=ORIENTED_EDGE('',*,*,#2421,.F.);
#3452=ORIENTED_EDGE('',*,*,#2417,.F.);
#3453=ORIENTED_EDGE('',*,*,#2416,.F.);
#3454=ORIENTED_EDGE('',*,*,#2413,.F.);
#3455=ORIENTED_EDGE('',*,*,#2412,.F.);
#3456=ORIENTED_EDGE('',*,*,#2408,.F.);
#3457=ORIENTED_EDGE('',*,*,#2404,.F.);
#3458=ORIENTED_EDGE('',*,*,#2403,.F.);
#3459=ORIENTED_EDGE('',*,*,#2400,.F.);
#3460=ORIENTED_EDGE('',*,*,#2399,.F.);
#3461=ORIENTED_EDGE('',*,*,#2395,.F.);
#3462=ORIENTED_EDGE('',*,*,#2394,.F.);
#3463=ORIENTED_EDGE('',*,*,#2391,.F.);
#3464=ORIENTED_EDGE('',*,*,#2521,.F.);
#3465=ORIENTED_EDGE('',*,*,#2304,.F.);
#3466=ORIENTED_EDGE('',*,*,#2308,.F.);
#3467=ORIENTED_EDGE('',*,*,#2311,.F.);
#3468=ORIENTED_EDGE('',*,*,#2314,.F.);
#3469=ORIENTED_EDGE('',*,*,#2317,.F.);
#3470=ORIENTED_EDGE('',*,*,#2320,.F.);
#3471=ORIENTED_EDGE('',*,*,#2323,.F.);
#3472=ORIENTED_EDGE('',*,*,#2326,.F.);
#3473=ORIENTED_EDGE('',*,*,#2329,.F.);
#3474=ORIENTED_EDGE('',*,*,#2332,.F.);
#3475=ORIENTED_EDGE('',*,*,#2335,.F.);
#3476=ORIENTED_EDGE('',*,*,#2338,.F.);
#3477=ORIENTED_EDGE('',*,*,#2341,.F.);
#3478=ORIENTED_EDGE('',*,*,#2344,.F.);
#3479=ORIENTED_EDGE('',*,*,#2347,.F.);
#3480=ORIENTED_EDGE('',*,*,#2350,.F.);
#3481=ORIENTED_EDGE('',*,*,#2353,.F.);
#3482=ORIENTED_EDGE('',*,*,#2356,.F.);
#3483=ORIENTED_EDGE('',*,*,#2359,.F.);
#3484=ORIENTED_EDGE('',*,*,#2362,.F.);
#3485=ORIENTED_EDGE('',*,*,#2365,.F.);
#3486=ORIENTED_EDGE('',*,*,#2368,.F.);
#3487=ORIENTED_EDGE('',*,*,#2371,.F.);
#3488=ORIENTED_EDGE('',*,*,#2374,.F.);
#3489=ORIENTED_EDGE('',*,*,#2377,.F.);
#3490=ORIENTED_EDGE('',*,*,#2380,.F.);
#3491=ORIENTED_EDGE('',*,*,#2383,.F.);
#3492=ORIENTED_EDGE('',*,*,#2386,.F.);
#3493=ORIENTED_EDGE('',*,*,#2516,.F.);
#3494=ORIENTED_EDGE('',*,*,#2517,.T.);
#3495=ORIENTED_EDGE('',*,*,#2514,.F.);
#3496=ORIENTED_EDGE('',*,*,#2387,.F.);
#3497=ORIENTED_EDGE('',*,*,#2384,.F.);
#3498=ORIENTED_EDGE('',*,*,#2381,.F.);
#3499=ORIENTED_EDGE('',*,*,#2378,.F.);
#3500=ORIENTED_EDGE('',*,*,#2375,.F.);
#3501=ORIENTED_EDGE('',*,*,#2372,.F.);
#3502=ORIENTED_EDGE('',*,*,#2369,.F.);
#3503=ORIENTED_EDGE('',*,*,#2366,.F.);
#3504=ORIENTED_EDGE('',*,*,#2363,.F.);
#3505=ORIENTED_EDGE('',*,*,#2360,.F.);
#3506=ORIENTED_EDGE('',*,*,#2357,.F.);
#3507=ORIENTED_EDGE('',*,*,#2354,.F.);
#3508=ORIENTED_EDGE('',*,*,#2351,.F.);
#3509=ORIENTED_EDGE('',*,*,#2348,.F.);
#3510=ORIENTED_EDGE('',*,*,#2345,.F.);
#3511=ORIENTED_EDGE('',*,*,#2342,.F.);
#3512=ORIENTED_EDGE('',*,*,#2339,.F.);
#3513=ORIENTED_EDGE('',*,*,#2336,.F.);
#3514=ORIENTED_EDGE('',*,*,#2333,.F.);
#3515=ORIENTED_EDGE('',*,*,#2330,.F.);
#3516=ORIENTED_EDGE('',*,*,#2327,.F.);
#3517=ORIENTED_EDGE('',*,*,#2324,.F.);
#3518=ORIENTED_EDGE('',*,*,#2321,.F.);
#3519=ORIENTED_EDGE('',*,*,#2318,.F.);
#3520=ORIENTED_EDGE('',*,*,#2315,.F.);
#3521=ORIENTED_EDGE('',*,*,#2312,.F.);
#3522=ORIENTED_EDGE('',*,*,#2309,.F.);
#3523=ORIENTED_EDGE('',*,*,#2306,.F.);
#3524=ORIENTED_EDGE('',*,*,#2522,.F.);
#3525=ORIENTED_EDGE('',*,*,#2523,.T.);
#3526=ORIENTED_EDGE('',*,*,#2389,.T.);
#3527=ORIENTED_EDGE('',*,*,#2393,.T.);
#3528=ORIENTED_EDGE('',*,*,#2398,.T.);
#3529=ORIENTED_EDGE('',*,*,#2397,.T.);
#3530=ORIENTED_EDGE('',*,*,#2402,.T.);
#3531=ORIENTED_EDGE('',*,*,#2407,.T.);
#3532=ORIENTED_EDGE('',*,*,#2406,.T.);
#3533=ORIENTED_EDGE('',*,*,#2411,.T.);
#3534=ORIENTED_EDGE('',*,*,#2410,.T.);
#3535=ORIENTED_EDGE('',*,*,#2415,.T.);
#3536=ORIENTED_EDGE('',*,*,#2420,.T.);
#3537=ORIENTED_EDGE('',*,*,#2419,.T.);
#3538=ORIENTED_EDGE('',*,*,#2423,.T.);
#3539=ORIENTED_EDGE('',*,*,#2428,.T.);
#3540=ORIENTED_EDGE('',*,*,#2427,.T.);
#3541=ORIENTED_EDGE('',*,*,#2431,.T.);
#3542=ORIENTED_EDGE('',*,*,#2436,.T.);
#3543=ORIENTED_EDGE('',*,*,#2435,.T.);
#3544=ORIENTED_EDGE('',*,*,#2440,.T.);
#3545=ORIENTED_EDGE('',*,*,#2439,.T.);
#3546=ORIENTED_EDGE('',*,*,#2445,.T.);
#3547=ORIENTED_EDGE('',*,*,#2444,.T.);
#3548=ORIENTED_EDGE('',*,*,#2449,.T.);
#3549=ORIENTED_EDGE('',*,*,#2454,.T.);
#3550=ORIENTED_EDGE('',*,*,#2453,.T.);
#3551=ORIENTED_EDGE('',*,*,#2458,.T.);
#3552=ORIENTED_EDGE('',*,*,#2462,.T.);
#3553=ORIENTED_EDGE('',*,*,#2461,.T.);
#3554=ORIENTED_EDGE('',*,*,#2466,.T.);
#3555=ORIENTED_EDGE('',*,*,#2471,.T.);
#3556=ORIENTED_EDGE('',*,*,#2470,.T.);
#3557=ORIENTED_EDGE('',*,*,#2476,.T.);
#3558=ORIENTED_EDGE('',*,*,#2475,.T.);
#3559=ORIENTED_EDGE('',*,*,#2481,.T.);
#3560=ORIENTED_EDGE('',*,*,#2480,.T.);
#3561=ORIENTED_EDGE('',*,*,#2485,.T.);
#3562=ORIENTED_EDGE('',*,*,#2484,.T.);
#3563=ORIENTED_EDGE('',*,*,#2489,.T.);
#3564=ORIENTED_EDGE('',*,*,#2494,.T.);
#3565=ORIENTED_EDGE('',*,*,#2493,.T.);
#3566=ORIENTED_EDGE('',*,*,#2498,.T.);
#3567=ORIENTED_EDGE('',*,*,#2497,.T.);
#3568=ORIENTED_EDGE('',*,*,#2503,.T.);
#3569=ORIENTED_EDGE('',*,*,#2502,.T.);
#3570=ORIENTED_EDGE('',*,*,#2506,.T.);
#3571=ORIENTED_EDGE('',*,*,#2513,.T.);
#3572=ORIENTED_EDGE('',*,*,#2512,.T.);
#3573=ORIENTED_EDGE('',*,*,#2524,.F.);
#3574=ORIENTED_EDGE('',*,*,#2525,.F.);
#3575=ORIENTED_EDGE('',*,*,#2526,.T.);
#3576=ORIENTED_EDGE('',*,*,#2527,.T.);
#3577=ORIENTED_EDGE('',*,*,#2528,.F.);
#3578=ORIENTED_EDGE('',*,*,#2529,.F.);
#3579=ORIENTED_EDGE('',*,*,#2530,.T.);
#3580=ORIENTED_EDGE('',*,*,#2531,.T.);
#3581=ORIENTED_EDGE('',*,*,#2526,.F.);
#3582=ORIENTED_EDGE('',*,*,#2532,.F.);
#3583=ORIENTED_EDGE('',*,*,#2533,.T.);
#3584=ORIENTED_EDGE('',*,*,#2534,.T.);
#3585=ORIENTED_EDGE('',*,*,#2530,.F.);
#3586=ORIENTED_EDGE('',*,*,#2535,.F.);
#3587=ORIENTED_EDGE('',*,*,#2536,.T.);
#3588=ORIENTED_EDGE('',*,*,#2537,.T.);
#3589=ORIENTED_EDGE('',*,*,#2533,.F.);
#3590=ORIENTED_EDGE('',*,*,#2538,.F.);
#3591=ORIENTED_EDGE('',*,*,#2539,.T.);
#3592=ORIENTED_EDGE('',*,*,#2540,.T.);
#3593=ORIENTED_EDGE('',*,*,#2536,.F.);
#3594=ORIENTED_EDGE('',*,*,#2541,.F.);
#3595=ORIENTED_EDGE('',*,*,#2528,.T.);
#3596=ORIENTED_EDGE('',*,*,#2542,.T.);
#3597=ORIENTED_EDGE('',*,*,#2539,.F.);
#3598=ORIENTED_EDGE('',*,*,#2542,.F.);
#3599=ORIENTED_EDGE('',*,*,#2527,.F.);
#3600=ORIENTED_EDGE('',*,*,#2531,.F.);
#3601=ORIENTED_EDGE('',*,*,#2534,.F.);
#3602=ORIENTED_EDGE('',*,*,#2537,.F.);
#3603=ORIENTED_EDGE('',*,*,#2540,.F.);
#3604=ORIENTED_EDGE('',*,*,#2543,.T.);
#3605=ORIENTED_EDGE('',*,*,#2521,.T.);
#3606=ORIENTED_EDGE('',*,*,#2390,.T.);
#3607=ORIENTED_EDGE('',*,*,#2523,.F.);
#3608=ORIENTED_EDGE('',*,*,#2522,.T.);
#3609=ORIENTED_EDGE('',*,*,#2305,.F.);
#3610=ORIENTED_EDGE('',*,*,#2543,.F.);
#3611=ORIENTED_EDGE('',*,*,#2544,.T.);
#3612=ORIENTED_EDGE('',*,*,#2545,.T.);
#3613=ORIENTED_EDGE('',*,*,#2544,.F.);
#3614=ORIENTED_EDGE('',*,*,#2545,.F.);
#3615=ORIENTED_EDGE('',*,*,#2525,.T.);
#3616=ORIENTED_EDGE('',*,*,#2541,.T.);
#3617=ORIENTED_EDGE('',*,*,#2538,.T.);
#3618=ORIENTED_EDGE('',*,*,#2535,.T.);
#3619=ORIENTED_EDGE('',*,*,#2532,.T.);
#3620=ORIENTED_EDGE('',*,*,#2529,.T.);
#3621=ORIENTED_EDGE('',*,*,#2518,.T.);
#3622=ORIENTED_EDGE('',*,*,#2524,.T.);
#3623=ORIENTED_EDGE('',*,*,#2511,.T.);
#3624=ORIENTED_EDGE('',*,*,#2520,.T.);
#3625=ORIENTED_EDGE('',*,*,#2546,.T.);
#3626=ORIENTED_EDGE('',*,*,#2547,.T.);
#3627=ORIENTED_EDGE('',*,*,#2548,.T.);
#3628=ORIENTED_EDGE('',*,*,#2549,.T.);
#3629=ORIENTED_EDGE('',*,*,#2549,.F.);
#3630=ORIENTED_EDGE('',*,*,#2550,.T.);
#3631=ORIENTED_EDGE('',*,*,#2551,.T.);
#3632=ORIENTED_EDGE('',*,*,#2552,.F.);
#3633=ORIENTED_EDGE('',*,*,#2548,.F.);
#3634=ORIENTED_EDGE('',*,*,#2553,.F.);
#3635=ORIENTED_EDGE('',*,*,#2554,.F.);
#3636=ORIENTED_EDGE('',*,*,#2555,.F.);
#3637=ORIENTED_EDGE('',*,*,#2556,.F.);
#3638=ORIENTED_EDGE('',*,*,#2557,.F.);
#3639=ORIENTED_EDGE('',*,*,#2550,.F.);
#3640=ORIENTED_EDGE('',*,*,#2558,.T.);
#3641=ORIENTED_EDGE('',*,*,#2559,.T.);
#3642=ORIENTED_EDGE('',*,*,#2560,.T.);
#3643=ORIENTED_EDGE('',*,*,#2554,.T.);
#3644=ORIENTED_EDGE('',*,*,#2561,.T.);
#3645=ORIENTED_EDGE('',*,*,#2560,.F.);
#3646=ORIENTED_EDGE('',*,*,#2562,.F.);
#3647=ORIENTED_EDGE('',*,*,#2563,.F.);
#3648=ORIENTED_EDGE('',*,*,#2555,.T.);
#3649=ORIENTED_EDGE('',*,*,#2564,.F.);
#3650=ORIENTED_EDGE('',*,*,#2565,.T.);
#3651=ORIENTED_EDGE('',*,*,#2558,.F.);
#3652=ORIENTED_EDGE('',*,*,#2565,.F.);
#3653=ORIENTED_EDGE('',*,*,#2547,.F.);
#3654=ORIENTED_EDGE('',*,*,#2566,.F.);
#3655=ORIENTED_EDGE('',*,*,#2561,.F.);
#3656=ORIENTED_EDGE('',*,*,#2553,.T.);
#3657=ORIENTED_EDGE('',*,*,#2556,.T.);
#3658=ORIENTED_EDGE('',*,*,#2563,.T.);
#3659=ORIENTED_EDGE('',*,*,#2567,.F.);
#3660=ORIENTED_EDGE('',*,*,#2568,.F.);
#3661=ORIENTED_EDGE('',*,*,#2557,.T.);
#3662=ORIENTED_EDGE('',*,*,#2568,.T.);
#3663=ORIENTED_EDGE('',*,*,#2569,.F.);
#3664=ORIENTED_EDGE('',*,*,#2551,.F.);
#3665=ORIENTED_EDGE('',*,*,#2546,.F.);
#3666=ORIENTED_EDGE('',*,*,#2552,.T.);
#3667=ORIENTED_EDGE('',*,*,#2569,.T.);
#3668=ORIENTED_EDGE('',*,*,#2567,.T.);
#3669=ORIENTED_EDGE('',*,*,#2562,.T.);
#3670=ORIENTED_EDGE('',*,*,#2559,.F.);
#3671=ORIENTED_EDGE('',*,*,#2566,.T.);
#3672=ORIENTED_EDGE('',*,*,#2564,.T.);
#3673=ORIENTED_EDGE('',*,*,#2570,.T.);
#3674=ORIENTED_EDGE('',*,*,#2571,.T.);
#3675=ORIENTED_EDGE('',*,*,#2572,.F.);
#3676=ORIENTED_EDGE('',*,*,#2573,.F.);
#3677=ORIENTED_EDGE('',*,*,#2574,.T.);
#3678=ORIENTED_EDGE('',*,*,#2573,.T.);
#3679=ORIENTED_EDGE('',*,*,#2575,.F.);
#3680=ORIENTED_EDGE('',*,*,#2576,.F.);
#3681=ORIENTED_EDGE('',*,*,#2577,.T.);
#3682=ORIENTED_EDGE('',*,*,#2576,.T.);
#3683=ORIENTED_EDGE('',*,*,#2578,.F.);
#3684=ORIENTED_EDGE('',*,*,#2579,.F.);
#3685=ORIENTED_EDGE('',*,*,#2580,.T.);
#3686=ORIENTED_EDGE('',*,*,#2579,.T.);
#3687=ORIENTED_EDGE('',*,*,#2581,.F.);
#3688=ORIENTED_EDGE('',*,*,#2571,.F.);
#3689=ORIENTED_EDGE('',*,*,#2581,.T.);
#3690=ORIENTED_EDGE('',*,*,#2578,.T.);
#3691=ORIENTED_EDGE('',*,*,#2575,.T.);
#3692=ORIENTED_EDGE('',*,*,#2572,.T.);
#3693=ORIENTED_EDGE('',*,*,#2580,.F.);
#3694=ORIENTED_EDGE('',*,*,#2570,.F.);
#3695=ORIENTED_EDGE('',*,*,#2574,.F.);
#3696=ORIENTED_EDGE('',*,*,#2577,.F.);
#3697=ORIENTED_EDGE('',*,*,#2582,.T.);
#3698=ORIENTED_EDGE('',*,*,#2583,.T.);
#3699=ORIENTED_EDGE('',*,*,#2584,.F.);
#3700=ORIENTED_EDGE('',*,*,#2583,.F.);
#3701=ORIENTED_EDGE('',*,*,#2585,.F.);
#3702=ORIENTED_EDGE('',*,*,#2586,.T.);
#3703=ORIENTED_EDGE('',*,*,#2587,.T.);
#3704=ORIENTED_EDGE('',*,*,#2586,.F.);
#3705=ORIENTED_EDGE('',*,*,#2585,.T.);
#3706=ORIENTED_EDGE('',*,*,#2584,.T.);
#3707=ORIENTED_EDGE('',*,*,#2587,.F.);
#3708=ORIENTED_EDGE('',*,*,#2582,.F.);
#3709=ORIENTED_EDGE('',*,*,#2588,.T.);
#3710=ORIENTED_EDGE('',*,*,#2589,.T.);
#3711=ORIENTED_EDGE('',*,*,#2590,.F.);
#3712=ORIENTED_EDGE('',*,*,#2591,.F.);
#3713=ORIENTED_EDGE('',*,*,#2592,.T.);
#3714=ORIENTED_EDGE('',*,*,#2591,.T.);
#3715=ORIENTED_EDGE('',*,*,#2593,.F.);
#3716=ORIENTED_EDGE('',*,*,#2594,.F.);
#3717=ORIENTED_EDGE('',*,*,#2595,.T.);
#3718=ORIENTED_EDGE('',*,*,#2594,.T.);
#3719=ORIENTED_EDGE('',*,*,#2596,.F.);
#3720=ORIENTED_EDGE('',*,*,#2597,.F.);
#3721=ORIENTED_EDGE('',*,*,#2598,.T.);
#3722=ORIENTED_EDGE('',*,*,#2597,.T.);
#3723=ORIENTED_EDGE('',*,*,#2599,.F.);
#3724=ORIENTED_EDGE('',*,*,#2589,.F.);
#3725=ORIENTED_EDGE('',*,*,#2599,.T.);
#3726=ORIENTED_EDGE('',*,*,#2596,.T.);
#3727=ORIENTED_EDGE('',*,*,#2593,.T.);
#3728=ORIENTED_EDGE('',*,*,#2590,.T.);
#3729=ORIENTED_EDGE('',*,*,#2598,.F.);
#3730=ORIENTED_EDGE('',*,*,#2588,.F.);
#3731=ORIENTED_EDGE('',*,*,#2592,.F.);
#3732=ORIENTED_EDGE('',*,*,#2595,.F.);
#3733=ORIENTED_EDGE('',*,*,#2600,.F.);
#3734=ORIENTED_EDGE('',*,*,#2601,.T.);
#3735=ORIENTED_EDGE('',*,*,#2602,.T.);
#3736=ORIENTED_EDGE('',*,*,#2601,.F.);
#3737=ORIENTED_EDGE('',*,*,#2600,.T.);
#3738=ORIENTED_EDGE('',*,*,#2602,.F.);
#3739=ORIENTED_EDGE('',*,*,#2603,.T.);
#3740=ORIENTED_EDGE('',*,*,#2604,.T.);
#3741=ORIENTED_EDGE('',*,*,#2605,.T.);
#3742=ORIENTED_EDGE('',*,*,#2606,.T.);
#3743=ORIENTED_EDGE('',*,*,#2603,.F.);
#3744=ORIENTED_EDGE('',*,*,#2606,.F.);
#3745=ORIENTED_EDGE('',*,*,#2604,.F.);
#3746=ORIENTED_EDGE('',*,*,#2607,.T.);
#3747=ORIENTED_EDGE('',*,*,#2608,.T.);
#3748=ORIENTED_EDGE('',*,*,#2607,.F.);
#3749=ORIENTED_EDGE('',*,*,#2608,.F.);
#3750=ORIENTED_EDGE('',*,*,#2605,.F.);
#3751=ORIENTED_EDGE('',*,*,#2609,.F.);
#3752=ORIENTED_EDGE('',*,*,#2610,.T.);
#3753=ORIENTED_EDGE('',*,*,#2611,.T.);
#3754=ORIENTED_EDGE('',*,*,#2610,.F.);
#3755=ORIENTED_EDGE('',*,*,#2612,.F.);
#3756=ORIENTED_EDGE('',*,*,#2611,.F.);
#3757=ORIENTED_EDGE('',*,*,#2613,.F.);
#3758=ORIENTED_EDGE('',*,*,#2609,.T.);
#3759=ORIENTED_EDGE('',*,*,#2614,.F.);
#3760=ORIENTED_EDGE('',*,*,#2615,.T.);
#3761=ORIENTED_EDGE('',*,*,#2613,.T.);
#3762=ORIENTED_EDGE('',*,*,#2615,.F.);
#3763=ORIENTED_EDGE('',*,*,#2616,.T.);
#3764=ORIENTED_EDGE('',*,*,#2617,.F.);
#3765=ORIENTED_EDGE('',*,*,#2616,.F.);
#3766=ORIENTED_EDGE('',*,*,#2618,.T.);
#3767=ORIENTED_EDGE('',*,*,#2619,.T.);
#3768=ORIENTED_EDGE('',*,*,#2618,.F.);
#3769=ORIENTED_EDGE('',*,*,#2619,.F.);
#3770=ORIENTED_EDGE('',*,*,#2612,.T.);
#3771=ORIENTED_EDGE('',*,*,#2620,.T.);
#3772=ORIENTED_EDGE('',*,*,#2617,.T.);
#3773=ORIENTED_EDGE('',*,*,#2620,.F.);
#3774=ORIENTED_EDGE('',*,*,#2614,.T.);
#3775=ORIENTED_EDGE('',*,*,#2621,.T.);
#3776=ORIENTED_EDGE('',*,*,#2622,.T.);
#3777=ORIENTED_EDGE('',*,*,#2623,.F.);
#3778=ORIENTED_EDGE('',*,*,#2622,.F.);
#3779=ORIENTED_EDGE('',*,*,#2624,.F.);
#3780=ORIENTED_EDGE('',*,*,#2625,.T.);
#3781=ORIENTED_EDGE('',*,*,#2626,.T.);
#3782=ORIENTED_EDGE('',*,*,#2625,.F.);
#3783=ORIENTED_EDGE('',*,*,#2624,.T.);
#3784=ORIENTED_EDGE('',*,*,#2623,.T.);
#3785=ORIENTED_EDGE('',*,*,#2626,.F.);
#3786=ORIENTED_EDGE('',*,*,#2621,.F.);
#3787=ORIENTED_EDGE('',*,*,#2627,.F.);
#3788=ORIENTED_EDGE('',*,*,#2628,.F.);
#3789=ORIENTED_EDGE('',*,*,#2629,.F.);
#3790=ORIENTED_EDGE('',*,*,#2630,.F.);
#3791=ORIENTED_EDGE('',*,*,#2631,.F.);
#3792=ORIENTED_EDGE('',*,*,#2632,.F.);
#3793=ORIENTED_EDGE('',*,*,#2633,.F.);
#3794=ORIENTED_EDGE('',*,*,#2634,.F.);
#3795=ORIENTED_EDGE('',*,*,#2634,.T.);
#3796=ORIENTED_EDGE('',*,*,#2635,.F.);
#3797=ORIENTED_EDGE('',*,*,#2628,.T.);
#3798=ORIENTED_EDGE('',*,*,#2636,.F.);
#3799=ORIENTED_EDGE('',*,*,#2631,.T.);
#3800=ORIENTED_EDGE('',*,*,#2636,.T.);
#3801=ORIENTED_EDGE('',*,*,#2627,.T.);
#3802=ORIENTED_EDGE('',*,*,#2637,.F.);
#3803=ORIENTED_EDGE('',*,*,#2633,.T.);
#3804=ORIENTED_EDGE('',*,*,#2638,.F.);
#3805=ORIENTED_EDGE('',*,*,#2629,.T.);
#3806=ORIENTED_EDGE('',*,*,#2635,.T.);
#3807=ORIENTED_EDGE('',*,*,#2632,.T.);
#3808=ORIENTED_EDGE('',*,*,#2637,.T.);
#3809=ORIENTED_EDGE('',*,*,#2630,.T.);
#3810=ORIENTED_EDGE('',*,*,#2638,.T.);
#3811=CYLINDRICAL_SURFACE('',#4363,10.);
#3812=CYLINDRICAL_SURFACE('',#4375,10.);
#3813=CYLINDRICAL_SURFACE('',#4378,10.);
#3814=CYLINDRICAL_SURFACE('',#4381,10.);
#3815=CYLINDRICAL_SURFACE('',#4383,4.5);
#3816=CYLINDRICAL_SURFACE('',#4385,4.5);
#3817=CYLINDRICAL_SURFACE('',#4387,4.5);
#3818=CYLINDRICAL_SURFACE('',#4389,4.5);
#3819=CYLINDRICAL_SURFACE('',#4394,6.5);
#3820=CYLINDRICAL_SURFACE('',#4397,6.5);
#3821=CYLINDRICAL_SURFACE('',#4407,6.5);
#3822=CYLINDRICAL_SURFACE('',#4410,6.5);
#3823=CYLINDRICAL_SURFACE('',#4420,2.);
#3824=CYLINDRICAL_SURFACE('',#4423,2.);
#3825=CYLINDRICAL_SURFACE('',#4425,2.);
#3826=CYLINDRICAL_SURFACE('',#4427,2.);
#3827=CYLINDRICAL_SURFACE('',#4442,6.);
#3828=CYLINDRICAL_SURFACE('',#4449,12.);
#3829=CYLINDRICAL_SURFACE('',#4455,6.11325);
#3830=CYLINDRICAL_SURFACE('',#4457,6.11325);
#3831=CYLINDRICAL_SURFACE('',#4458,6.11325);
#3832=CYLINDRICAL_SURFACE('',#4459,6.11325);
#3833=CYLINDRICAL_SURFACE('',#4460,6.11325);
#3834=CYLINDRICAL_SURFACE('',#4461,6.11325);
#3835=CYLINDRICAL_SURFACE('',#4462,6.11325);
#3836=CYLINDRICAL_SURFACE('',#4463,6.11325);
#3837=CYLINDRICAL_SURFACE('',#4464,6.11325);
#3838=CYLINDRICAL_SURFACE('',#4465,6.11325);
#3839=CYLINDRICAL_SURFACE('',#4466,6.11325);
#3840=CYLINDRICAL_SURFACE('',#4468,5.13675);
#3841=CYLINDRICAL_SURFACE('',#4470,5.13675);
#3842=CYLINDRICAL_SURFACE('',#4471,5.13675);
#3843=CYLINDRICAL_SURFACE('',#4472,5.13675);
#3844=CYLINDRICAL_SURFACE('',#4473,5.13675);
#3845=CYLINDRICAL_SURFACE('',#4474,5.13675);
#3846=CYLINDRICAL_SURFACE('',#4475,5.13675);
#3847=CYLINDRICAL_SURFACE('',#4476,5.13675);
#3848=CYLINDRICAL_SURFACE('',#4477,5.13675);
#3849=CYLINDRICAL_SURFACE('',#4478,5.13675);
#3850=CYLINDRICAL_SURFACE('',#4479,5.13675);
#3851=CYLINDRICAL_SURFACE('',#4481,5.13675);
#3852=CYLINDRICAL_SURFACE('',#4482,6.11325);
#3853=CYLINDRICAL_SURFACE('',#4485,12.);
#3854=CYLINDRICAL_SURFACE('',#4489,6.5);
#3855=CYLINDRICAL_SURFACE('',#4492,12.);
#3856=CYLINDRICAL_SURFACE('',#4498,5.91675);
#3857=CYLINDRICAL_SURFACE('',#4500,5.91675);
#3858=CYLINDRICAL_SURFACE('',#4501,5.91675);
#3859=CYLINDRICAL_SURFACE('',#4502,5.91675);
#3860=CYLINDRICAL_SURFACE('',#4503,5.91675);
#3861=CYLINDRICAL_SURFACE('',#4504,5.91675);
#3862=CYLINDRICAL_SURFACE('',#4505,5.91675);
#3863=CYLINDRICAL_SURFACE('',#4506,5.91675);
#3864=CYLINDRICAL_SURFACE('',#4507,5.91675);
#3865=CYLINDRICAL_SURFACE('',#4508,5.91675);
#3866=CYLINDRICAL_SURFACE('',#4509,5.91675);
#3867=CYLINDRICAL_SURFACE('',#4510,5.91675);
#3868=CYLINDRICAL_SURFACE('',#4511,5.91675);
#3869=CYLINDRICAL_SURFACE('',#4512,5.91675);
#3870=CYLINDRICAL_SURFACE('',#4513,5.91675);
#3871=CYLINDRICAL_SURFACE('',#4514,5.91675);
#3872=CYLINDRICAL_SURFACE('',#4515,5.91675);
#3873=CYLINDRICAL_SURFACE('',#4516,5.91675);
#3874=CYLINDRICAL_SURFACE('',#4517,5.91675);
#3875=CYLINDRICAL_SURFACE('',#4518,5.91675);
#3876=CYLINDRICAL_SURFACE('',#4519,5.91675);
#3877=CYLINDRICAL_SURFACE('',#4520,5.91675);
#3878=CYLINDRICAL_SURFACE('',#4521,5.91675);
#3879=CYLINDRICAL_SURFACE('',#4522,5.91675);
#3880=CYLINDRICAL_SURFACE('',#4523,5.91675);
#3881=CYLINDRICAL_SURFACE('',#4524,5.91675);
#3882=CYLINDRICAL_SURFACE('',#4525,5.91675);
#3883=CYLINDRICAL_SURFACE('',#4526,5.91675);
#3884=CYLINDRICAL_SURFACE('',#4527,4.91825);
#3885=CYLINDRICAL_SURFACE('',#4529,4.91825);
#3886=CYLINDRICAL_SURFACE('',#4530,4.91825);
#3887=CYLINDRICAL_SURFACE('',#4531,4.91825);
#3888=CYLINDRICAL_SURFACE('',#4532,4.91825);
#3889=CYLINDRICAL_SURFACE('',#4533,4.91825);
#3890=CYLINDRICAL_SURFACE('',#4534,4.91825);
#3891=CYLINDRICAL_SURFACE('',#4535,4.91825);
#3892=CYLINDRICAL_SURFACE('',#4536,4.91825);
#3893=CYLINDRICAL_SURFACE('',#4537,4.91825);
#3894=CYLINDRICAL_SURFACE('',#4538,4.91825);
#3895=CYLINDRICAL_SURFACE('',#4539,4.91825);
#3896=CYLINDRICAL_SURFACE('',#4540,4.91825);
#3897=CYLINDRICAL_SURFACE('',#4541,4.91825);
#3898=CYLINDRICAL_SURFACE('',#4542,4.91825);
#3899=CYLINDRICAL_SURFACE('',#4543,4.91825);
#3900=CYLINDRICAL_SURFACE('',#4544,4.91825);
#3901=CYLINDRICAL_SURFACE('',#4545,4.91825);
#3902=CYLINDRICAL_SURFACE('',#4546,4.91825);
#3903=CYLINDRICAL_SURFACE('',#4547,4.91825);
#3904=CYLINDRICAL_SURFACE('',#4548,4.91825);
#3905=CYLINDRICAL_SURFACE('',#4549,4.91825);
#3906=CYLINDRICAL_SURFACE('',#4550,4.91825);
#3907=CYLINDRICAL_SURFACE('',#4551,4.91825);
#3908=CYLINDRICAL_SURFACE('',#4552,4.91825);
#3909=CYLINDRICAL_SURFACE('',#4553,4.91825);
#3910=CYLINDRICAL_SURFACE('',#4554,4.91825);
#3911=CYLINDRICAL_SURFACE('',#4555,4.91825);
#3912=CYLINDRICAL_SURFACE('',#4556,4.91825);
#3913=CYLINDRICAL_SURFACE('',#4558,5.91675);
#3914=CYLINDRICAL_SURFACE('',#4573,9.);
#3915=CYLINDRICAL_SURFACE('',#4578,5.);
#3916=CYLINDRICAL_SURFACE('',#4586,5.);
#3917=CYLINDRICAL_SURFACE('',#4589,8.);
#3918=CYLINDRICAL_SURFACE('',#4592,12.);
#3919=CYLINDRICAL_SURFACE('',#4604,6.);
#3920=CYLINDRICAL_SURFACE('',#4607,8.);
#3921=CYLINDRICAL_SURFACE('',#4620,8.);
#3922=CYLINDRICAL_SURFACE('',#4630,8.);
#3923=CYLINDRICAL_SURFACE('',#4632,16.);
#3924=CYLINDRICAL_SURFACE('',#4636,5.);
#3925=CYLINDRICAL_SURFACE('',#4643,6.);
#3926=CYLINDRICAL_SURFACE('',#4648,9.);
#3927=CYLINDRICAL_SURFACE('',#4651,6.);
#3928=CYLINDRICAL_SURFACE('',#4654,6.);
#3929=CYLINDRICAL_SURFACE('',#4657,11.);
#3930=CYLINDRICAL_SURFACE('',#4668,5.);
#3931=CYLINDRICAL_SURFACE('',#4670,9.);
#3932=ADVANCED_FACE('',(#602),#3811,.T.);
#3933=ADVANCED_FACE('',(#603),#516,.T.);
#3934=ADVANCED_FACE('',(#604,#482,#483,#484,#485),#517,.F.);
#3935=ADVANCED_FACE('',(#605),#3812,.T.);
#3936=ADVANCED_FACE('',(#606),#518,.T.);
#3937=ADVANCED_FACE('',(#607),#3813,.T.);
#3938=ADVANCED_FACE('',(#608),#519,.T.);
#3939=ADVANCED_FACE('',(#609),#3814,.T.);
#3940=ADVANCED_FACE('',(#610),#3815,.F.);
#3941=ADVANCED_FACE('',(#611),#3816,.F.);
#3942=ADVANCED_FACE('',(#612),#3817,.F.);
#3943=ADVANCED_FACE('',(#613),#3818,.F.);
#3944=ADVANCED_FACE('',(#614),#520,.T.);
#3945=ADVANCED_FACE('',(#615,#486,#487,#488,#489),#521,.T.);
#3946=ADVANCED_FACE('',(#616),#3819,.F.);
#3947=ADVANCED_FACE('',(#617),#3820,.F.);
#3948=ADVANCED_FACE('',(#618),#522,.T.);
#3949=ADVANCED_FACE('',(#619),#523,.T.);
#3950=ADVANCED_FACE('',(#620),#524,.T.);
#3951=ADVANCED_FACE('',(#621),#525,.T.);
#3952=ADVANCED_FACE('',(#622,#490,#491),#526,.T.);
#3953=ADVANCED_FACE('',(#623,#492,#493),#527,.F.);
#3954=ADVANCED_FACE('',(#624),#3821,.F.);
#3955=ADVANCED_FACE('',(#625),#3822,.F.);
#3956=ADVANCED_FACE('',(#626),#528,.T.);
#3957=ADVANCED_FACE('',(#627,#494,#495),#529,.T.);
#3958=ADVANCED_FACE('',(#628),#530,.T.);
#3959=ADVANCED_FACE('',(#629,#496,#497),#531,.T.);
#3960=ADVANCED_FACE('',(#630),#532,.T.);
#3961=ADVANCED_FACE('',(#631),#533,.F.);
#3962=ADVANCED_FACE('',(#632),#3823,.T.);
#3963=ADVANCED_FACE('',(#633),#3824,.T.);
#3964=ADVANCED_FACE('',(#634),#3825,.T.);
#3965=ADVANCED_FACE('',(#635),#3826,.T.);
#3966=ADVANCED_FACE('',(#636),#534,.T.);
#3967=ADVANCED_FACE('',(#637),#535,.F.);
#3968=ADVANCED_FACE('',(#638),#536,.T.);
#3969=ADVANCED_FACE('',(#639),#537,.T.);
#3970=ADVANCED_FACE('',(#640),#538,.T.);
#3971=ADVANCED_FACE('',(#641),#539,.T.);
#3972=ADVANCED_FACE('',(#642),#540,.T.);
#3973=ADVANCED_FACE('',(#643),#541,.T.);
#3974=ADVANCED_FACE('',(#644),#542,.T.);
#3975=ADVANCED_FACE('',(#645),#543,.T.);
#3976=ADVANCED_FACE('',(#646),#544,.T.);
#3977=ADVANCED_FACE('',(#647),#545,.F.);
#3978=ADVANCED_FACE('',(#648),#3827,.F.);
#3979=ADVANCED_FACE('',(#649),#546,.T.);
#3980=ADVANCED_FACE('',(#650),#547,.T.);
#3981=ADVANCED_FACE('',(#651),#548,.T.);
#3982=ADVANCED_FACE('',(#652),#549,.T.);
#3983=ADVANCED_FACE('',(#653),#3828,.T.);
#3984=ADVANCED_FACE('',(#654,#498),#550,.T.);
#3985=ADVANCED_FACE('',(#655,#499),#551,.F.);
#3986=ADVANCED_FACE('',(#656),#3829,.F.);
#3987=ADVANCED_FACE('',(#657),#3830,.F.);
#3988=ADVANCED_FACE('',(#658),#3831,.F.);
#3989=ADVANCED_FACE('',(#659),#3832,.F.);
#3990=ADVANCED_FACE('',(#660),#3833,.F.);
#3991=ADVANCED_FACE('',(#661),#3834,.F.);
#3992=ADVANCED_FACE('',(#662),#3835,.F.);
#3993=ADVANCED_FACE('',(#663),#3836,.F.);
#3994=ADVANCED_FACE('',(#664),#3837,.F.);
#3995=ADVANCED_FACE('',(#665),#3838,.F.);
#3996=ADVANCED_FACE('',(#666),#3839,.F.);
#3997=ADVANCED_FACE('',(#667),#3840,.F.);
#3998=ADVANCED_FACE('',(#668),#3841,.F.);
#3999=ADVANCED_FACE('',(#669),#3842,.F.);
#4000=ADVANCED_FACE('',(#670),#3843,.F.);
#4001=ADVANCED_FACE('',(#671),#3844,.F.);
#4002=ADVANCED_FACE('',(#672),#3845,.F.);
#4003=ADVANCED_FACE('',(#673),#3846,.F.);
#4004=ADVANCED_FACE('',(#674),#3847,.F.);
#4005=ADVANCED_FACE('',(#675),#3848,.F.);
#4006=ADVANCED_FACE('',(#676),#3849,.F.);
#4007=ADVANCED_FACE('',(#677),#3850,.F.);
#4008=ADVANCED_FACE('',(#678),#3851,.F.);
#4009=ADVANCED_FACE('',(#679),#3852,.F.);
#4010=ADVANCED_FACE('',(#680),#148,.F.);
#4011=ADVANCED_FACE('',(#681),#149,.F.);
#4012=ADVANCED_FACE('',(#682,#500),#552,.T.);
#4013=ADVANCED_FACE('',(#683),#3853,.T.);
#4014=ADVANCED_FACE('',(#684,#501),#553,.F.);
#4015=ADVANCED_FACE('',(#685),#3854,.F.);
#4016=ADVANCED_FACE('',(#686),#3855,.T.);
#4017=ADVANCED_FACE('',(#687,#502),#554,.T.);
#4018=ADVANCED_FACE('',(#688,#503),#555,.F.);
#4019=ADVANCED_FACE('',(#689),#3856,.T.);
#4020=ADVANCED_FACE('',(#690),#3857,.T.);
#4021=ADVANCED_FACE('',(#691),#3858,.T.);
#4022=ADVANCED_FACE('',(#692),#3859,.T.);
#4023=ADVANCED_FACE('',(#693),#3860,.T.);
#4024=ADVANCED_FACE('',(#694),#3861,.T.);
#4025=ADVANCED_FACE('',(#695),#3862,.T.);
#4026=ADVANCED_FACE('',(#696),#3863,.T.);
#4027=ADVANCED_FACE('',(#697),#3864,.T.);
#4028=ADVANCED_FACE('',(#698),#3865,.T.);
#4029=ADVANCED_FACE('',(#699),#3866,.T.);
#4030=ADVANCED_FACE('',(#700),#3867,.T.);
#4031=ADVANCED_FACE('',(#701),#3868,.T.);
#4032=ADVANCED_FACE('',(#702),#3869,.T.);
#4033=ADVANCED_FACE('',(#703),#3870,.T.);
#4034=ADVANCED_FACE('',(#704),#3871,.T.);
#4035=ADVANCED_FACE('',(#705),#3872,.T.);
#4036=ADVANCED_FACE('',(#706),#3873,.T.);
#4037=ADVANCED_FACE('',(#707),#3874,.T.);
#4038=ADVANCED_FACE('',(#708),#3875,.T.);
#4039=ADVANCED_FACE('',(#709),#3876,.T.);
#4040=ADVANCED_FACE('',(#710),#3877,.T.);
#4041=ADVANCED_FACE('',(#711),#3878,.T.);
#4042=ADVANCED_FACE('',(#712),#3879,.T.);
#4043=ADVANCED_FACE('',(#713),#3880,.T.);
#4044=ADVANCED_FACE('',(#714),#3881,.T.);
#4045=ADVANCED_FACE('',(#715),#3882,.T.);
#4046=ADVANCED_FACE('',(#716),#3883,.T.);
#4047=ADVANCED_FACE('',(#717),#3884,.T.);
#4048=ADVANCED_FACE('',(#718),#3885,.T.);
#4049=ADVANCED_FACE('',(#719),#3886,.T.);
#4050=ADVANCED_FACE('',(#720),#3887,.T.);
#4051=ADVANCED_FACE('',(#721),#3888,.T.);
#4052=ADVANCED_FACE('',(#722),#3889,.T.);
#4053=ADVANCED_FACE('',(#723),#3890,.T.);
#4054=ADVANCED_FACE('',(#724),#3891,.T.);
#4055=ADVANCED_FACE('',(#725),#3892,.T.);
#4056=ADVANCED_FACE('',(#726),#3893,.T.);
#4057=ADVANCED_FACE('',(#727),#3894,.T.);
#4058=ADVANCED_FACE('',(#728),#3895,.T.);
#4059=ADVANCED_FACE('',(#729),#3896,.T.);
#4060=ADVANCED_FACE('',(#730),#3897,.T.);
#4061=ADVANCED_FACE('',(#731),#3898,.T.);
#4062=ADVANCED_FACE('',(#732),#3899,.T.);
#4063=ADVANCED_FACE('',(#733),#3900,.T.);
#4064=ADVANCED_FACE('',(#734),#3901,.T.);
#4065=ADVANCED_FACE('',(#735),#3902,.T.);
#4066=ADVANCED_FACE('',(#736),#3903,.T.);
#4067=ADVANCED_FACE('',(#737),#3904,.T.);
#4068=ADVANCED_FACE('',(#738),#3905,.T.);
#4069=ADVANCED_FACE('',(#739),#3906,.T.);
#4070=ADVANCED_FACE('',(#740),#3907,.T.);
#4071=ADVANCED_FACE('',(#741),#3908,.T.);
#4072=ADVANCED_FACE('',(#742),#3909,.T.);
#4073=ADVANCED_FACE('',(#743),#3910,.T.);
#4074=ADVANCED_FACE('',(#744),#3911,.T.);
#4075=ADVANCED_FACE('',(#745),#3912,.T.);
#4076=ADVANCED_FACE('',(#746),#3913,.T.);
#4077=ADVANCED_FACE('',(#747),#147,.T.);
#4078=ADVANCED_FACE('',(#748),#150,.F.);
#4079=ADVANCED_FACE('',(#749),#151,.F.);
#4080=ADVANCED_FACE('',(#750),#556,.F.);
#4081=ADVANCED_FACE('',(#751),#557,.F.);
#4082=ADVANCED_FACE('',(#752),#558,.F.);
#4083=ADVANCED_FACE('',(#753),#559,.F.);
#4084=ADVANCED_FACE('',(#754),#560,.F.);
#4085=ADVANCED_FACE('',(#755),#561,.F.);
#4086=ADVANCED_FACE('',(#756),#562,.F.);
#4087=ADVANCED_FACE('',(#757,#504),#563,.T.);
#4088=ADVANCED_FACE('',(#758),#3914,.T.);
#4089=ADVANCED_FACE('',(#759,#505),#564,.F.);
#4090=ADVANCED_FACE('',(#760),#565,.T.);
#4091=ADVANCED_FACE('',(#761),#3915,.T.);
#4092=ADVANCED_FACE('',(#762),#566,.T.);
#4093=ADVANCED_FACE('',(#763,#506),#567,.F.);
#4094=ADVANCED_FACE('',(#764),#3916,.T.);
#4095=ADVANCED_FACE('',(#765),#568,.T.);
#4096=ADVANCED_FACE('',(#766),#3917,.F.);
#4097=ADVANCED_FACE('',(#767),#569,.T.);
#4098=ADVANCED_FACE('',(#768),#3918,.T.);
#4099=ADVANCED_FACE('',(#769),#570,.T.);
#4100=ADVANCED_FACE('',(#770,#507),#571,.T.);
#4101=ADVANCED_FACE('',(#771),#572,.T.);
#4102=ADVANCED_FACE('',(#772),#573,.T.);
#4103=ADVANCED_FACE('',(#773),#574,.T.);
#4104=ADVANCED_FACE('',(#774),#575,.T.);
#4105=ADVANCED_FACE('',(#775),#576,.T.);
#4106=ADVANCED_FACE('',(#776),#577,.F.);
#4107=ADVANCED_FACE('',(#777),#3919,.F.);
#4108=ADVANCED_FACE('',(#778),#3920,.T.);
#4109=ADVANCED_FACE('',(#779,#508),#578,.T.);
#4110=ADVANCED_FACE('',(#780,#509),#579,.F.);
#4111=ADVANCED_FACE('',(#781),#580,.T.);
#4112=ADVANCED_FACE('',(#782),#581,.T.);
#4113=ADVANCED_FACE('',(#783),#582,.T.);
#4114=ADVANCED_FACE('',(#784),#583,.T.);
#4115=ADVANCED_FACE('',(#785),#584,.T.);
#4116=ADVANCED_FACE('',(#786),#585,.F.);
#4117=ADVANCED_FACE('',(#787),#3921,.T.);
#4118=ADVANCED_FACE('',(#788),#586,.T.);
#4119=ADVANCED_FACE('',(#789),#587,.F.);
#4120=ADVANCED_FACE('',(#790),#588,.F.);
#4121=ADVANCED_FACE('',(#791),#589,.T.);
#4122=ADVANCED_FACE('',(#792),#3922,.F.);
#4123=ADVANCED_FACE('',(#793),#3923,.T.);
#4124=ADVANCED_FACE('',(#794,#510),#590,.F.);
#4125=ADVANCED_FACE('',(#795),#3924,.T.);
#4126=ADVANCED_FACE('',(#796,#511),#591,.F.);
#4127=ADVANCED_FACE('',(#797,#512),#592,.F.);
#4128=ADVANCED_FACE('',(#798),#3925,.T.);
#4129=ADVANCED_FACE('',(#799,#513),#593,.T.);
#4130=ADVANCED_FACE('',(#800),#3926,.T.);
#4131=ADVANCED_FACE('',(#801),#594,.F.);
#4132=ADVANCED_FACE('',(#802),#3927,.T.);
#4133=ADVANCED_FACE('',(#803),#595,.T.);
#4134=ADVANCED_FACE('',(#804),#3928,.F.);
#4135=ADVANCED_FACE('',(#805),#3929,.T.);
#4136=ADVANCED_FACE('',(#806,#514),#596,.T.);
#4137=ADVANCED_FACE('',(#807,#515),#597,.F.);
#4138=ADVANCED_FACE('',(#808),#598,.F.);
#4139=ADVANCED_FACE('',(#809),#599,.F.);
#4140=ADVANCED_FACE('',(#810),#600,.F.);
#4141=ADVANCED_FACE('',(#811),#3930,.F.);
#4142=ADVANCED_FACE('',(#812),#3931,.T.);
#4143=ADVANCED_FACE('',(#813),#601,.T.);
#4144=CLOSED_SHELL('',(#3932,#3933,#3934,#3935,#3936,#3937,#3938,#3939,
#3940,#3941,#3942,#3943,#3944,#3945));
#4145=CLOSED_SHELL('',(#3946,#3947,#3948,#3949,#3950,#3951,#3952,#3953));
#4146=CLOSED_SHELL('',(#3954,#3955,#3956,#3957,#3958,#3959,#3960,#3961));
#4147=CLOSED_SHELL('',(#3962,#3963,#3964,#3965,#3966,#3967,#3968,#3969,
#3970,#3971));
#4148=CLOSED_SHELL('',(#3972,#3973,#3974,#3975,#3976,#3977));
#4149=CLOSED_SHELL('',(#3978,#3979,#3980,#3981,#3982,#3983,#3984,#3985));
#4150=CLOSED_SHELL('',(#3986,#3987,#3988,#3989,#3990,#3991,#3992,#3993,
#3994,#3995,#3996,#3997,#3998,#3999,#4000,#4001,#4002,#4003,#4004,#4005,
#4006,#4007,#4008,#4009,#4010,#4011,#4012,#4013,#4014));
#4151=CLOSED_SHELL('',(#4015,#4016,#4017,#4018));
#4152=CLOSED_SHELL('',(#4019,#4020,#4021,#4022,#4023,#4024,#4025,#4026,
#4027,#4028,#4029,#4030,#4031,#4032,#4033,#4034,#4035,#4036,#4037,#4038,
#4039,#4040,#4041,#4042,#4043,#4044,#4045,#4046,#4047,#4048,#4049,#4050,
#4051,#4052,#4053,#4054,#4055,#4056,#4057,#4058,#4059,#4060,#4061,#4062,
#4063,#4064,#4065,#4066,#4067,#4068,#4069,#4070,#4071,#4072,#4073,#4074,
#4075,#4076,#4077,#4078,#4079,#4080,#4081,#4082,#4083,#4084,#4085,#4086,
#4087,#4088,#4089,#4090));
#4153=CLOSED_SHELL('',(#4091,#4092,#4093,#4094,#4095,#4096,#4097,#4098,
#4099,#4100));
#4154=CLOSED_SHELL('',(#4101,#4102,#4103,#4104,#4105,#4106));
#4155=CLOSED_SHELL('',(#4107,#4108,#4109,#4110));
#4156=CLOSED_SHELL('',(#4111,#4112,#4113,#4114,#4115,#4116));
#4157=CLOSED_SHELL('',(#4117,#4118,#4119));
#4158=CLOSED_SHELL('',(#4120,#4121,#4122,#4123,#4124));
#4159=CLOSED_SHELL('',(#4125,#4126,#4127,#4128,#4129,#4130,#4131,#4132,
#4133));
#4160=CLOSED_SHELL('',(#4134,#4135,#4136,#4137));
#4161=CLOSED_SHELL('',(#4138,#4139,#4140,#4141,#4142,#4143));
#4162=DERIVED_UNIT_ELEMENT(#4198,1.);
#4163=DERIVED_UNIT_ELEMENT(#37703,-3.);
#4164=DERIVED_UNIT_ELEMENT(#4198,1.);
#4165=DERIVED_UNIT_ELEMENT(#37703,-3.);
#4166=DERIVED_UNIT_ELEMENT(#4198,1.);
#4167=DERIVED_UNIT_ELEMENT(#37703,-3.);
#4168=DERIVED_UNIT_ELEMENT(#4198,1.);
#4169=DERIVED_UNIT_ELEMENT(#37703,-3.);
#4170=DERIVED_UNIT_ELEMENT(#4198,1.);
#4171=DERIVED_UNIT_ELEMENT(#37703,-3.);
#4172=DERIVED_UNIT_ELEMENT(#4198,1.);
#4173=DERIVED_UNIT_ELEMENT(#37703,-3.);
#4174=DERIVED_UNIT_ELEMENT(#4198,1.);
#4175=DERIVED_UNIT_ELEMENT(#37703,-3.);
#4176=DERIVED_UNIT_ELEMENT(#4198,1.);
#4177=DERIVED_UNIT_ELEMENT(#37703,-3.);
#4178=DERIVED_UNIT_ELEMENT(#4198,1.);
#4179=DERIVED_UNIT_ELEMENT(#37703,-3.);
#4180=DERIVED_UNIT_ELEMENT(#4198,1.);
#4181=DERIVED_UNIT_ELEMENT(#37703,-3.);
#4182=DERIVED_UNIT_ELEMENT(#4198,1.);
#4183=DERIVED_UNIT_ELEMENT(#37703,-3.);
#4184=DERIVED_UNIT_ELEMENT(#4198,1.);
#4185=DERIVED_UNIT_ELEMENT(#37703,-3.);
#4186=DERIVED_UNIT_ELEMENT(#4198,1.);
#4187=DERIVED_UNIT_ELEMENT(#37703,-3.);
#4188=DERIVED_UNIT_ELEMENT(#4198,1.);
#4189=DERIVED_UNIT_ELEMENT(#37703,-3.);
#4190=DERIVED_UNIT_ELEMENT(#4198,1.);
#4191=DERIVED_UNIT_ELEMENT(#37703,-3.);
#4192=DERIVED_UNIT_ELEMENT(#4198,1.);
#4193=DERIVED_UNIT_ELEMENT(#37703,-3.);
#4194=DERIVED_UNIT_ELEMENT(#4198,1.);
#4195=DERIVED_UNIT_ELEMENT(#37703,-3.);
#4196=DERIVED_UNIT_ELEMENT(#4198,1.);
#4197=DERIVED_UNIT_ELEMENT(#37703,-3.);
#4198=(
MASS_UNIT()
NAMED_UNIT(*)
SI_UNIT(.KILO.,.GRAM.)
);
#4199=DERIVED_UNIT((#4162,#4163));
#4200=DERIVED_UNIT((#4164,#4165));
#4201=DERIVED_UNIT((#4166,#4167));
#4202=DERIVED_UNIT((#4168,#4169));
#4203=DERIVED_UNIT((#4170,#4171));
#4204=DERIVED_UNIT((#4172,#4173));
#4205=DERIVED_UNIT((#4174,#4175));
#4206=DERIVED_UNIT((#4176,#4177));
#4207=DERIVED_UNIT((#4178,#4179));
#4208=DERIVED_UNIT((#4180,#4181));
#4209=DERIVED_UNIT((#4182,#4183));
#4210=DERIVED_UNIT((#4184,#4185));
#4211=DERIVED_UNIT((#4186,#4187));
#4212=DERIVED_UNIT((#4188,#4189));
#4213=DERIVED_UNIT((#4190,#4191));
#4214=DERIVED_UNIT((#4192,#4193));
#4215=DERIVED_UNIT((#4194,#4195));
#4216=DERIVED_UNIT((#4196,#4197));
#4217=MEASURE_REPRESENTATION_ITEM('density measure',
POSITIVE_RATIO_MEASURE(7850.),#4199);
#4218=MEASURE_REPRESENTATION_ITEM('density measure',
POSITIVE_RATIO_MEASURE(7850.),#4200);
#4219=MEASURE_REPRESENTATION_ITEM('density measure',
POSITIVE_RATIO_MEASURE(7850.),#4201);
#4220=MEASURE_REPRESENTATION_ITEM('density measure',
POSITIVE_RATIO_MEASURE(7850.),#4202);
#4221=MEASURE_REPRESENTATION_ITEM('density measure',
POSITIVE_RATIO_MEASURE(7850.),#4203);
#4222=MEASURE_REPRESENTATION_ITEM('density measure',
POSITIVE_RATIO_MEASURE(7850.),#4204);
#4223=MEASURE_REPRESENTATION_ITEM('density measure',
POSITIVE_RATIO_MEASURE(7850.),#4205);
#4224=MEASURE_REPRESENTATION_ITEM('density measure',
POSITIVE_RATIO_MEASURE(7850.),#4206);
#4225=MEASURE_REPRESENTATION_ITEM('density measure',
POSITIVE_RATIO_MEASURE(7850.),#4207);
#4226=MEASURE_REPRESENTATION_ITEM('density measure',
POSITIVE_RATIO_MEASURE(7850.),#4208);
#4227=MEASURE_REPRESENTATION_ITEM('density measure',
POSITIVE_RATIO_MEASURE(7850.),#4209);
#4228=MEASURE_REPRESENTATION_ITEM('density measure',
POSITIVE_RATIO_MEASURE(8920.),#4210);
#4229=MEASURE_REPRESENTATION_ITEM('density measure',
POSITIVE_RATIO_MEASURE(7850.),#4211);
#4230=MEASURE_REPRESENTATION_ITEM('density measure',
POSITIVE_RATIO_MEASURE(7850.),#4212);
#4231=MEASURE_REPRESENTATION_ITEM('density measure',
POSITIVE_RATIO_MEASURE(1250.),#4213);
#4232=MEASURE_REPRESENTATION_ITEM('density measure',
POSITIVE_RATIO_MEASURE(7850.),#4214);
#4233=MEASURE_REPRESENTATION_ITEM('density measure',
POSITIVE_RATIO_MEASURE(7850.),#4215);
#4234=MEASURE_REPRESENTATION_ITEM('density measure',
POSITIVE_RATIO_MEASURE(7850.),#4216);
#4235=PROPERTY_DEFINITION_REPRESENTATION(#4325,#4271);
#4236=PROPERTY_DEFINITION_REPRESENTATION(#4326,#4272);
#4237=PROPERTY_DEFINITION_REPRESENTATION(#4327,#4273);
#4238=PROPERTY_DEFINITION_REPRESENTATION(#4328,#4274);
#4239=PROPERTY_DEFINITION_REPRESENTATION(#4329,#4275);
#4240=PROPERTY_DEFINITION_REPRESENTATION(#4330,#4276);
#4241=PROPERTY_DEFINITION_REPRESENTATION(#4331,#4277);
#4242=PROPERTY_DEFINITION_REPRESENTATION(#4332,#4278);
#4243=PROPERTY_DEFINITION_REPRESENTATION(#4333,#4279);
#4244=PROPERTY_DEFINITION_REPRESENTATION(#4334,#4280);
#4245=PROPERTY_DEFINITION_REPRESENTATION(#4335,#4281);
#4246=PROPERTY_DEFINITION_REPRESENTATION(#4336,#4282);
#4247=PROPERTY_DEFINITION_REPRESENTATION(#4337,#4283);
#4248=PROPERTY_DEFINITION_REPRESENTATION(#4338,#4284);
#4249=PROPERTY_DEFINITION_REPRESENTATION(#4339,#4285);
#4250=PROPERTY_DEFINITION_REPRESENTATION(#4340,#4286);
#4251=PROPERTY_DEFINITION_REPRESENTATION(#4341,#4287);
#4252=PROPERTY_DEFINITION_REPRESENTATION(#4342,#4288);
#4253=PROPERTY_DEFINITION_REPRESENTATION(#4343,#4289);
#4254=PROPERTY_DEFINITION_REPRESENTATION(#4344,#4290);
#4255=PROPERTY_DEFINITION_REPRESENTATION(#4345,#4291);
#4256=PROPERTY_DEFINITION_REPRESENTATION(#4346,#4292);
#4257=PROPERTY_DEFINITION_REPRESENTATION(#4347,#4293);
#4258=PROPERTY_DEFINITION_REPRESENTATION(#4348,#4294);
#4259=PROPERTY_DEFINITION_REPRESENTATION(#4349,#4295);
#4260=PROPERTY_DEFINITION_REPRESENTATION(#4350,#4296);
#4261=PROPERTY_DEFINITION_REPRESENTATION(#4351,#4297);
#4262=PROPERTY_DEFINITION_REPRESENTATION(#4352,#4298);
#4263=PROPERTY_DEFINITION_REPRESENTATION(#4353,#4299);
#4264=PROPERTY_DEFINITION_REPRESENTATION(#4354,#4300);
#4265=PROPERTY_DEFINITION_REPRESENTATION(#4355,#4301);
#4266=PROPERTY_DEFINITION_REPRESENTATION(#4356,#4302);
#4267=PROPERTY_DEFINITION_REPRESENTATION(#4357,#4303);
#4268=PROPERTY_DEFINITION_REPRESENTATION(#4358,#4304);
#4269=PROPERTY_DEFINITION_REPRESENTATION(#4359,#4305);
#4270=PROPERTY_DEFINITION_REPRESENTATION(#4360,#4306);
#4271=REPRESENTATION('material name',(#4307),#37683);
#4272=REPRESENTATION('density',(#4217),#37683);
#4273=REPRESENTATION('material name',(#4308),#37684);
#4274=REPRESENTATION('density',(#4218),#37684);
#4275=REPRESENTATION('material name',(#4309),#37685);
#4276=REPRESENTATION('density',(#4219),#37685);
#4277=REPRESENTATION('material name',(#4310),#37686);
#4278=REPRESENTATION('density',(#4220),#37686);
#4279=REPRESENTATION('material name',(#4311),#37687);
#4280=REPRESENTATION('density',(#4221),#37687);
#4281=REPRESENTATION('material name',(#4312),#37688);
#4282=REPRESENTATION('density',(#4222),#37688);
#4283=REPRESENTATION('material name',(#4313),#37689);
#4284=REPRESENTATION('density',(#4223),#37689);
#4285=REPRESENTATION('material name',(#4314),#37690);
#4286=REPRESENTATION('density',(#4224),#37690);
#4287=REPRESENTATION('material name',(#4315),#37691);
#4288=REPRESENTATION('density',(#4225),#37691);
#4289=REPRESENTATION('material name',(#4316),#37692);
#4290=REPRESENTATION('density',(#4226),#37692);
#4291=REPRESENTATION('material name',(#4317),#37693);
#4292=REPRESENTATION('density',(#4227),#37693);
#4293=REPRESENTATION('material name',(#4318),#37694);
#4294=REPRESENTATION('density',(#4228),#37694);
#4295=REPRESENTATION('material name',(#4319),#37695);
#4296=REPRESENTATION('density',(#4229),#37695);
#4297=REPRESENTATION('material name',(#4320),#37696);
#4298=REPRESENTATION('density',(#4230),#37696);
#4299=REPRESENTATION('material name',(#4321),#37697);
#4300=REPRESENTATION('density',(#4231),#37697);
#4301=REPRESENTATION('material name',(#4322),#37698);
#4302=REPRESENTATION('density',(#4232),#37698);
#4303=REPRESENTATION('material name',(#4323),#37699);
#4304=REPRESENTATION('density',(#4233),#37699);
#4305=REPRESENTATION('material name',(#4324),#37700);
#4306=REPRESENTATION('density',(#4234),#37700);
#4307=DESCRIPTIVE_REPRESENTATION_ITEM('Steel','Steel');
#4308=DESCRIPTIVE_REPRESENTATION_ITEM('Steel','Steel');
#4309=DESCRIPTIVE_REPRESENTATION_ITEM('Steel','Steel');
#4310=DESCRIPTIVE_REPRESENTATION_ITEM('Steel','Steel');
#4311=DESCRIPTIVE_REPRESENTATION_ITEM('Steel','Steel');
#4312=DESCRIPTIVE_REPRESENTATION_ITEM('Steel','Steel');
#4313=DESCRIPTIVE_REPRESENTATION_ITEM('Steel','Steel');
#4314=DESCRIPTIVE_REPRESENTATION_ITEM('Steel','Steel');
#4315=DESCRIPTIVE_REPRESENTATION_ITEM('Steel','Steel');
#4316=DESCRIPTIVE_REPRESENTATION_ITEM('Steel','Steel');
#4317=DESCRIPTIVE_REPRESENTATION_ITEM('Steel','Steel');
#4318=DESCRIPTIVE_REPRESENTATION_ITEM('Copper, Alloy','Copper, Alloy');
#4319=DESCRIPTIVE_REPRESENTATION_ITEM('Steel','Steel');
#4320=DESCRIPTIVE_REPRESENTATION_ITEM('Steel','Steel');
#4321=DESCRIPTIVE_REPRESENTATION_ITEM('Rubber, Silicone',
'Rubber, Silicone');
#4322=DESCRIPTIVE_REPRESENTATION_ITEM('Steel','Steel');
#4323=DESCRIPTIVE_REPRESENTATION_ITEM('Steel','Steel');
#4324=DESCRIPTIVE_REPRESENTATION_ITEM('Steel','Steel');
#4325=PROPERTY_DEFINITION('material property','material name',#37799);
#4326=PROPERTY_DEFINITION('material property','density of part',#37799);
#4327=PROPERTY_DEFINITION('material property','material name',#37800);
#4328=PROPERTY_DEFINITION('material property','density of part',#37800);
#4329=PROPERTY_DEFINITION('material property','material name',#37801);
#4330=PROPERTY_DEFINITION('material property','density of part',#37801);
#4331=PROPERTY_DEFINITION('material property','material name',#37802);
#4332=PROPERTY_DEFINITION('material property','density of part',#37802);
#4333=PROPERTY_DEFINITION('material property','material name',#37803);
#4334=PROPERTY_DEFINITION('material property','density of part',#37803);
#4335=PROPERTY_DEFINITION('material property','material name',#37804);
#4336=PROPERTY_DEFINITION('material property','density of part',#37804);
#4337=PROPERTY_DEFINITION('material property','material name',#37805);
#4338=PROPERTY_DEFINITION('material property','density of part',#37805);
#4339=PROPERTY_DEFINITION('material property','material name',#37806);
#4340=PROPERTY_DEFINITION('material property','density of part',#37806);
#4341=PROPERTY_DEFINITION('material property','material name',#37807);
#4342=PROPERTY_DEFINITION('material property','density of part',#37807);
#4343=PROPERTY_DEFINITION('material property','material name',#37808);
#4344=PROPERTY_DEFINITION('material property','density of part',#37808);
#4345=PROPERTY_DEFINITION('material property','material name',#37809);
#4346=PROPERTY_DEFINITION('material property','density of part',#37809);
#4347=PROPERTY_DEFINITION('material property','material name',#37810);
#4348=PROPERTY_DEFINITION('material property','density of part',#37810);
#4349=PROPERTY_DEFINITION('material property','material name',#37811);
#4350=PROPERTY_DEFINITION('material property','density of part',#37811);
#4351=PROPERTY_DEFINITION('material property','material name',#37812);
#4352=PROPERTY_DEFINITION('material property','density of part',#37812);
#4353=PROPERTY_DEFINITION('material property','material name',#37813);
#4354=PROPERTY_DEFINITION('material property','density of part',#37813);
#4355=PROPERTY_DEFINITION('material property','material name',#37814);
#4356=PROPERTY_DEFINITION('material property','density of part',#37814);
#4357=PROPERTY_DEFINITION('material property','material name',#37815);
#4358=PROPERTY_DEFINITION('material property','density of part',#37815);
#4359=PROPERTY_DEFINITION('material property','material name',#37816);
#4360=PROPERTY_DEFINITION('material property','density of part',#37816);
#4361=AXIS2_PLACEMENT_3D('',#5648,#4707,#4708);
#4362=AXIS2_PLACEMENT_3D('',#5649,#4709,#4710);
#4363=AXIS2_PLACEMENT_3D('',#5650,#4711,#4712);
#4364=AXIS2_PLACEMENT_3D('',#5653,#4713,#4714);
#4365=AXIS2_PLACEMENT_3D('',#5657,#4716,#4717);
#4366=AXIS2_PLACEMENT_3D('',#5659,#4719,#4720);
#4367=AXIS2_PLACEMENT_3D('',#5665,#4724,#4725);
#4368=AXIS2_PLACEMENT_3D('',#5669,#4727,#4728);
#4369=AXIS2_PLACEMENT_3D('',#5673,#4730,#4731);
#4370=AXIS2_PLACEMENT_3D('',#5676,#4733,#4734);
#4371=AXIS2_PLACEMENT_3D('',#5678,#4735,#4736);
#4372=AXIS2_PLACEMENT_3D('',#5680,#4737,#4738);
#4373=AXIS2_PLACEMENT_3D('',#5682,#4739,#4740);
#4374=AXIS2_PLACEMENT_3D('',#5684,#4741,#4742);
#4375=AXIS2_PLACEMENT_3D('',#5685,#4743,#4744);
#4376=AXIS2_PLACEMENT_3D('',#5687,#4745,#4746);
#4377=AXIS2_PLACEMENT_3D('',#5689,#4748,#4749);
#4378=AXIS2_PLACEMENT_3D('',#5693,#4752,#4753);
#4379=AXIS2_PLACEMENT_3D('',#5695,#4754,#4755);
#4380=AXIS2_PLACEMENT_3D('',#5697,#4757,#4758);
#4381=AXIS2_PLACEMENT_3D('',#5701,#4761,#4762);
#4382=AXIS2_PLACEMENT_3D('',#5703,#4763,#4764);
#4383=AXIS2_PLACEMENT_3D('',#5705,#4766,#4767);
#4384=AXIS2_PLACEMENT_3D('',#5707,#4768,#4769);
#4385=AXIS2_PLACEMENT_3D('',#5709,#4771,#4772);
#4386=AXIS2_PLACEMENT_3D('',#5711,#4773,#4774);
#4387=AXIS2_PLACEMENT_3D('',#5713,#4776,#4777);
#4388=AXIS2_PLACEMENT_3D('',#5715,#4778,#4779);
#4389=AXIS2_PLACEMENT_3D('',#5717,#4781,#4782);
#4390=AXIS2_PLACEMENT_3D('',#5719,#4783,#4784);
#4391=AXIS2_PLACEMENT_3D('',#5721,#4786,#4787);
#4392=AXIS2_PLACEMENT_3D('',#5723,#4789,#4790);
#4393=AXIS2_PLACEMENT_3D('',#5724,#4791,#4792);
#4394=AXIS2_PLACEMENT_3D('',#5725,#4793,#4794);
#4395=AXIS2_PLACEMENT_3D('',#5727,#4795,#4796);
#4396=AXIS2_PLACEMENT_3D('',#5730,#4798,#4799);
#4397=AXIS2_PLACEMENT_3D('',#5731,#4800,#4801);
#4398=AXIS2_PLACEMENT_3D('',#5733,#4802,#4803);
#4399=AXIS2_PLACEMENT_3D('',#5736,#4805,#4806);
#4400=AXIS2_PLACEMENT_3D('',#5737,#4807,#4808);
#4401=AXIS2_PLACEMENT_3D('',#5746,#4813,#4814);
#4402=AXIS2_PLACEMENT_3D('',#5752,#4818,#4819);
#4403=AXIS2_PLACEMENT_3D('',#5758,#4823,#4824);
#4404=AXIS2_PLACEMENT_3D('',#5761,#4827,#4828);
#4405=AXIS2_PLACEMENT_3D('',#5762,#4829,#4830);
#4406=AXIS2_PLACEMENT_3D('',#5763,#4831,#4832);
#4407=AXIS2_PLACEMENT_3D('',#5764,#4833,#4834);
#4408=AXIS2_PLACEMENT_3D('',#5766,#4835,#4836);
#4409=AXIS2_PLACEMENT_3D('',#5769,#4838,#4839);
#4410=AXIS2_PLACEMENT_3D('',#5770,#4840,#4841);
#4411=AXIS2_PLACEMENT_3D('',#5772,#4842,#4843);
#4412=AXIS2_PLACEMENT_3D('',#5775,#4845,#4846);
#4413=AXIS2_PLACEMENT_3D('',#5776,#4847,#4848);
#4414=AXIS2_PLACEMENT_3D('',#5785,#4853,#4854);
#4415=AXIS2_PLACEMENT_3D('',#5791,#4858,#4859);
#4416=AXIS2_PLACEMENT_3D('',#5797,#4863,#4864);
#4417=AXIS2_PLACEMENT_3D('',#5800,#4867,#4868);
#4418=AXIS2_PLACEMENT_3D('',#5801,#4869,#4870);
#4419=AXIS2_PLACEMENT_3D('',#5802,#4871,#4872);
#4420=AXIS2_PLACEMENT_3D('',#5803,#4873,#4874);
#4421=AXIS2_PLACEMENT_3D('',#5808,#4876,#4877);
#4422=AXIS2_PLACEMENT_3D('',#5811,#4879,#4880);
#4423=AXIS2_PLACEMENT_3D('',#5812,#4881,#4882);
#4424=AXIS2_PLACEMENT_3D('',#5817,#4885,#4886);
#4425=AXIS2_PLACEMENT_3D('',#5818,#4887,#4888);
#4426=AXIS2_PLACEMENT_3D('',#5823,#4891,#4892);
#4427=AXIS2_PLACEMENT_3D('',#5824,#4893,#4894);
#4428=AXIS2_PLACEMENT_3D('',#5827,#4897,#4898);
#4429=AXIS2_PLACEMENT_3D('',#5833,#4902,#4903);
#4430=AXIS2_PLACEMENT_3D('',#5837,#4906,#4907);
#4431=AXIS2_PLACEMENT_3D('',#5838,#4908,#4909);
#4432=AXIS2_PLACEMENT_3D('',#5842,#4912,#4913);
#4433=AXIS2_PLACEMENT_3D('',#5844,#4915,#4916);
#4434=AXIS2_PLACEMENT_3D('',#5845,#4917,#4918);
#4435=AXIS2_PLACEMENT_3D('',#5846,#4919,#4920);
#4436=AXIS2_PLACEMENT_3D('',#5855,#4925,#4926);
#4437=AXIS2_PLACEMENT_3D('',#5861,#4930,#4931);
#4438=AXIS2_PLACEMENT_3D('',#5867,#4935,#4936);
#4439=AXIS2_PLACEMENT_3D('',#5870,#4939,#4940);
#4440=AXIS2_PLACEMENT_3D('',#5871,#4941,#4942);
#4441=AXIS2_PLACEMENT_3D('',#5872,#4943,#4944);
#4442=AXIS2_PLACEMENT_3D('',#5873,#4945,#4946);
#4443=AXIS2_PLACEMENT_3D('',#5875,#4947,#4948);
#4444=AXIS2_PLACEMENT_3D('',#5878,#4950,#4951);
#4445=AXIS2_PLACEMENT_3D('',#5879,#4952,#4953);
#4446=AXIS2_PLACEMENT_3D('',#5888,#4958,#4959);
#4447=AXIS2_PLACEMENT_3D('',#5894,#4963,#4964);
#4448=AXIS2_PLACEMENT_3D('',#5900,#4968,#4969);
#4449=AXIS2_PLACEMENT_3D('',#5906,#4973,#4974);
#4450=AXIS2_PLACEMENT_3D('',#5907,#4975,#4976);
#4451=AXIS2_PLACEMENT_3D('',#5908,#4977,#4978);
#4452=AXIS2_PLACEMENT_3D('',#5909,#4979,#4980);
#4453=AXIS2_PLACEMENT_3D('',#5910,#4981,#4982);
#4454=AXIS2_PLACEMENT_3D('',#5911,#4983,#4984);
#4455=AXIS2_PLACEMENT_3D('',#5912,#4985,#4986);
#4456=AXIS2_PLACEMENT_3D('',#5936,#4988,#4989);
#4457=AXIS2_PLACEMENT_3D('',#6002,#4990,#4991);
#4458=AXIS2_PLACEMENT_3D('',#6186,#4993,#4994);
#4459=AXIS2_PLACEMENT_3D('',#6585,#4996,#4997);
#4460=AXIS2_PLACEMENT_3D('',#6779,#4999,#5000);
#4461=AXIS2_PLACEMENT_3D('',#7102,#5002,#5003);
#4462=AXIS2_PLACEMENT_3D('',#7574,#5005,#5006);
#4463=AXIS2_PLACEMENT_3D('',#8049,#5008,#5009);
#4464=AXIS2_PLACEMENT_3D('',#8386,#5011,#5012);
#4465=AXIS2_PLACEMENT_3D('',#8784,#5014,#5015);
#4466=AXIS2_PLACEMENT_3D('',#9256,#5017,#5018);
#4467=AXIS2_PLACEMENT_3D('',#9278,#5020,#5021);
#4468=AXIS2_PLACEMENT_3D('',#9435,#5022,#5023);
#4469=AXIS2_PLACEMENT_3D('',#9509,#5025,#5026);
#4470=AXIS2_PLACEMENT_3D('',#9608,#5027,#5028);
#4471=AXIS2_PLACEMENT_3D('',#9845,#5030,#5031);
#4472=AXIS2_PLACEMENT_3D('',#10104,#5033,#5034);
#4473=AXIS2_PLACEMENT_3D('',#10370,#5036,#5037);
#4474=AXIS2_PLACEMENT_3D('',#10703,#5039,#5040);
#4475=AXIS2_PLACEMENT_3D('',#10843,#5042,#5043);
#4476=AXIS2_PLACEMENT_3D('',#11006,#5045,#5046);
#4477=AXIS2_PLACEMENT_3D('',#11346,#5048,#5049);
#4478=AXIS2_PLACEMENT_3D('',#11580,#5051,#5052);
#4479=AXIS2_PLACEMENT_3D('',#11805,#5054,#5055);
#4480=AXIS2_PLACEMENT_3D('',#11932,#5057,#5058);
#4481=AXIS2_PLACEMENT_3D('',#12019,#5059,#5060);
#4482=AXIS2_PLACEMENT_3D('',#12174,#5061,#5062);
#4483=AXIS2_PLACEMENT_3D('',#14143,#5063,#5064);
#4484=AXIS2_PLACEMENT_3D('',#14145,#5065,#5066);
#4485=AXIS2_PLACEMENT_3D('',#14146,#5067,#5068);
#4486=AXIS2_PLACEMENT_3D('',#14149,#5070,#5071);
#4487=AXIS2_PLACEMENT_3D('',#14150,#5072,#5073);
#4488=AXIS2_PLACEMENT_3D('',#14151,#5074,#5075);
#4489=AXIS2_PLACEMENT_3D('',#14152,#5076,#5077);
#4490=AXIS2_PLACEMENT_3D('',#14154,#5078,#5079);
#4491=AXIS2_PLACEMENT_3D('',#14157,#5081,#5082);
#4492=AXIS2_PLACEMENT_3D('',#14158,#5083,#5084);
#4493=AXIS2_PLACEMENT_3D('',#14160,#5085,#5086);
#4494=AXIS2_PLACEMENT_3D('',#14163,#5088,#5089);
#4495=AXIS2_PLACEMENT_3D('',#14164,#5090,#5091);
#4496=AXIS2_PLACEMENT_3D('',#14165,#5092,#5093);
#4497=AXIS2_PLACEMENT_3D('',#14166,#5094,#5095);
#4498=AXIS2_PLACEMENT_3D('',#14167,#5096,#5097);
#4499=AXIS2_PLACEMENT_3D('',#14249,#5099,#5100);
#4500=AXIS2_PLACEMENT_3D('',#14256,#5101,#5102);
#4501=AXIS2_PLACEMENT_3D('',#14505,#5104,#5105);
#4502=AXIS2_PLACEMENT_3D('',#14543,#5107,#5108);
#4503=AXIS2_PLACEMENT_3D('',#15008,#5110,#5111);
#4504=AXIS2_PLACEMENT_3D('',#15473,#5113,#5114);
#4505=AXIS2_PLACEMENT_3D('',#15723,#5116,#5117);
#4506=AXIS2_PLACEMENT_3D('',#15972,#5119,#5120);
#4507=AXIS2_PLACEMENT_3D('',#16222,#5122,#5123);
#4508=AXIS2_PLACEMENT_3D('',#16471,#5125,#5126);
#4509=AXIS2_PLACEMENT_3D('',#16721,#5128,#5129);
#4510=AXIS2_PLACEMENT_3D('',#17186,#5131,#5132);
#4511=AXIS2_PLACEMENT_3D('',#17648,#5134,#5135);
#4512=AXIS2_PLACEMENT_3D('',#17898,#5137,#5138);
#4513=AXIS2_PLACEMENT_3D('',#18147,#5140,#5141);
#4514=AXIS2_PLACEMENT_3D('',#18398,#5143,#5144);
#4515=AXIS2_PLACEMENT_3D('',#18437,#5146,#5147);
#4516=AXIS2_PLACEMENT_3D('',#18686,#5149,#5150);
#4517=AXIS2_PLACEMENT_3D('',#18936,#5152,#5153);
#4518=AXIS2_PLACEMENT_3D('',#19185,#5155,#5156);
#4519=AXIS2_PLACEMENT_3D('',#19223,#5158,#5159);
#4520=AXIS2_PLACEMENT_3D('',#19685,#5161,#5162);
#4521=AXIS2_PLACEMENT_3D('',#19937,#5164,#5165);
#4522=AXIS2_PLACEMENT_3D('',#20399,#5167,#5168);
#4523=AXIS2_PLACEMENT_3D('',#20864,#5170,#5171);
#4524=AXIS2_PLACEMENT_3D('',#21114,#5173,#5174);
#4525=AXIS2_PLACEMENT_3D('',#21151,#5176,#5177);
#4526=AXIS2_PLACEMENT_3D('',#21404,#5179,#5180);
#4527=AXIS2_PLACEMENT_3D('',#21866,#5182,#5183);
#4528=AXIS2_PLACEMENT_3D('',#22088,#5185,#5186);
#4529=AXIS2_PLACEMENT_3D('',#22228,#5187,#5188);
#4530=AXIS2_PLACEMENT_3D('',#22496,#5190,#5191);
#4531=AXIS2_PLACEMENT_3D('',#23020,#5193,#5194);
#4532=AXIS2_PLACEMENT_3D('',#23621,#5196,#5197);
#4533=AXIS2_PLACEMENT_3D('',#24103,#5199,#5200);
#4534=AXIS2_PLACEMENT_3D('',#24392,#5202,#5203);
#4535=AXIS2_PLACEMENT_3D('',#24870,#5205,#5206);
#4536=AXIS2_PLACEMENT_3D('',#25409,#5208,#5209);
#4537=AXIS2_PLACEMENT_3D('',#25928,#5211,#5212);
#4538=AXIS2_PLACEMENT_3D('',#26403,#5214,#5215);
#4539=AXIS2_PLACEMENT_3D('',#26902,#5217,#5218);
#4540=AXIS2_PLACEMENT_3D('',#27401,#5220,#5221);
#4541=AXIS2_PLACEMENT_3D('',#27461,#5223,#5224);
#4542=AXIS2_PLACEMENT_3D('',#27934,#5226,#5227);
#4543=AXIS2_PLACEMENT_3D('',#28211,#5229,#5230);
#4544=AXIS2_PLACEMENT_3D('',#28718,#5232,#5233);
#4545=AXIS2_PLACEMENT_3D('',#29224,#5235,#5236);
#4546=AXIS2_PLACEMENT_3D('',#29726,#5238,#5239);
#4547=AXIS2_PLACEMENT_3D('',#30014,#5241,#5242);
#4548=AXIS2_PLACEMENT_3D('',#30272,#5244,#5245);
#4549=AXIS2_PLACEMENT_3D('',#30759,#5247,#5248);
#4550=AXIS2_PLACEMENT_3D('',#31038,#5250,#5251);
#4551=AXIS2_PLACEMENT_3D('',#31333,#5253,#5254);
#4552=AXIS2_PLACEMENT_3D('',#31813,#5256,#5257);
#4553=AXIS2_PLACEMENT_3D('',#32292,#5259,#5260);
#4554=AXIS2_PLACEMENT_3D('',#32599,#5262,#5263);
#4555=AXIS2_PLACEMENT_3D('',#33066,#5265,#5266);
#4556=AXIS2_PLACEMENT_3D('',#33345,#5268,#5269);
#4557=AXIS2_PLACEMENT_3D('',#33565,#5270,#5271);
#4558=AXIS2_PLACEMENT_3D('',#33743,#5272,#5273);
#4559=AXIS2_PLACEMENT_3D('',#33761,#5274,#5275);
#4560=AXIS2_PLACEMENT_3D('',#33931,#5276,#5277);
#4561=AXIS2_PLACEMENT_3D('',#34205,#5278,#5279);
#4562=AXIS2_PLACEMENT_3D('',#35672,#5280,#5281);
#4563=AXIS2_PLACEMENT_3D('',#37364,#5282,#5283);
#4564=AXIS2_PLACEMENT_3D('',#37365,#5284,#5285);
#4565=AXIS2_PLACEMENT_3D('',#37374,#5290,#5291);
#4566=AXIS2_PLACEMENT_3D('',#37380,#5295,#5296);
#4567=AXIS2_PLACEMENT_3D('',#37386,#5300,#5301);
#4568=AXIS2_PLACEMENT_3D('',#37392,#5305,#5306);
#4569=AXIS2_PLACEMENT_3D('',#37398,#5310,#5311);
#4570=AXIS2_PLACEMENT_3D('',#37401,#5314,#5315);
#4571=AXIS2_PLACEMENT_3D('',#37402,#5316,#5317);
#4572=AXIS2_PLACEMENT_3D('',#37404,#5318,#5319);
#4573=AXIS2_PLACEMENT_3D('',#37405,#5320,#5321);
#4574=AXIS2_PLACEMENT_3D('',#37408,#5323,#5324);
#4575=AXIS2_PLACEMENT_3D('',#37409,#5325,#5326);
#4576=AXIS2_PLACEMENT_3D('',#37410,#5327,#5328);
#4577=AXIS2_PLACEMENT_3D('',#37411,#5329,#5330);
#4578=AXIS2_PLACEMENT_3D('',#37412,#5331,#5332);
#4579=AXIS2_PLACEMENT_3D('',#37415,#5333,#5334);
#4580=AXIS2_PLACEMENT_3D('',#37419,#5336,#5337);
#4581=AXIS2_PLACEMENT_3D('',#37421,#5339,#5340);
#4582=AXIS2_PLACEMENT_3D('',#37427,#5344,#5345);
#4583=AXIS2_PLACEMENT_3D('',#37431,#5347,#5348);
#4584=AXIS2_PLACEMENT_3D('',#37435,#5350,#5351);
#4585=AXIS2_PLACEMENT_3D('',#37438,#5353,#5354);
#4586=AXIS2_PLACEMENT_3D('',#37439,#5355,#5356);
#4587=AXIS2_PLACEMENT_3D('',#37442,#5357,#5358);
#4588=AXIS2_PLACEMENT_3D('',#37445,#5361,#5362);
#4589=AXIS2_PLACEMENT_3D('',#37449,#5365,#5366);
#4590=AXIS2_PLACEMENT_3D('',#37451,#5367,#5368);
#4591=AXIS2_PLACEMENT_3D('',#37453,#5370,#5371);
#4592=AXIS2_PLACEMENT_3D('',#37455,#5373,#5374);
#4593=AXIS2_PLACEMENT_3D('',#37457,#5375,#5376);
#4594=AXIS2_PLACEMENT_3D('',#37459,#5378,#5379);
#4595=AXIS2_PLACEMENT_3D('',#37461,#5381,#5382);
#4596=AXIS2_PLACEMENT_3D('',#37462,#5383,#5384);
#4597=AXIS2_PLACEMENT_3D('',#37463,#5385,#5386);
#4598=AXIS2_PLACEMENT_3D('',#37472,#5391,#5392);
#4599=AXIS2_PLACEMENT_3D('',#37478,#5396,#5397);
#4600=AXIS2_PLACEMENT_3D('',#37484,#5401,#5402);
#4601=AXIS2_PLACEMENT_3D('',#37487,#5405,#5406);
#4602=AXIS2_PLACEMENT_3D('',#37488,#5407,#5408);
#4603=AXIS2_PLACEMENT_3D('',#37489,#5409,#5410);
#4604=AXIS2_PLACEMENT_3D('',#37490,#5411,#5412);
#4605=AXIS2_PLACEMENT_3D('',#37492,#5413,#5414);
#4606=AXIS2_PLACEMENT_3D('',#37495,#5416,#5417);
#4607=AXIS2_PLACEMENT_3D('',#37496,#5418,#5419);
#4608=AXIS2_PLACEMENT_3D('',#37498,#5420,#5421);
#4609=AXIS2_PLACEMENT_3D('',#37501,#5423,#5424);
#4610=AXIS2_PLACEMENT_3D('',#37502,#5425,#5426);
#4611=AXIS2_PLACEMENT_3D('',#37503,#5427,#5428);
#4612=AXIS2_PLACEMENT_3D('',#37504,#5429,#5430);
#4613=AXIS2_PLACEMENT_3D('',#37505,#5431,#5432);
#4614=AXIS2_PLACEMENT_3D('',#37514,#5437,#5438);
#4615=AXIS2_PLACEMENT_3D('',#37520,#5442,#5443);
#4616=AXIS2_PLACEMENT_3D('',#37526,#5447,#5448);
#4617=AXIS2_PLACEMENT_3D('',#37529,#5451,#5452);
#4618=AXIS2_PLACEMENT_3D('',#37530,#5453,#5454);
#4619=AXIS2_PLACEMENT_3D('',#37531,#5455,#5456);
#4620=AXIS2_PLACEMENT_3D('',#37532,#5457,#5458);
#4621=AXIS2_PLACEMENT_3D('',#37534,#5459,#5460);
#4622=AXIS2_PLACEMENT_3D('',#37537,#5462,#5463);
#4623=AXIS2_PLACEMENT_3D('',#37538,#5464,#5465);
#4624=AXIS2_PLACEMENT_3D('',#37539,#5466,#5467);
#4625=AXIS2_PLACEMENT_3D('',#37540,#5468,#5469);
#4626=AXIS2_PLACEMENT_3D('',#37541,#5470,#5471);
#4627=AXIS2_PLACEMENT_3D('',#37543,#5472,#5473);
#4628=AXIS2_PLACEMENT_3D('',#37544,#5474,#5475);
#4629=AXIS2_PLACEMENT_3D('',#37546,#5476,#5477);
#4630=AXIS2_PLACEMENT_3D('',#37547,#5478,#5479);
#4631=AXIS2_PLACEMENT_3D('',#37549,#5480,#5481);
#4632=AXIS2_PLACEMENT_3D('',#37551,#5483,#5484);
#4633=AXIS2_PLACEMENT_3D('',#37554,#5486,#5487);
#4634=AXIS2_PLACEMENT_3D('',#37555,#5488,#5489);
#4635=AXIS2_PLACEMENT_3D('',#37556,#5490,#5491);
#4636=AXIS2_PLACEMENT_3D('',#37557,#5492,#5493);
#4637=AXIS2_PLACEMENT_3D('',#37559,#5494,#5495);
#4638=AXIS2_PLACEMENT_3D('',#37562,#5497,#5498);
#4639=AXIS2_PLACEMENT_3D('',#37563,#5499,#5500);
#4640=AXIS2_PLACEMENT_3D('',#37565,#5501,#5502);
#4641=AXIS2_PLACEMENT_3D('',#37566,#5503,#5504);
#4642=AXIS2_PLACEMENT_3D('',#37568,#5505,#5506);
#4643=AXIS2_PLACEMENT_3D('',#37569,#5507,#5508);
#4644=AXIS2_PLACEMENT_3D('',#37571,#5509,#5510);
#4645=AXIS2_PLACEMENT_3D('',#37573,#5512,#5513);
#4646=AXIS2_PLACEMENT_3D('',#37575,#5514,#5515);
#4647=AXIS2_PLACEMENT_3D('',#37577,#5516,#5517);
#4648=AXIS2_PLACEMENT_3D('',#37578,#5518,#5519);
#4649=AXIS2_PLACEMENT_3D('',#37581,#5521,#5522);
#4650=AXIS2_PLACEMENT_3D('',#37582,#5523,#5524);
#4651=AXIS2_PLACEMENT_3D('',#37583,#5525,#5526);
#4652=AXIS2_PLACEMENT_3D('',#37585,#5528,#5529);
#4653=AXIS2_PLACEMENT_3D('',#37586,#5530,#5531);
#4654=AXIS2_PLACEMENT_3D('',#37587,#5532,#5533);
#4655=AXIS2_PLACEMENT_3D('',#37589,#5534,#5535);
#4656=AXIS2_PLACEMENT_3D('',#37592,#5537,#5538);
#4657=AXIS2_PLACEMENT_3D('',#37593,#5539,#5540);
#4658=AXIS2_PLACEMENT_3D('',#37595,#5541,#5542);
#4659=AXIS2_PLACEMENT_3D('',#37598,#5544,#5545);
#4660=AXIS2_PLACEMENT_3D('',#37599,#5546,#5547);
#4661=AXIS2_PLACEMENT_3D('',#37600,#5548,#5549);
#4662=AXIS2_PLACEMENT_3D('',#37601,#5550,#5551);
#4663=AXIS2_PLACEMENT_3D('',#37602,#5552,#5553);
#4664=AXIS2_PLACEMENT_3D('',#37611,#5558,#5559);
#4665=AXIS2_PLACEMENT_3D('',#37620,#5564,#5565);
#4666=AXIS2_PLACEMENT_3D('',#37621,#5566,#5567);
#4667=AXIS2_PLACEMENT_3D('',#37622,#5568,#5569);
#4668=AXIS2_PLACEMENT_3D('',#37623,#5570,#5571);
#4669=AXIS2_PLACEMENT_3D('',#37624,#5572,#5573);
#4670=AXIS2_PLACEMENT_3D('',#37625,#5574,#5575);
#4671=AXIS2_PLACEMENT_3D('',#37626,#5576,#5577);
#4672=AXIS2_PLACEMENT_3D('',#37627,#5578,#5579);
#4673=AXIS2_PLACEMENT_3D('',#37628,#5580,#5581);
#4674=AXIS2_PLACEMENT_3D('',#37629,#5582,#5583);
#4675=AXIS2_PLACEMENT_3D('',#37630,#5584,#5585);
#4676=AXIS2_PLACEMENT_3D('',#37631,#5586,#5587);
#4677=AXIS2_PLACEMENT_3D('',#37632,#5588,#5589);
#4678=AXIS2_PLACEMENT_3D('',#37633,#5590,#5591);
#4679=AXIS2_PLACEMENT_3D('',#37634,#5592,#5593);
#4680=AXIS2_PLACEMENT_3D('',#37635,#5594,#5595);
#4681=AXIS2_PLACEMENT_3D('',#37636,#5596,#5597);
#4682=AXIS2_PLACEMENT_3D('',#37637,#5598,#5599);
#4683=AXIS2_PLACEMENT_3D('',#37638,#5600,#5601);
#4684=AXIS2_PLACEMENT_3D('',#37639,#5602,#5603);
#4685=AXIS2_PLACEMENT_3D('',#37640,#5604,#5605);
#4686=AXIS2_PLACEMENT_3D('',#37641,#5606,#5607);
#4687=AXIS2_PLACEMENT_3D('',#37642,#5608,#5609);
#4688=AXIS2_PLACEMENT_3D('',#37643,#5610,#5611);
#4689=AXIS2_PLACEMENT_3D('',#37644,#5612,#5613);
#4690=AXIS2_PLACEMENT_3D('',#37645,#5614,#5615);
#4691=AXIS2_PLACEMENT_3D('',#37646,#5616,#5617);
#4692=AXIS2_PLACEMENT_3D('',#37647,#5618,#5619);
#4693=AXIS2_PLACEMENT_3D('',#37648,#5620,#5621);
#4694=AXIS2_PLACEMENT_3D('',#37649,#5622,#5623);
#4695=AXIS2_PLACEMENT_3D('',#37650,#5624,#5625);
#4696=AXIS2_PLACEMENT_3D('',#37651,#5626,#5627);
#4697=AXIS2_PLACEMENT_3D('',#37652,#5628,#5629);
#4698=AXIS2_PLACEMENT_3D('',#37653,#5630,#5631);
#4699=AXIS2_PLACEMENT_3D('',#37654,#5632,#5633);
#4700=AXIS2_PLACEMENT_3D('',#37655,#5634,#5635);
#4701=AXIS2_PLACEMENT_3D('',#37656,#5636,#5637);
#4702=AXIS2_PLACEMENT_3D('',#37657,#5638,#5639);
#4703=AXIS2_PLACEMENT_3D('',#37658,#5640,#5641);
#4704=AXIS2_PLACEMENT_3D('',#37659,#5642,#5643);
#4705=AXIS2_PLACEMENT_3D('',#37660,#5644,#5645);
#4706=AXIS2_PLACEMENT_3D('',#37661,#5646,#5647);
#4707=DIRECTION('axis',(0.,0.,1.));
#4708=DIRECTION('refdir',(1.,0.,0.));
#4709=DIRECTION('axis',(0.,0.,1.));
#4710=DIRECTION('refdir',(1.,0.,0.));
#4711=DIRECTION('center_axis',(0.,0.,1.));
#4712=DIRECTION('ref_axis',(0.707106781186548,0.707106781186548,0.));
#4713=DIRECTION('center_axis',(0.,0.,-1.));
#4714=DIRECTION('ref_axis',(0.707106781186548,0.707106781186548,0.));
#4715=DIRECTION('',(0.,0.,-1.));
#4716=DIRECTION('center_axis',(0.,0.,1.));
#4717=DIRECTION('ref_axis',(0.707106781186548,0.707106781186548,0.));
#4718=DIRECTION('',(0.,0.,1.));
#4719=DIRECTION('center_axis',(0.,1.,0.));
#4720=DIRECTION('ref_axis',(-1.,0.,0.));
#4721=DIRECTION('',(1.,0.,0.));
#4722=DIRECTION('',(0.,0.,-1.));
#4723=DIRECTION('',(1.,0.,0.));
#4724=DIRECTION('center_axis',(0.,0.,1.));
#4725=DIRECTION('ref_axis',(1.,0.,0.));
#4726=DIRECTION('',(0.,-1.,0.));
#4727=DIRECTION('center_axis',(0.,0.,1.));
#4728=DIRECTION('ref_axis',(0.707106781186548,-0.707106781186548,0.));
#4729=DIRECTION('',(-1.,0.,0.));
#4730=DIRECTION('center_axis',(0.,0.,1.));
#4731=DIRECTION('ref_axis',(-0.707106781186548,-0.707106781186548,0.));
#4732=DIRECTION('',(0.,1.,0.));
#4733=DIRECTION('center_axis',(0.,0.,1.));
#4734=DIRECTION('ref_axis',(-0.707106781186548,0.707106781186548,0.));
#4735=DIRECTION('center_axis',(0.,0.,1.));
#4736=DIRECTION('ref_axis',(1.,0.,0.));
#4737=DIRECTION('center_axis',(0.,0.,1.));
#4738=DIRECTION('ref_axis',(1.,0.,0.));
#4739=DIRECTION('center_axis',(0.,0.,1.));
#4740=DIRECTION('ref_axis',(1.,0.,0.));
#4741=DIRECTION('center_axis',(0.,0.,1.));
#4742=DIRECTION('ref_axis',(1.,0.,0.));
#4743=DIRECTION('center_axis',(0.,0.,1.));
#4744=DIRECTION('ref_axis',(-0.707106781186548,0.707106781186548,0.));
#4745=DIRECTION('center_axis',(0.,0.,-1.));
#4746=DIRECTION('ref_axis',(-0.707106781186548,0.707106781186548,0.));
#4747=DIRECTION('',(0.,0.,1.));
#4748=DIRECTION('center_axis',(-1.,0.,0.));
#4749=DIRECTION('ref_axis',(0.,-1.,0.));
#4750=DIRECTION('',(0.,0.,-1.));
#4751=DIRECTION('',(0.,1.,0.));
#4752=DIRECTION('center_axis',(0.,0.,1.));
#4753=DIRECTION('ref_axis',(-0.707106781186548,-0.707106781186548,0.));
#4754=DIRECTION('center_axis',(0.,0.,-1.));
#4755=DIRECTION('ref_axis',(-0.707106781186548,-0.707106781186548,0.));
#4756=DIRECTION('',(0.,0.,1.));
#4757=DIRECTION('center_axis',(0.,-1.,0.));
#4758=DIRECTION('ref_axis',(1.,0.,0.));
#4759=DIRECTION('',(0.,0.,-1.));
#4760=DIRECTION('',(-1.,0.,0.));
#4761=DIRECTION('center_axis',(0.,0.,1.));
#4762=DIRECTION('ref_axis',(0.707106781186548,-0.707106781186548,0.));
#4763=DIRECTION('center_axis',(0.,0.,-1.));
#4764=DIRECTION('ref_axis',(0.707106781186548,-0.707106781186548,0.));
#4765=DIRECTION('',(0.,0.,1.));
#4766=DIRECTION('center_axis',(0.,0.,-1.));
#4767=DIRECTION('ref_axis',(1.,0.,0.));
#4768=DIRECTION('center_axis',(0.,0.,-1.));
#4769=DIRECTION('ref_axis',(1.,0.,0.));
#4770=DIRECTION('',(0.,0.,-1.));
#4771=DIRECTION('center_axis',(0.,0.,-1.));
#4772=DIRECTION('ref_axis',(1.,0.,0.));
#4773=DIRECTION('center_axis',(0.,0.,-1.));
#4774=DIRECTION('ref_axis',(1.,0.,0.));
#4775=DIRECTION('',(0.,0.,-1.));
#4776=DIRECTION('center_axis',(0.,0.,-1.));
#4777=DIRECTION('ref_axis',(1.,0.,0.));
#4778=DIRECTION('center_axis',(0.,0.,-1.));
#4779=DIRECTION('ref_axis',(1.,0.,0.));
#4780=DIRECTION('',(0.,0.,-1.));
#4781=DIRECTION('center_axis',(0.,0.,-1.));
#4782=DIRECTION('ref_axis',(1.,0.,0.));
#4783=DIRECTION('center_axis',(0.,0.,-1.));
#4784=DIRECTION('ref_axis',(1.,0.,0.));
#4785=DIRECTION('',(0.,0.,-1.));
#4786=DIRECTION('center_axis',(1.,0.,0.));
#4787=DIRECTION('ref_axis',(0.,1.,0.));
#4788=DIRECTION('',(0.,-1.,0.));
#4789=DIRECTION('center_axis',(0.,0.,1.));
#4790=DIRECTION('ref_axis',(1.,0.,0.));
#4791=DIRECTION('axis',(0.,0.,1.));
#4792=DIRECTION('refdir',(1.,0.,0.));
#4793=DIRECTION('center_axis',(0.,0.,-1.));
#4794=DIRECTION('ref_axis',(1.,0.,0.));
#4795=DIRECTION('center_axis',(0.,0.,-1.));
#4796=DIRECTION('ref_axis',(1.,0.,0.));
#4797=DIRECTION('',(0.,0.,-1.));
#4798=DIRECTION('center_axis',(0.,0.,1.));
#4799=DIRECTION('ref_axis',(1.,0.,0.));
#4800=DIRECTION('center_axis',(0.,0.,-1.));
#4801=DIRECTION('ref_axis',(1.,0.,0.));
#4802=DIRECTION('center_axis',(0.,0.,-1.));
#4803=DIRECTION('ref_axis',(1.,0.,0.));
#4804=DIRECTION('',(0.,0.,-1.));
#4805=DIRECTION('center_axis',(0.,0.,1.));
#4806=DIRECTION('ref_axis',(1.,0.,0.));
#4807=DIRECTION('center_axis',(0.,1.,0.));
#4808=DIRECTION('ref_axis',(-1.,0.,0.));
#4809=DIRECTION('',(-1.,0.,0.));
#4810=DIRECTION('',(0.,0.,1.));
#4811=DIRECTION('',(-1.,0.,0.));
#4812=DIRECTION('',(0.,0.,1.));
#4813=DIRECTION('center_axis',(1.,0.,0.));
#4814=DIRECTION('ref_axis',(0.,1.,0.));
#4815=DIRECTION('',(0.,1.,0.));
#4816=DIRECTION('',(0.,1.,0.));
#4817=DIRECTION('',(0.,0.,1.));
#4818=DIRECTION('center_axis',(0.,-1.,0.));
#4819=DIRECTION('ref_axis',(1.,0.,0.));
#4820=DIRECTION('',(1.,0.,0.));
#4821=DIRECTION('',(1.,0.,0.));
#4822=DIRECTION('',(0.,0.,1.));
#4823=DIRECTION('center_axis',(-1.,0.,0.));
#4824=DIRECTION('ref_axis',(0.,-1.,0.));
#4825=DIRECTION('',(0.,-1.,0.));
#4826=DIRECTION('',(0.,-1.,0.));
#4827=DIRECTION('center_axis',(0.,0.,1.));
#4828=DIRECTION('ref_axis',(1.,0.,0.));
#4829=DIRECTION('center_axis',(0.,0.,1.));
#4830=DIRECTION('ref_axis',(1.,0.,0.));
#4831=DIRECTION('axis',(0.,0.,1.));
#4832=DIRECTION('refdir',(1.,0.,0.));
#4833=DIRECTION('center_axis',(0.,0.,-1.));
#4834=DIRECTION('ref_axis',(1.,0.,0.));
#4835=DIRECTION('center_axis',(0.,0.,-1.));
#4836=DIRECTION('ref_axis',(1.,0.,0.));
#4837=DIRECTION('',(0.,0.,-1.));
#4838=DIRECTION('center_axis',(0.,0.,1.));
#4839=DIRECTION('ref_axis',(1.,0.,0.));
#4840=DIRECTION('center_axis',(0.,0.,-1.));
#4841=DIRECTION('ref_axis',(1.,0.,0.));
#4842=DIRECTION('center_axis',(0.,0.,-1.));
#4843=DIRECTION('ref_axis',(1.,0.,0.));
#4844=DIRECTION('',(0.,0.,-1.));
#4845=DIRECTION('center_axis',(0.,0.,1.));
#4846=DIRECTION('ref_axis',(1.,0.,0.));
#4847=DIRECTION('center_axis',(-1.,0.,0.));
#4848=DIRECTION('ref_axis',(0.,0.,1.));
#4849=DIRECTION('',(0.,0.,-1.));
#4850=DIRECTION('',(0.,1.,0.));
#4851=DIRECTION('',(0.,0.,1.));
#4852=DIRECTION('',(0.,1.,0.));
#4853=DIRECTION('center_axis',(0.,0.,-1.));
#4854=DIRECTION('ref_axis',(-1.,0.,0.));
#4855=DIRECTION('',(1.,0.,0.));
#4856=DIRECTION('',(-1.,0.,0.));
#4857=DIRECTION('',(0.,1.,0.));
#4858=DIRECTION('center_axis',(0.496138938356834,0.,0.868243142124459));
#4859=DIRECTION('ref_axis',(0.868243142124459,0.,-0.496138938356834));
#4860=DIRECTION('',(-0.868243142124459,0.,0.496138938356834));
#4861=DIRECTION('',(0.868243142124459,0.,-0.496138938356834));
#4862=DIRECTION('',(0.,1.,0.));
#4863=DIRECTION('center_axis',(0.,0.,1.));
#4864=DIRECTION('ref_axis',(1.,0.,0.));
#4865=DIRECTION('',(-1.,0.,0.));
#4866=DIRECTION('',(1.,0.,0.));
#4867=DIRECTION('center_axis',(0.,1.,0.));
#4868=DIRECTION('ref_axis',(0.,0.,1.));
#4869=DIRECTION('center_axis',(0.,1.,0.));
#4870=DIRECTION('ref_axis',(1.,0.,0.));
#4871=DIRECTION('axis',(0.,0.,1.));
#4872=DIRECTION('refdir',(1.,0.,0.));
#4873=DIRECTION('center_axis',(0.,1.,0.));
#4874=DIRECTION('ref_axis',(0.707106781186546,0.,-0.707106781186549));
#4875=DIRECTION('',(0.,-1.,0.));
#4876=DIRECTION('center_axis',(0.,0.707106781186549,-0.707106781186546));
#4877=DIRECTION('ref_axis',(0.,-0.707106781186546,-0.707106781186549));
#4878=DIRECTION('',(0.,1.,0.));
#4879=DIRECTION('center_axis',(0.,-0.707106781186549,-0.707106781186546));
#4880=DIRECTION('ref_axis',(0.,-0.707106781186546,0.707106781186549));
#4881=DIRECTION('center_axis',(0.,0.,1.));
#4882=DIRECTION('ref_axis',(0.707106781186551,-0.707106781186544,0.));
#4883=DIRECTION('',(0.,0.,-1.));
#4884=DIRECTION('',(0.,0.,1.));
#4885=DIRECTION('center_axis',(0.,-0.707106781186549,-0.707106781186546));
#4886=DIRECTION('ref_axis',(0.,0.707106781186546,-0.707106781186549));
#4887=DIRECTION('center_axis',(0.,0.,1.));
#4888=DIRECTION('ref_axis',(0.707106781186548,0.707106781186548,0.));
#4889=DIRECTION('',(0.,0.,-1.));
#4890=DIRECTION('',(0.,0.,1.));
#4891=DIRECTION('center_axis',(0.,0.707106781186549,-0.707106781186546));
#4892=DIRECTION('ref_axis',(0.,-0.707106781186546,-0.707106781186549));
#4893=DIRECTION('center_axis',(0.,1.,0.));
#4894=DIRECTION('ref_axis',(0.707106781186549,0.,0.707106781186546));
#4895=DIRECTION('',(0.,-1.,0.));
#4896=DIRECTION('',(0.,1.,0.));
#4897=DIRECTION('center_axis',(0.,1.,0.));
#4898=DIRECTION('ref_axis',(-1.,0.,0.));
#4899=DIRECTION('',(-1.,0.,0.));
#4900=DIRECTION('',(0.,0.,1.));
#4901=DIRECTION('',(-1.,0.,0.));
#4902=DIRECTION('center_axis',(0.,0.,1.));
#4903=DIRECTION('ref_axis',(1.,0.,0.));
#4904=DIRECTION('',(1.,0.,0.));
#4905=DIRECTION('',(0.,-1.,0.));
#4906=DIRECTION('center_axis',(1.,0.,0.));
#4907=DIRECTION('ref_axis',(0.,1.,0.));
#4908=DIRECTION('center_axis',(0.,-1.,0.));
#4909=DIRECTION('ref_axis',(1.,0.,0.));
#4910=DIRECTION('',(1.,0.,0.));
#4911=DIRECTION('',(0.,0.,1.));
#4912=DIRECTION('center_axis',(-1.,0.,0.));
#4913=DIRECTION('ref_axis',(0.,-1.,0.));
#4914=DIRECTION('',(0.,-1.,0.));
#4915=DIRECTION('center_axis',(0.,0.,1.));
#4916=DIRECTION('ref_axis',(1.,0.,0.));
#4917=DIRECTION('axis',(0.,0.,1.));
#4918=DIRECTION('refdir',(1.,0.,0.));
#4919=DIRECTION('center_axis',(0.,1.,0.));
#4920=DIRECTION('ref_axis',(-1.,0.,0.));
#4921=DIRECTION('',(-1.,0.,0.));
#4922=DIRECTION('',(0.,0.,1.));
#4923=DIRECTION('',(-1.,0.,0.));
#4924=DIRECTION('',(0.,0.,1.));
#4925=DIRECTION('center_axis',(1.,0.,0.));
#4926=DIRECTION('ref_axis',(0.,1.,0.));
#4927=DIRECTION('',(0.,1.,0.));
#4928=DIRECTION('',(0.,1.,0.));
#4929=DIRECTION('',(0.,0.,1.));
#4930=DIRECTION('center_axis',(0.,-1.,0.));
#4931=DIRECTION('ref_axis',(1.,0.,0.));
#4932=DIRECTION('',(1.,0.,0.));
#4933=DIRECTION('',(1.,0.,0.));
#4934=DIRECTION('',(0.,0.,1.));
#4935=DIRECTION('center_axis',(-1.,0.,0.));
#4936=DIRECTION('ref_axis',(0.,-1.,0.));
#4937=DIRECTION('',(0.,-1.,0.));
#4938=DIRECTION('',(0.,-1.,0.));
#4939=DIRECTION('center_axis',(0.,0.,1.));
#4940=DIRECTION('ref_axis',(1.,0.,0.));
#4941=DIRECTION('center_axis',(0.,0.,1.));
#4942=DIRECTION('ref_axis',(1.,0.,0.));
#4943=DIRECTION('axis',(0.,0.,1.));
#4944=DIRECTION('refdir',(1.,0.,0.));
#4945=DIRECTION('center_axis',(0.,-1.,0.));
#4946=DIRECTION('ref_axis',(0.,0.,1.));
#4947=DIRECTION('center_axis',(0.,-1.,0.));
#4948=DIRECTION('ref_axis',(0.,0.,1.));
#4949=DIRECTION('',(0.,-1.,0.));
#4950=DIRECTION('center_axis',(0.,1.,0.));
#4951=DIRECTION('ref_axis',(0.,0.,1.));
#4952=DIRECTION('center_axis',(0.,0.,1.));
#4953=DIRECTION('ref_axis',(1.,0.,0.));
#4954=DIRECTION('',(-1.,0.,0.));
#4955=DIRECTION('',(0.,1.,0.));
#4956=DIRECTION('',(1.,0.,0.));
#4957=DIRECTION('',(0.,1.,0.));
#4958=DIRECTION('center_axis',(-1.,0.,0.));
#4959=DIRECTION('ref_axis',(0.,0.,1.));
#4960=DIRECTION('',(0.,0.,-1.));
#4961=DIRECTION('',(0.,0.,1.));
#4962=DIRECTION('',(0.,1.,0.));
#4963=DIRECTION('center_axis',(0.,0.,-1.));
#4964=DIRECTION('ref_axis',(-1.,0.,0.));
#4965=DIRECTION('',(1.,0.,0.));
#4966=DIRECTION('',(-1.,0.,0.));
#4967=DIRECTION('',(0.,1.,0.));
#4968=DIRECTION('center_axis',(1.,0.,0.));
#4969=DIRECTION('ref_axis',(0.,0.,-1.));
#4970=DIRECTION('',(0.,0.,1.));
#4971=DIRECTION('',(0.,0.,-1.));
#4972=DIRECTION('',(0.,1.,0.));
#4973=DIRECTION('center_axis',(0.,1.,0.));
#4974=DIRECTION('ref_axis',(3.70074341541719E-16,0.,1.));
#4975=DIRECTION('center_axis',(0.,1.,0.));
#4976=DIRECTION('ref_axis',(3.70074341541719E-16,0.,1.));
#4977=DIRECTION('center_axis',(0.,1.,0.));
#4978=DIRECTION('ref_axis',(3.70074341541719E-16,0.,1.));
#4979=DIRECTION('center_axis',(0.,1.,0.));
#4980=DIRECTION('ref_axis',(1.,0.,0.));
#4981=DIRECTION('center_axis',(0.,1.,0.));
#4982=DIRECTION('ref_axis',(1.,0.,0.));
#4983=DIRECTION('axis',(0.,0.,1.));
#4984=DIRECTION('refdir',(1.,0.,0.));
#4985=DIRECTION('center_axis',(0.,0.,1.));
#4986=DIRECTION('ref_axis',(-0.608992685579745,0.793175837321315,0.));
#4987=DIRECTION('',(0.,0.,1.));
#4988=DIRECTION('center_axis',(0.,0.,-1.));
#4989=DIRECTION('ref_axis',(1.,6.25384645961333E-14,0.));
#4990=DIRECTION('center_axis',(0.,0.,1.));
#4991=DIRECTION('ref_axis',(-0.608992685579745,0.793175837321315,0.));
#4992=DIRECTION('',(0.,0.,1.));
#4993=DIRECTION('center_axis',(0.,0.,1.));
#4994=DIRECTION('ref_axis',(-0.608992685579745,0.793175837321315,0.));
#4995=DIRECTION('',(0.,0.,1.));
#4996=DIRECTION('center_axis',(0.,0.,1.));
#4997=DIRECTION('ref_axis',(-0.608992685579745,0.793175837321315,0.));
#4998=DIRECTION('',(0.,0.,1.));
#4999=DIRECTION('center_axis',(0.,0.,1.));
#5000=DIRECTION('ref_axis',(-0.608992685579745,0.793175837321315,0.));
#5001=DIRECTION('',(0.,0.,1.));
#5002=DIRECTION('center_axis',(0.,0.,1.));
#5003=DIRECTION('ref_axis',(-0.608992685579745,0.793175837321315,0.));
#5004=DIRECTION('',(0.,0.,1.));
#5005=DIRECTION('center_axis',(0.,0.,1.));
#5006=DIRECTION('ref_axis',(-0.608992685579745,0.793175837321315,0.));
#5007=DIRECTION('',(0.,0.,1.));
#5008=DIRECTION('center_axis',(0.,0.,1.));
#5009=DIRECTION('ref_axis',(-0.608992685579745,0.793175837321315,0.));
#5010=DIRECTION('',(0.,0.,1.));
#5011=DIRECTION('center_axis',(0.,0.,1.));
#5012=DIRECTION('ref_axis',(-0.608992685579745,0.793175837321315,0.));
#5013=DIRECTION('',(0.,0.,1.));
#5014=DIRECTION('center_axis',(0.,0.,1.));
#5015=DIRECTION('ref_axis',(-0.608992685579745,0.793175837321315,0.));
#5016=DIRECTION('',(0.,0.,1.));
#5017=DIRECTION('center_axis',(0.,0.,1.));
#5018=DIRECTION('ref_axis',(-0.608992685579745,0.793175837321315,0.));
#5019=DIRECTION('',(0.,0.,1.));
#5020=DIRECTION('center_axis',(0.,0.,1.));
#5021=DIRECTION('ref_axis',(1.,6.25384645961333E-14,0.));
#5022=DIRECTION('center_axis',(0.,0.,1.));
#5023=DIRECTION('ref_axis',(0.835515886164021,-0.549466290110277,0.));
#5024=DIRECTION('',(0.,0.,1.));
#5025=DIRECTION('center_axis',(0.,0.,1.));
#5026=DIRECTION('ref_axis',(1.,0.,0.));
#5027=DIRECTION('center_axis',(0.,0.,1.));
#5028=DIRECTION('ref_axis',(0.835515886164021,-0.549466290110277,0.));
#5029=DIRECTION('',(0.,0.,1.));
#5030=DIRECTION('center_axis',(0.,0.,1.));
#5031=DIRECTION('ref_axis',(0.835515886164021,-0.549466290110277,0.));
#5032=DIRECTION('',(0.,0.,1.));
#5033=DIRECTION('center_axis',(0.,0.,1.));
#5034=DIRECTION('ref_axis',(0.835515886164021,-0.549466290110277,0.));
#5035=DIRECTION('',(0.,0.,1.));
#5036=DIRECTION('center_axis',(0.,0.,1.));
#5037=DIRECTION('ref_axis',(0.835515886164021,-0.549466290110277,0.));
#5038=DIRECTION('',(0.,0.,1.));
#5039=DIRECTION('center_axis',(0.,0.,1.));
#5040=DIRECTION('ref_axis',(0.835515886164021,-0.549466290110277,0.));
#5041=DIRECTION('',(0.,0.,1.));
#5042=DIRECTION('center_axis',(0.,0.,1.));
#5043=DIRECTION('ref_axis',(0.835515886164021,-0.549466290110277,0.));
#5044=DIRECTION('',(0.,0.,1.));
#5045=DIRECTION('center_axis',(0.,0.,1.));
#5046=DIRECTION('ref_axis',(0.835515886164021,-0.549466290110277,0.));
#5047=DIRECTION('',(0.,0.,1.));
#5048=DIRECTION('center_axis',(0.,0.,1.));
#5049=DIRECTION('ref_axis',(0.835515886164021,-0.549466290110277,0.));
#5050=DIRECTION('',(0.,0.,1.));
#5051=DIRECTION('center_axis',(0.,0.,1.));
#5052=DIRECTION('ref_axis',(0.835515886164021,-0.549466290110277,0.));
#5053=DIRECTION('',(0.,0.,1.));
#5054=DIRECTION('center_axis',(0.,0.,1.));
#5055=DIRECTION('ref_axis',(0.835515886164021,-0.549466290110277,0.));
#5056=DIRECTION('',(0.,0.,1.));
#5057=DIRECTION('center_axis',(0.,0.,1.));
#5058=DIRECTION('ref_axis',(1.,0.,0.));
#5059=DIRECTION('center_axis',(0.,0.,1.));
#5060=DIRECTION('ref_axis',(0.835515886164021,-0.549466290110277,0.));
#5061=DIRECTION('center_axis',(0.,0.,1.));
#5062=DIRECTION('ref_axis',(-0.608992685579745,0.793175837321315,0.));
#5063=DIRECTION('center_axis',(0.,0.,1.));
#5064=DIRECTION('ref_axis',(1.,0.,0.));
#5065=DIRECTION('center_axis',(0.,0.,1.));
#5066=DIRECTION('ref_axis',(1.,0.,0.));
#5067=DIRECTION('center_axis',(0.,0.,1.));
#5068=DIRECTION('ref_axis',(1.,0.,0.));
#5069=DIRECTION('',(0.,0.,-1.));
#5070=DIRECTION('center_axis',(0.,0.,1.));
#5071=DIRECTION('ref_axis',(1.,0.,0.));
#5072=DIRECTION('center_axis',(0.,0.,1.));
#5073=DIRECTION('ref_axis',(1.,0.,0.));
#5074=DIRECTION('axis',(0.,0.,1.));
#5075=DIRECTION('refdir',(1.,0.,0.));
#5076=DIRECTION('center_axis',(0.,0.,1.));
#5077=DIRECTION('ref_axis',(1.,0.,0.));
#5078=DIRECTION('center_axis',(0.,0.,-1.));
#5079=DIRECTION('ref_axis',(1.,0.,0.));
#5080=DIRECTION('',(0.,0.,1.));
#5081=DIRECTION('center_axis',(0.,0.,-1.));
#5082=DIRECTION('ref_axis',(1.,0.,0.));
#5083=DIRECTION('center_axis',(0.,0.,1.));
#5084=DIRECTION('ref_axis',(1.,0.,0.));
#5085=DIRECTION('center_axis',(0.,0.,1.));
#5086=DIRECTION('ref_axis',(1.,0.,0.));
#5087=DIRECTION('',(0.,0.,-1.));
#5088=DIRECTION('center_axis',(0.,0.,1.));
#5089=DIRECTION('ref_axis',(1.,0.,0.));
#5090=DIRECTION('center_axis',(0.,0.,1.));
#5091=DIRECTION('ref_axis',(1.,0.,0.));
#5092=DIRECTION('center_axis',(0.,0.,1.));
#5093=DIRECTION('ref_axis',(1.,0.,0.));
#5094=DIRECTION('axis',(0.,0.,1.));
#5095=DIRECTION('refdir',(1.,0.,0.));
#5096=DIRECTION('center_axis',(0.,0.,1.));
#5097=DIRECTION('ref_axis',(1.,0.,0.));
#5098=DIRECTION('',(0.,0.,-1.));
#5099=DIRECTION('center_axis',(0.,0.,-1.));
#5100=DIRECTION('ref_axis',(1.,0.,0.));
#5101=DIRECTION('center_axis',(0.,0.,1.));
#5102=DIRECTION('ref_axis',(1.,0.,0.));
#5103=DIRECTION('',(0.,0.,-1.));
#5104=DIRECTION('center_axis',(0.,0.,1.));
#5105=DIRECTION('ref_axis',(1.,0.,0.));
#5106=DIRECTION('',(0.,0.,-1.));
#5107=DIRECTION('center_axis',(0.,0.,1.));
#5108=DIRECTION('ref_axis',(1.,0.,0.));
#5109=DIRECTION('',(0.,0.,-1.));
#5110=DIRECTION('center_axis',(0.,0.,1.));
#5111=DIRECTION('ref_axis',(1.,0.,0.));
#5112=DIRECTION('',(0.,0.,-1.));
#5113=DIRECTION('center_axis',(0.,0.,1.));
#5114=DIRECTION('ref_axis',(1.,0.,0.));
#5115=DIRECTION('',(0.,0.,-1.));
#5116=DIRECTION('center_axis',(0.,0.,1.));
#5117=DIRECTION('ref_axis',(1.,0.,0.));
#5118=DIRECTION('',(0.,0.,-1.));
#5119=DIRECTION('center_axis',(0.,0.,1.));
#5120=DIRECTION('ref_axis',(1.,0.,0.));
#5121=DIRECTION('',(0.,0.,-1.));
#5122=DIRECTION('center_axis',(0.,0.,1.));
#5123=DIRECTION('ref_axis',(1.,0.,0.));
#5124=DIRECTION('',(0.,0.,-1.));
#5125=DIRECTION('center_axis',(0.,0.,1.));
#5126=DIRECTION('ref_axis',(1.,0.,0.));
#5127=DIRECTION('',(0.,0.,-1.));
#5128=DIRECTION('center_axis',(0.,0.,1.));
#5129=DIRECTION('ref_axis',(1.,0.,0.));
#5130=DIRECTION('',(0.,0.,-1.));
#5131=DIRECTION('center_axis',(0.,0.,1.));
#5132=DIRECTION('ref_axis',(1.,0.,0.));
#5133=DIRECTION('',(0.,0.,-1.));
#5134=DIRECTION('center_axis',(0.,0.,1.));
#5135=DIRECTION('ref_axis',(1.,0.,0.));
#5136=DIRECTION('',(0.,0.,-1.));
#5137=DIRECTION('center_axis',(0.,0.,1.));
#5138=DIRECTION('ref_axis',(1.,0.,0.));
#5139=DIRECTION('',(0.,0.,-1.));
#5140=DIRECTION('center_axis',(0.,0.,1.));
#5141=DIRECTION('ref_axis',(1.,0.,0.));
#5142=DIRECTION('',(0.,0.,-1.));
#5143=DIRECTION('center_axis',(0.,0.,1.));
#5144=DIRECTION('ref_axis',(1.,0.,0.));
#5145=DIRECTION('',(0.,0.,-1.));
#5146=DIRECTION('center_axis',(0.,0.,1.));
#5147=DIRECTION('ref_axis',(1.,0.,0.));
#5148=DIRECTION('',(0.,0.,-1.));
#5149=DIRECTION('center_axis',(0.,0.,1.));
#5150=DIRECTION('ref_axis',(1.,0.,0.));
#5151=DIRECTION('',(0.,0.,-1.));
#5152=DIRECTION('center_axis',(0.,0.,1.));
#5153=DIRECTION('ref_axis',(1.,0.,0.));
#5154=DIRECTION('',(0.,0.,-1.));
#5155=DIRECTION('center_axis',(0.,0.,1.));
#5156=DIRECTION('ref_axis',(1.,0.,0.));
#5157=DIRECTION('',(0.,0.,-1.));
#5158=DIRECTION('center_axis',(0.,0.,1.));
#5159=DIRECTION('ref_axis',(1.,0.,0.));
#5160=DIRECTION('',(0.,0.,-1.));
#5161=DIRECTION('center_axis',(0.,0.,1.));
#5162=DIRECTION('ref_axis',(1.,0.,0.));
#5163=DIRECTION('',(0.,0.,-1.));
#5164=DIRECTION('center_axis',(0.,0.,1.));
#5165=DIRECTION('ref_axis',(1.,0.,0.));
#5166=DIRECTION('',(0.,0.,-1.));
#5167=DIRECTION('center_axis',(0.,0.,1.));
#5168=DIRECTION('ref_axis',(1.,0.,0.));
#5169=DIRECTION('',(0.,0.,-1.));
#5170=DIRECTION('center_axis',(0.,0.,1.));
#5171=DIRECTION('ref_axis',(1.,0.,0.));
#5172=DIRECTION('',(0.,0.,-1.));
#5173=DIRECTION('center_axis',(0.,0.,1.));
#5174=DIRECTION('ref_axis',(1.,0.,0.));
#5175=DIRECTION('',(0.,0.,-1.));
#5176=DIRECTION('center_axis',(0.,0.,1.));
#5177=DIRECTION('ref_axis',(1.,0.,0.));
#5178=DIRECTION('',(0.,0.,-1.));
#5179=DIRECTION('center_axis',(0.,0.,1.));
#5180=DIRECTION('ref_axis',(1.,0.,0.));
#5181=DIRECTION('',(0.,0.,-1.));
#5182=DIRECTION('center_axis',(0.,0.,1.));
#5183=DIRECTION('ref_axis',(0.968644250912352,-0.248451836729877,0.));
#5184=DIRECTION('',(0.,0.,-1.));
#5185=DIRECTION('center_axis',(0.,0.,-1.));
#5186=DIRECTION('ref_axis',(1.,-9.58699708308227E-14,0.));
#5187=DIRECTION('center_axis',(0.,0.,1.));
#5188=DIRECTION('ref_axis',(0.968644250912352,-0.248451836729877,0.));
#5189=DIRECTION('',(0.,0.,-1.));
#5190=DIRECTION('center_axis',(0.,0.,1.));
#5191=DIRECTION('ref_axis',(0.968644250912352,-0.248451836729877,0.));
#5192=DIRECTION('',(0.,0.,-1.));
#5193=DIRECTION('center_axis',(0.,0.,1.));
#5194=DIRECTION('ref_axis',(0.968644250912352,-0.248451836729877,0.));
#5195=DIRECTION('',(0.,0.,-1.));
#5196=DIRECTION('center_axis',(0.,0.,1.));
#5197=DIRECTION('ref_axis',(0.968644250912352,-0.248451836729877,0.));
#5198=DIRECTION('',(0.,0.,-1.));
#5199=DIRECTION('center_axis',(0.,0.,1.));
#5200=DIRECTION('ref_axis',(0.968644250912352,-0.248451836729877,0.));
#5201=DIRECTION('',(0.,0.,-1.));
#5202=DIRECTION('center_axis',(0.,0.,1.));
#5203=DIRECTION('ref_axis',(0.968644250912352,-0.248451836729877,0.));
#5204=DIRECTION('',(0.,0.,-1.));
#5205=DIRECTION('center_axis',(0.,0.,1.));
#5206=DIRECTION('ref_axis',(0.968644250912352,-0.248451836729877,0.));
#5207=DIRECTION('',(0.,0.,-1.));
#5208=DIRECTION('center_axis',(0.,0.,1.));
#5209=DIRECTION('ref_axis',(0.968644250912352,-0.248451836729877,0.));
#5210=DIRECTION('',(0.,0.,-1.));
#5211=DIRECTION('center_axis',(0.,0.,1.));
#5212=DIRECTION('ref_axis',(0.968644250912352,-0.248451836729877,0.));
#5213=DIRECTION('',(0.,0.,-1.));
#5214=DIRECTION('center_axis',(0.,0.,1.));
#5215=DIRECTION('ref_axis',(0.968644250912352,-0.248451836729877,0.));
#5216=DIRECTION('',(0.,0.,-1.));
#5217=DIRECTION('center_axis',(0.,0.,1.));
#5218=DIRECTION('ref_axis',(0.968644250912352,-0.248451836729877,0.));
#5219=DIRECTION('',(0.,0.,-1.));
#5220=DIRECTION('center_axis',(0.,0.,1.));
#5221=DIRECTION('ref_axis',(0.968644250912352,-0.248451836729877,0.));
#5222=DIRECTION('',(0.,0.,-1.));
#5223=DIRECTION('center_axis',(0.,0.,1.));
#5224=DIRECTION('ref_axis',(0.968644250912352,-0.248451836729877,0.));
#5225=DIRECTION('',(0.,0.,-1.));
#5226=DIRECTION('center_axis',(0.,0.,1.));
#5227=DIRECTION('ref_axis',(0.968644250912352,-0.248451836729877,0.));
#5228=DIRECTION('',(0.,0.,-1.));
#5229=DIRECTION('center_axis',(0.,0.,1.));
#5230=DIRECTION('ref_axis',(0.968644250912352,-0.248451836729877,0.));
#5231=DIRECTION('',(0.,0.,-1.));
#5232=DIRECTION('center_axis',(0.,0.,1.));
#5233=DIRECTION('ref_axis',(0.968644250912352,-0.248451836729877,0.));
#5234=DIRECTION('',(0.,0.,-1.));
#5235=DIRECTION('center_axis',(0.,0.,1.));
#5236=DIRECTION('ref_axis',(0.968644250912352,-0.248451836729877,0.));
#5237=DIRECTION('',(0.,0.,-1.));
#5238=DIRECTION('center_axis',(0.,0.,1.));
#5239=DIRECTION('ref_axis',(0.968644250912352,-0.248451836729877,0.));
#5240=DIRECTION('',(0.,0.,-1.));
#5241=DIRECTION('center_axis',(0.,0.,1.));
#5242=DIRECTION('ref_axis',(0.968644250912352,-0.248451836729877,0.));
#5243=DIRECTION('',(0.,0.,-1.));
#5244=DIRECTION('center_axis',(0.,0.,1.));
#5245=DIRECTION('ref_axis',(0.968644250912352,-0.248451836729877,0.));
#5246=DIRECTION('',(0.,0.,-1.));
#5247=DIRECTION('center_axis',(0.,0.,1.));
#5248=DIRECTION('ref_axis',(0.968644250912352,-0.248451836729877,0.));
#5249=DIRECTION('',(0.,0.,-1.));
#5250=DIRECTION('center_axis',(0.,0.,1.));
#5251=DIRECTION('ref_axis',(0.968644250912352,-0.248451836729877,0.));
#5252=DIRECTION('',(0.,0.,-1.));
#5253=DIRECTION('center_axis',(0.,0.,1.));
#5254=DIRECTION('ref_axis',(0.968644250912352,-0.248451836729877,0.));
#5255=DIRECTION('',(0.,0.,-1.));
#5256=DIRECTION('center_axis',(0.,0.,1.));
#5257=DIRECTION('ref_axis',(0.968644250912352,-0.248451836729877,0.));
#5258=DIRECTION('',(0.,0.,-1.));
#5259=DIRECTION('center_axis',(0.,0.,1.));
#5260=DIRECTION('ref_axis',(0.968644250912352,-0.248451836729877,0.));
#5261=DIRECTION('',(0.,0.,-1.));
#5262=DIRECTION('center_axis',(0.,0.,1.));
#5263=DIRECTION('ref_axis',(0.968644250912352,-0.248451836729877,0.));
#5264=DIRECTION('',(0.,0.,-1.));
#5265=DIRECTION('center_axis',(0.,0.,1.));
#5266=DIRECTION('ref_axis',(0.968644250912352,-0.248451836729877,0.));
#5267=DIRECTION('',(0.,0.,-1.));
#5268=DIRECTION('center_axis',(0.,0.,1.));
#5269=DIRECTION('ref_axis',(0.929914003289978,-0.367777033656544,0.));
#5270=DIRECTION('center_axis',(0.,0.,1.));
#5271=DIRECTION('ref_axis',(1.,-9.58699708308227E-14,0.));
#5272=DIRECTION('center_axis',(0.,0.,1.));
#5273=DIRECTION('ref_axis',(1.,0.,0.));
#5274=DIRECTION('center_axis',(0.,0.,-1.));
#5275=DIRECTION('ref_axis',(1.,0.,0.));
#5276=DIRECTION('center_axis',(0.,0.,-1.));
#5277=DIRECTION('ref_axis',(-0.244277982423325,-0.969705247641359,0.));
#5278=DIRECTION('center_axis',(0.,0.,1.));
#5279=DIRECTION('ref_axis',(1.,0.,0.));
#5280=DIRECTION('center_axis',(-2.18604941971849E-13,1.11567293784461E-13,
1.));
#5281=DIRECTION('ref_axis',(-0.547317217186752,-0.836925243836598,-2.62727639485539E-14));
#5282=DIRECTION('center_axis',(-1.76900854822811E-13,-9.65744760848165E-13,
1.));
#5283=DIRECTION('ref_axis',(0.90668614223658,-0.421805926317007,-2.46963309817708E-13));
#5284=DIRECTION('center_axis',(-1.92296268638356E-16,-1.,0.));
#5285=DIRECTION('ref_axis',(1.,-1.92296268638356E-16,0.));
#5286=DIRECTION('',(1.,-1.92296268638356E-16,0.));
#5287=DIRECTION('',(0.,0.,1.));
#5288=DIRECTION('',(1.,-1.92296268638356E-16,0.));
#5289=DIRECTION('',(0.,0.,1.));
#5290=DIRECTION('center_axis',(-0.866025403784439,-0.5,0.));
#5291=DIRECTION('ref_axis',(0.5,-0.866025403784439,0.));
#5292=DIRECTION('',(0.5,-0.866025403784439,0.));
#5293=DIRECTION('',(0.,0.,1.));
#5294=DIRECTION('',(0.5,-0.866025403784439,0.));
#5295=DIRECTION('center_axis',(-0.866025403784439,0.5,0.));
#5296=DIRECTION('ref_axis',(-0.5,-0.866025403784439,0.));
#5297=DIRECTION('',(-0.5,-0.866025403784439,0.));
#5298=DIRECTION('',(0.,0.,1.));
#5299=DIRECTION('',(-0.5,-0.866025403784439,0.));
#5300=DIRECTION('center_axis',(1.92296268638356E-16,1.,0.));
#5301=DIRECTION('ref_axis',(-1.,1.92296268638356E-16,0.));
#5302=DIRECTION('',(-1.,1.92296268638356E-16,0.));
#5303=DIRECTION('',(0.,0.,1.));
#5304=DIRECTION('',(-1.,1.92296268638356E-16,0.));
#5305=DIRECTION('center_axis',(0.866025403784439,0.5,0.));
#5306=DIRECTION('ref_axis',(-0.5,0.866025403784439,0.));
#5307=DIRECTION('',(-0.5,0.866025403784439,0.));
#5308=DIRECTION('',(0.,0.,1.));
#5309=DIRECTION('',(-0.5,0.866025403784439,0.));
#5310=DIRECTION('center_axis',(0.866025403784439,-0.5,0.));
#5311=DIRECTION('ref_axis',(0.5,0.866025403784439,0.));
#5312=DIRECTION('',(0.5,0.866025403784439,0.));
#5313=DIRECTION('',(0.5,0.866025403784439,0.));
#5314=DIRECTION('center_axis',(0.,0.,1.));
#5315=DIRECTION('ref_axis',(1.,0.,0.));
#5316=DIRECTION('center_axis',(0.,0.,1.));
#5317=DIRECTION('ref_axis',(1.,0.,0.));
#5318=DIRECTION('center_axis',(0.,0.,1.));
#5319=DIRECTION('ref_axis',(1.,0.,0.));
#5320=DIRECTION('center_axis',(0.,0.,1.));
#5321=DIRECTION('ref_axis',(1.,0.,0.));
#5322=DIRECTION('',(0.,0.,-1.));
#5323=DIRECTION('center_axis',(0.,0.,1.));
#5324=DIRECTION('ref_axis',(1.,0.,0.));
#5325=DIRECTION('center_axis',(0.,0.,1.));
#5326=DIRECTION('ref_axis',(1.,0.,0.));
#5327=DIRECTION('center_axis',(0.,0.,1.));
#5328=DIRECTION('ref_axis',(1.,0.,0.));
#5329=DIRECTION('axis',(0.,0.,1.));
#5330=DIRECTION('refdir',(1.,0.,0.));
#5331=DIRECTION('center_axis',(0.,1.,0.));
#5332=DIRECTION('ref_axis',(0.707106781186548,0.,-0.707106781186548));
#5333=DIRECTION('center_axis',(0.,-1.,0.));
#5334=DIRECTION('ref_axis',(0.707106781186548,0.,-0.707106781186548));
#5335=DIRECTION('',(0.,-1.,0.));
#5336=DIRECTION('center_axis',(0.,1.,0.));
#5337=DIRECTION('ref_axis',(0.707106781186548,0.,-0.707106781186548));
#5338=DIRECTION('',(0.,1.,0.));
#5339=DIRECTION('center_axis',(0.,0.,-1.));
#5340=DIRECTION('ref_axis',(-1.,0.,0.));
#5341=DIRECTION('',(-1.,0.,0.));
#5342=DIRECTION('',(0.,1.,0.));
#5343=DIRECTION('',(-1.,0.,0.));
#5344=DIRECTION('center_axis',(0.,1.,0.));
#5345=DIRECTION('ref_axis',(1.,0.,0.));
#5346=DIRECTION('',(0.,0.,-1.));
#5347=DIRECTION('center_axis',(0.,1.,0.));
#5348=DIRECTION('ref_axis',(0.78333569292048,0.,0.621598899771221));
#5349=DIRECTION('',(0.973841209741793,0.,-0.227229615606418));
#5350=DIRECTION('center_axis',(0.,1.,0.));
#5351=DIRECTION('ref_axis',(-3.70074341541719E-16,0.,-1.));
#5352=DIRECTION('',(0.,0.,1.));
#5353=DIRECTION('center_axis',(0.,1.,0.));
#5354=DIRECTION('ref_axis',(0.,0.,1.));
#5355=DIRECTION('center_axis',(0.,1.,0.));
#5356=DIRECTION('ref_axis',(0.78333569292048,0.,0.621598899771221));
#5357=DIRECTION('center_axis',(0.,-1.,0.));
#5358=DIRECTION('ref_axis',(0.78333569292048,0.,0.621598899771221));
#5359=DIRECTION('',(0.,-1.,0.));
#5360=DIRECTION('',(0.,1.,0.));
#5361=DIRECTION('center_axis',(0.227229615606418,0.,0.973841209741793));
#5362=DIRECTION('ref_axis',(0.973841209741793,0.,-0.227229615606418));
#5363=DIRECTION('',(0.973841209741793,0.,-0.227229615606418));
#5364=DIRECTION('',(0.,1.,0.));
#5365=DIRECTION('center_axis',(0.,-1.,0.));
#5366=DIRECTION('ref_axis',(0.,0.,1.));
#5367=DIRECTION('center_axis',(0.,-1.,0.));
#5368=DIRECTION('ref_axis',(0.,0.,1.));
#5369=DIRECTION('',(0.,-1.,0.));
#5370=DIRECTION('center_axis',(1.,0.,0.));
#5371=DIRECTION('ref_axis',(0.,0.,-1.));
#5372=DIRECTION('',(0.,0.,-1.));
#5373=DIRECTION('center_axis',(0.,1.,0.));
#5374=DIRECTION('ref_axis',(-3.70074341541719E-16,0.,-1.));
#5375=DIRECTION('center_axis',(0.,1.,0.));
#5376=DIRECTION('ref_axis',(-3.70074341541719E-16,0.,-1.));
#5377=DIRECTION('',(0.,1.,0.));
#5378=DIRECTION('center_axis',(-1.,0.,0.));
#5379=DIRECTION('ref_axis',(0.,0.,1.));
#5380=DIRECTION('',(0.,0.,1.));
#5381=DIRECTION('center_axis',(0.,1.,0.));
#5382=DIRECTION('ref_axis',(1.,0.,0.));
#5383=DIRECTION('axis',(0.,0.,1.));
#5384=DIRECTION('refdir',(1.,0.,0.));
#5385=DIRECTION('center_axis',(0.,1.,0.));
#5386=DIRECTION('ref_axis',(-1.,0.,0.));
#5387=DIRECTION('',(-1.,0.,0.));
#5388=DIRECTION('',(0.,0.,1.));
#5389=DIRECTION('',(-1.,0.,0.));
#5390=DIRECTION('',(0.,0.,1.));
#5391=DIRECTION('center_axis',(1.,0.,0.));
#5392=DIRECTION('ref_axis',(0.,1.,0.));
#5393=DIRECTION('',(0.,1.,0.));
#5394=DIRECTION('',(0.,1.,0.));
#5395=DIRECTION('',(0.,0.,1.));
#5396=DIRECTION('center_axis',(0.,-1.,0.));
#5397=DIRECTION('ref_axis',(1.,0.,0.));
#5398=DIRECTION('',(1.,0.,0.));
#5399=DIRECTION('',(1.,0.,0.));
#5400=DIRECTION('',(0.,0.,1.));
#5401=DIRECTION('center_axis',(-1.,0.,0.));
#5402=DIRECTION('ref_axis',(0.,-1.,0.));
#5403=DIRECTION('',(0.,-1.,0.));
#5404=DIRECTION('',(0.,-1.,0.));
#5405=DIRECTION('center_axis',(0.,0.,1.));
#5406=DIRECTION('ref_axis',(1.,0.,0.));
#5407=DIRECTION('center_axis',(0.,0.,1.));
#5408=DIRECTION('ref_axis',(1.,0.,0.));
#5409=DIRECTION('axis',(0.,0.,1.));
#5410=DIRECTION('refdir',(1.,0.,0.));
#5411=DIRECTION('center_axis',(0.,0.,1.));
#5412=DIRECTION('ref_axis',(1.,0.,0.));
#5413=DIRECTION('center_axis',(0.,0.,-1.));
#5414=DIRECTION('ref_axis',(1.,0.,0.));
#5415=DIRECTION('',(0.,0.,1.));
#5416=DIRECTION('center_axis',(0.,0.,-1.));
#5417=DIRECTION('ref_axis',(1.,0.,0.));
#5418=DIRECTION('center_axis',(0.,0.,1.));
#5419=DIRECTION('ref_axis',(1.,0.,0.));
#5420=DIRECTION('center_axis',(0.,0.,1.));
#5421=DIRECTION('ref_axis',(1.,0.,0.));
#5422=DIRECTION('',(0.,0.,-1.));
#5423=DIRECTION('center_axis',(0.,0.,1.));
#5424=DIRECTION('ref_axis',(1.,0.,0.));
#5425=DIRECTION('center_axis',(0.,0.,1.));
#5426=DIRECTION('ref_axis',(1.,0.,0.));
#5427=DIRECTION('center_axis',(0.,0.,1.));
#5428=DIRECTION('ref_axis',(1.,0.,0.));
#5429=DIRECTION('axis',(0.,0.,1.));
#5430=DIRECTION('refdir',(1.,0.,0.));
#5431=DIRECTION('center_axis',(0.,1.,0.));
#5432=DIRECTION('ref_axis',(-1.,0.,0.));
#5433=DIRECTION('',(-1.,0.,0.));
#5434=DIRECTION('',(0.,0.,1.));
#5435=DIRECTION('',(-1.,0.,0.));
#5436=DIRECTION('',(0.,0.,1.));
#5437=DIRECTION('center_axis',(1.,0.,0.));
#5438=DIRECTION('ref_axis',(0.,1.,0.));
#5439=DIRECTION('',(0.,1.,0.));
#5440=DIRECTION('',(0.,1.,0.));
#5441=DIRECTION('',(0.,0.,1.));
#5442=DIRECTION('center_axis',(0.,-1.,0.));
#5443=DIRECTION('ref_axis',(1.,0.,0.));
#5444=DIRECTION('',(1.,0.,0.));
#5445=DIRECTION('',(1.,0.,0.));
#5446=DIRECTION('',(0.,0.,1.));
#5447=DIRECTION('center_axis',(-1.,0.,0.));
#5448=DIRECTION('ref_axis',(0.,-1.,0.));
#5449=DIRECTION('',(0.,-1.,0.));
#5450=DIRECTION('',(0.,-1.,0.));
#5451=DIRECTION('center_axis',(0.,0.,1.));
#5452=DIRECTION('ref_axis',(1.,0.,0.));
#5453=DIRECTION('center_axis',(0.,0.,1.));
#5454=DIRECTION('ref_axis',(1.,0.,0.));
#5455=DIRECTION('axis',(0.,0.,1.));
#5456=DIRECTION('refdir',(1.,0.,0.));
#5457=DIRECTION('center_axis',(0.,0.,1.));
#5458=DIRECTION('ref_axis',(1.,0.,0.));
#5459=DIRECTION('center_axis',(0.,0.,1.));
#5460=DIRECTION('ref_axis',(1.,0.,0.));
#5461=DIRECTION('',(0.,0.,-1.));
#5462=DIRECTION('center_axis',(0.,0.,1.));
#5463=DIRECTION('ref_axis',(1.,0.,0.));
#5464=DIRECTION('center_axis',(0.,0.,1.));
#5465=DIRECTION('ref_axis',(1.,0.,0.));
#5466=DIRECTION('center_axis',(0.,0.,1.));
#5467=DIRECTION('ref_axis',(1.,0.,0.));
#5468=DIRECTION('axis',(0.,0.,1.));
#5469=DIRECTION('refdir',(1.,0.,0.));
#5470=DIRECTION('center_axis',(0.,0.,1.));
#5471=DIRECTION('ref_axis',(1.,0.,0.));
#5472=DIRECTION('center_axis',(0.,0.,-1.));
#5473=DIRECTION('ref_axis',(1.,0.,0.));
#5474=DIRECTION('center_axis',(0.,0.,1.));
#5475=DIRECTION('ref_axis',(1.,0.,0.));
#5476=DIRECTION('center_axis',(0.,0.,-1.));
#5477=DIRECTION('ref_axis',(1.,0.,0.));
#5478=DIRECTION('center_axis',(0.,0.,1.));
#5479=DIRECTION('ref_axis',(1.,0.,0.));
#5480=DIRECTION('center_axis',(0.,0.,-1.));
#5481=DIRECTION('ref_axis',(1.,0.,0.));
#5482=DIRECTION('',(0.,0.,1.));
#5483=DIRECTION('center_axis',(0.,0.,1.));
#5484=DIRECTION('ref_axis',(1.,0.,0.));
#5485=DIRECTION('',(0.,0.,-1.));
#5486=DIRECTION('center_axis',(0.,0.,-1.));
#5487=DIRECTION('ref_axis',(1.,0.,0.));
#5488=DIRECTION('center_axis',(0.,0.,1.));
#5489=DIRECTION('ref_axis',(1.,0.,0.));
#5490=DIRECTION('axis',(0.,0.,1.));
#5491=DIRECTION('refdir',(1.,0.,0.));
#5492=DIRECTION('center_axis',(0.,0.,1.));
#5493=DIRECTION('ref_axis',(1.,0.,0.));
#5494=DIRECTION('center_axis',(0.,0.,1.));
#5495=DIRECTION('ref_axis',(1.,0.,0.));
#5496=DIRECTION('',(0.,0.,-1.));
#5497=DIRECTION('center_axis',(0.,0.,1.));
#5498=DIRECTION('ref_axis',(1.,0.,0.));
#5499=DIRECTION('center_axis',(0.,0.,-1.));
#5500=DIRECTION('ref_axis',(-1.,0.,0.));
#5501=DIRECTION('center_axis',(0.,0.,-1.));
#5502=DIRECTION('ref_axis',(1.,0.,0.));
#5503=DIRECTION('center_axis',(0.,0.,1.));
#5504=DIRECTION('ref_axis',(1.,0.,0.));
#5505=DIRECTION('center_axis',(0.,0.,1.));
#5506=DIRECTION('ref_axis',(1.,0.,0.));
#5507=DIRECTION('center_axis',(0.,0.,1.));
#5508=DIRECTION('ref_axis',(1.,0.,0.));
#5509=DIRECTION('center_axis',(0.,0.,1.));
#5510=DIRECTION('ref_axis',(1.,0.,0.));
#5511=DIRECTION('',(0.,0.,-1.));
#5512=DIRECTION('center_axis',(0.,0.,1.));
#5513=DIRECTION('ref_axis',(1.,0.,0.));
#5514=DIRECTION('center_axis',(0.,0.,1.));
#5515=DIRECTION('ref_axis',(1.,0.,0.));
#5516=DIRECTION('center_axis',(0.,0.,1.));
#5517=DIRECTION('ref_axis',(1.,0.,0.));
#5518=DIRECTION('center_axis',(0.,0.,1.));
#5519=DIRECTION('ref_axis',(1.,0.,0.));
#5520=DIRECTION('',(0.,0.,-1.));
#5521=DIRECTION('center_axis',(0.,0.,1.));
#5522=DIRECTION('ref_axis',(1.,0.,0.));
#5523=DIRECTION('center_axis',(0.,0.,1.));
#5524=DIRECTION('ref_axis',(1.,0.,0.));
#5525=DIRECTION('center_axis',(0.,0.,1.));
#5526=DIRECTION('ref_axis',(1.,0.,0.));
#5527=DIRECTION('',(0.,0.,-1.));
#5528=DIRECTION('center_axis',(0.,0.,1.));
#5529=DIRECTION('ref_axis',(1.,0.,0.));
#5530=DIRECTION('axis',(0.,0.,1.));
#5531=DIRECTION('refdir',(1.,0.,0.));
#5532=DIRECTION('center_axis',(0.,0.,1.));
#5533=DIRECTION('ref_axis',(1.,0.,0.));
#5534=DIRECTION('center_axis',(0.,0.,-1.));
#5535=DIRECTION('ref_axis',(1.,0.,0.));
#5536=DIRECTION('',(0.,0.,1.));
#5537=DIRECTION('center_axis',(0.,0.,-1.));
#5538=DIRECTION('ref_axis',(1.,0.,0.));
#5539=DIRECTION('center_axis',(0.,0.,1.));
#5540=DIRECTION('ref_axis',(1.,0.,0.));
#5541=DIRECTION('center_axis',(0.,0.,1.));
#5542=DIRECTION('ref_axis',(1.,0.,0.));
#5543=DIRECTION('',(0.,0.,-1.));
#5544=DIRECTION('center_axis',(0.,0.,1.));
#5545=DIRECTION('ref_axis',(1.,0.,0.));
#5546=DIRECTION('center_axis',(0.,0.,1.));
#5547=DIRECTION('ref_axis',(1.,0.,0.));
#5548=DIRECTION('center_axis',(0.,0.,1.));
#5549=DIRECTION('ref_axis',(1.,0.,0.));
#5550=DIRECTION('axis',(0.,0.,1.));
#5551=DIRECTION('refdir',(1.,0.,0.));
#5552=DIRECTION('center_axis',(-1.,0.,0.));
#5553=DIRECTION('ref_axis',(0.,1.,0.));
#5554=DIRECTION('',(0.,0.,1.));
#5555=DIRECTION('',(0.,-1.,0.));
#5556=DIRECTION('',(0.,0.,-1.));
#5557=DIRECTION('',(0.,1.,0.));
#5558=DIRECTION('center_axis',(1.,0.,0.));
#5559=DIRECTION('ref_axis',(0.,-1.,0.));
#5560=DIRECTION('',(0.,0.,-1.));
#5561=DIRECTION('',(0.,-1.,0.));
#5562=DIRECTION('',(0.,0.,1.));
#5563=DIRECTION('',(0.,1.,0.));
#5564=DIRECTION('center_axis',(0.,0.,1.));
#5565=DIRECTION('ref_axis',(1.,0.,0.));
#5566=DIRECTION('center_axis',(0.,0.,1.));
#5567=DIRECTION('ref_axis',(1.,0.,0.));
#5568=DIRECTION('center_axis',(0.,0.,-1.));
#5569=DIRECTION('ref_axis',(1.,0.,0.));
#5570=DIRECTION('center_axis',(0.,0.,1.));
#5571=DIRECTION('ref_axis',(6.12323399573677E-17,-1.,0.));
#5572=DIRECTION('center_axis',(0.,0.,-1.));
#5573=DIRECTION('ref_axis',(1.,0.,0.));
#5574=DIRECTION('center_axis',(0.,0.,1.));
#5575=DIRECTION('ref_axis',(6.12323399573677E-17,-1.,0.));
#5576=DIRECTION('center_axis',(0.,0.,1.));
#5577=DIRECTION('ref_axis',(1.,0.,0.));
#5578=DIRECTION('center_axis',(0.,0.,1.));
#5579=DIRECTION('ref_axis',(1.,0.,0.));
#5580=DIRECTION('',(0.,0.,1.));
#5581=DIRECTION('',(1.,0.,0.));
#5582=DIRECTION('',(0.,0.,1.));
#5583=DIRECTION('',(1.,0.,0.));
#5584=DIRECTION('',(0.,0.,1.));
#5585=DIRECTION('',(1.,0.,0.));
#5586=DIRECTION('',(0.,0.,1.));
#5587=DIRECTION('',(1.,0.,0.));
#5588=DIRECTION('',(0.,0.,1.));
#5589=DIRECTION('',(1.,0.,0.));
#5590=DIRECTION('',(0.,0.,1.));
#5591=DIRECTION('',(1.,0.,0.));
#5592=DIRECTION('',(0.,0.,1.));
#5593=DIRECTION('',(1.,0.,0.));
#5594=DIRECTION('',(-7.00087615379875E-34,-1.22464679914735E-16,-1.));
#5595=DIRECTION('',(-0.766044443118978,0.642787609686539,-7.87187788734196E-17));
#5596=DIRECTION('',(0.,0.,1.));
#5597=DIRECTION('',(1.,0.,0.));
#5598=DIRECTION('',(0.,0.,1.));
#5599=DIRECTION('',(1.,0.,0.));
#5600=DIRECTION('',(0.,0.,1.));
#5601=DIRECTION('',(1.,0.,0.));
#5602=DIRECTION('',(0.,1.,2.22044604925031E-16));
#5603=DIRECTION('',(1.,0.,0.));
#5604=DIRECTION('',(0.,0.,1.));
#5605=DIRECTION('',(1.,0.,0.));
#5606=DIRECTION('',(1.,0.,0.));
#5607=DIRECTION('',(0.,1.,0.));
#5608=DIRECTION('',(1.,0.,0.));
#5609=DIRECTION('',(0.,1.,0.));
#5610=DIRECTION('',(0.,1.,2.22044604925031E-16));
#5611=DIRECTION('',(1.,0.,0.));
#5612=DIRECTION('',(0.,1.,2.22044604925031E-16));
#5613=DIRECTION('',(1.,0.,0.));
#5614=DIRECTION('',(0.,1.,2.22044604925031E-16));
#5615=DIRECTION('',(1.,0.,0.));
#5616=DIRECTION('',(0.,0.,1.));
#5617=DIRECTION('',(1.,0.,0.));
#5618=DIRECTION('',(0.,0.,1.));
#5619=DIRECTION('',(1.,0.,0.));
#5620=DIRECTION('',(0.,0.,1.));
#5621=DIRECTION('',(1.,0.,0.));
#5622=DIRECTION('',(0.,0.,1.));
#5623=DIRECTION('',(1.,0.,0.));
#5624=DIRECTION('',(-7.00087615379875E-34,-1.22464679914735E-16,-1.));
#5625=DIRECTION('',(-0.766044443118978,0.642787609686539,-7.87187788734196E-17));
#5626=DIRECTION('',(0.,0.,1.));
#5627=DIRECTION('',(1.,0.,0.));
#5628=DIRECTION('',(0.,0.,1.));
#5629=DIRECTION('',(1.,0.,0.));
#5630=DIRECTION('',(0.,1.,2.22044604925031E-16));
#5631=DIRECTION('',(1.,0.,0.));
#5632=DIRECTION('',(0.,0.,1.));
#5633=DIRECTION('',(1.,0.,0.));
#5634=DIRECTION('',(1.,0.,0.));
#5635=DIRECTION('',(0.,1.,0.));
#5636=DIRECTION('',(1.,0.,0.));
#5637=DIRECTION('',(0.,1.,0.));
#5638=DIRECTION('',(0.,1.,2.22044604925031E-16));
#5639=DIRECTION('',(1.,0.,0.));
#5640=DIRECTION('',(0.,-1.,0.));
#5641=DIRECTION('',(1.,0.,0.));
#5642=DIRECTION('',(0.,-1.,0.));
#5643=DIRECTION('',(1.,0.,0.));
#5644=DIRECTION('',(0.,-1.,0.));
#5645=DIRECTION('',(1.,0.,0.));
#5646=DIRECTION('',(0.,-1.,0.));
#5647=DIRECTION('',(1.,0.,0.));
#5648=CARTESIAN_POINT('',(0.,0.,0.));
#5649=CARTESIAN_POINT('',(0.,0.,0.));
#5650=CARTESIAN_POINT('Origin',(25.,125.,0.));
#5651=CARTESIAN_POINT('',(25.,135.,10.));
#5652=CARTESIAN_POINT('',(35.,125.,10.));
#5653=CARTESIAN_POINT('Origin',(25.,125.,10.));
#5654=CARTESIAN_POINT('',(35.,125.,-5.));
#5655=CARTESIAN_POINT('',(35.,125.,0.));
#5656=CARTESIAN_POINT('',(25.,135.,-5.));
#5657=CARTESIAN_POINT('Origin',(25.,125.,-5.));
#5658=CARTESIAN_POINT('',(25.,135.,0.));
#5659=CARTESIAN_POINT('Origin',(40.,135.,0.));
#5660=CARTESIAN_POINT('',(-105.,135.,-5.));
#5661=CARTESIAN_POINT('',(2.5,135.,-5.));
#5662=CARTESIAN_POINT('',(-105.,135.,10.));
#5663=CARTESIAN_POINT('',(-105.,135.,0.));
#5664=CARTESIAN_POINT('',(2.5,135.,10.));
#5665=CARTESIAN_POINT('Origin',(-35.,0.,-5.));
#5666=CARTESIAN_POINT('',(35.,-125.,-5.));
#5667=CARTESIAN_POINT('',(35.,-65.,-5.));
#5668=CARTESIAN_POINT('',(25.,-135.,-5.));
#5669=CARTESIAN_POINT('Origin',(25.,-125.,-5.));
#5670=CARTESIAN_POINT('',(-105.,-135.,-5.));
#5671=CARTESIAN_POINT('',(-72.5,-135.,-5.));
#5672=CARTESIAN_POINT('',(-115.,-125.,-5.));
#5673=CARTESIAN_POINT('Origin',(-105.,-125.,-5.));
#5674=CARTESIAN_POINT('',(-115.,125.,-5.));
#5675=CARTESIAN_POINT('',(-115.,65.,-5.));
#5676=CARTESIAN_POINT('Origin',(-105.,125.,-5.));
#5677=CARTESIAN_POINT('',(20.5,-115.,-5.));
#5678=CARTESIAN_POINT('Origin',(25.,-115.,-5.));
#5679=CARTESIAN_POINT('',(-99.5,-115.,-5.));
#5680=CARTESIAN_POINT('Origin',(-95.,-115.,-5.));
#5681=CARTESIAN_POINT('',(-99.5,115.,-5.));
#5682=CARTESIAN_POINT('Origin',(-95.,115.,-5.));
#5683=CARTESIAN_POINT('',(20.5,115.,-5.));
#5684=CARTESIAN_POINT('Origin',(25.,115.,-5.));
#5685=CARTESIAN_POINT('Origin',(-105.,125.,0.));
#5686=CARTESIAN_POINT('',(-115.,125.,10.));
#5687=CARTESIAN_POINT('Origin',(-105.,125.,10.));
#5688=CARTESIAN_POINT('',(-115.,125.,0.));
#5689=CARTESIAN_POINT('Origin',(-115.,130.,0.));
#5690=CARTESIAN_POINT('',(-115.,-125.,10.));
#5691=CARTESIAN_POINT('',(-115.,-125.,0.));
#5692=CARTESIAN_POINT('',(-115.,65.,10.));
#5693=CARTESIAN_POINT('Origin',(-105.,-125.,0.));
#5694=CARTESIAN_POINT('',(-105.,-135.,10.));
#5695=CARTESIAN_POINT('Origin',(-105.,-125.,10.));
#5696=CARTESIAN_POINT('',(-105.,-135.,0.));
#5697=CARTESIAN_POINT('Origin',(-110.,-135.,0.));
#5698=CARTESIAN_POINT('',(25.,-135.,10.));
#5699=CARTESIAN_POINT('',(25.,-135.,0.));
#5700=CARTESIAN_POINT('',(-72.5,-135.,10.));
#5701=CARTESIAN_POINT('Origin',(25.,-125.,0.));
#5702=CARTESIAN_POINT('',(35.,-125.,10.));
#5703=CARTESIAN_POINT('Origin',(25.,-125.,10.));
#5704=CARTESIAN_POINT('',(35.,-125.,0.));
#5705=CARTESIAN_POINT('Origin',(25.,-115.,5.));
#5706=CARTESIAN_POINT('',(20.5,-115.,10.));
#5707=CARTESIAN_POINT('Origin',(25.,-115.,10.));
#5708=CARTESIAN_POINT('',(20.5,-115.,5.));
#5709=CARTESIAN_POINT('Origin',(-95.,-115.,5.));
#5710=CARTESIAN_POINT('',(-99.5,-115.,10.));
#5711=CARTESIAN_POINT('Origin',(-95.,-115.,10.));
#5712=CARTESIAN_POINT('',(-99.5,-115.,5.));
#5713=CARTESIAN_POINT('Origin',(-95.,115.,5.));
#5714=CARTESIAN_POINT('',(-99.5,115.,10.));
#5715=CARTESIAN_POINT('Origin',(-95.,115.,10.));
#5716=CARTESIAN_POINT('',(-99.5,115.,5.));
#5717=CARTESIAN_POINT('Origin',(25.,115.,5.));
#5718=CARTESIAN_POINT('',(20.5,115.,10.));
#5719=CARTESIAN_POINT('Origin',(25.,115.,10.));
#5720=CARTESIAN_POINT('',(20.5,115.,5.));
#5721=CARTESIAN_POINT('Origin',(35.,-130.,0.));
#5722=CARTESIAN_POINT('',(35.,-65.,10.));
#5723=CARTESIAN_POINT('Origin',(-35.,0.,10.));
#5724=CARTESIAN_POINT('',(0.,0.,0.));
#5725=CARTESIAN_POINT('Origin',(-60.,-75.,35.));
#5726=CARTESIAN_POINT('',(-66.5,-75.,40.));
#5727=CARTESIAN_POINT('Origin',(-60.,-75.,40.));
#5728=CARTESIAN_POINT('',(-66.5,-75.,30.));
#5729=CARTESIAN_POINT('',(-66.5,-75.,35.));
#5730=CARTESIAN_POINT('Origin',(-60.,-75.,30.));
#5731=CARTESIAN_POINT('Origin',(-60.,75.,35.));
#5732=CARTESIAN_POINT('',(-66.5,75.,40.));
#5733=CARTESIAN_POINT('Origin',(-60.,75.,40.));
#5734=CARTESIAN_POINT('',(-66.5,75.,30.));
#5735=CARTESIAN_POINT('',(-66.5,75.,35.));
#5736=CARTESIAN_POINT('Origin',(-60.,75.,30.));
#5737=CARTESIAN_POINT('Origin',(0.,100.,30.));
#5738=CARTESIAN_POINT('',(0.,100.,30.));
#5739=CARTESIAN_POINT('',(-100.,100.,30.));
#5740=CARTESIAN_POINT('',(0.,100.,30.));
#5741=CARTESIAN_POINT('',(-100.,100.,40.));
#5742=CARTESIAN_POINT('',(-100.,100.,30.));
#5743=CARTESIAN_POINT('',(0.,100.,40.));
#5744=CARTESIAN_POINT('',(0.,100.,40.));
#5745=CARTESIAN_POINT('',(0.,100.,30.));
#5746=CARTESIAN_POINT('Origin',(0.,-100.,30.));
#5747=CARTESIAN_POINT('',(0.,-100.,30.));
#5748=CARTESIAN_POINT('',(0.,-100.,30.));
#5749=CARTESIAN_POINT('',(0.,-100.,40.));
#5750=CARTESIAN_POINT('',(0.,-100.,40.));
#5751=CARTESIAN_POINT('',(0.,-100.,30.));
#5752=CARTESIAN_POINT('Origin',(-100.,-100.,30.));
#5753=CARTESIAN_POINT('',(-100.,-100.,30.));
#5754=CARTESIAN_POINT('',(-100.,-100.,30.));
#5755=CARTESIAN_POINT('',(-100.,-100.,40.));
#5756=CARTESIAN_POINT('',(-100.,-100.,40.));
#5757=CARTESIAN_POINT('',(-100.,-100.,30.));
#5758=CARTESIAN_POINT('Origin',(-100.,100.,30.));
#5759=CARTESIAN_POINT('',(-100.,100.,30.));
#5760=CARTESIAN_POINT('',(-100.,100.,40.));
#5761=CARTESIAN_POINT('Origin',(-50.,0.,40.));
#5762=CARTESIAN_POINT('Origin',(-50.,0.,30.));
#5763=CARTESIAN_POINT('',(0.,0.,0.));
#5764=CARTESIAN_POINT('Origin',(-60.,25.,52.));
#5765=CARTESIAN_POINT('',(-66.5,25.,62.));
#5766=CARTESIAN_POINT('Origin',(-60.,25.,62.));
#5767=CARTESIAN_POINT('',(-66.5,25.,42.));
#5768=CARTESIAN_POINT('',(-66.5,25.,52.));
#5769=CARTESIAN_POINT('Origin',(-60.,25.,42.));
#5770=CARTESIAN_POINT('Origin',(-60.,175.,52.));
#5771=CARTESIAN_POINT('',(-66.5,175.,62.));
#5772=CARTESIAN_POINT('Origin',(-60.,175.,62.));
#5773=CARTESIAN_POINT('',(-66.5,175.,42.));
#5774=CARTESIAN_POINT('',(-66.5,175.,52.));
#5775=CARTESIAN_POINT('Origin',(-60.,175.,42.));
#5776=CARTESIAN_POINT('Origin',(-100.,0.,42.));
#5777=CARTESIAN_POINT('',(-100.,0.,62.));
#5778=CARTESIAN_POINT('',(-100.,0.,42.));
#5779=CARTESIAN_POINT('',(-100.,0.,62.));
#5780=CARTESIAN_POINT('',(-100.,200.,62.));
#5781=CARTESIAN_POINT('',(-100.,0.,62.));
#5782=CARTESIAN_POINT('',(-100.,200.,42.));
#5783=CARTESIAN_POINT('',(-100.,200.,62.));
#5784=CARTESIAN_POINT('',(-100.,0.,42.));
#5785=CARTESIAN_POINT('Origin',(-0.999999999999996,0.,42.));
#5786=CARTESIAN_POINT('',(-1.,0.,42.));
#5787=CARTESIAN_POINT('',(-100.,0.,42.));
#5788=CARTESIAN_POINT('',(-1.,200.,42.));
#5789=CARTESIAN_POINT('',(-100.,200.,42.));
#5790=CARTESIAN_POINT('',(-1.,0.,42.));
#5791=CARTESIAN_POINT('Origin',(-36.,0.,62.));
#5792=CARTESIAN_POINT('',(-36.,0.,62.));
#5793=CARTESIAN_POINT('',(-1.,0.,42.));
#5794=CARTESIAN_POINT('',(-36.,200.,62.));
#5795=CARTESIAN_POINT('',(-1.,200.,42.));
#5796=CARTESIAN_POINT('',(-36.,0.,62.));
#5797=CARTESIAN_POINT('Origin',(-100.,0.,62.));
#5798=CARTESIAN_POINT('',(-36.,0.,62.));
#5799=CARTESIAN_POINT('',(-36.,200.,62.));
#5800=CARTESIAN_POINT('Origin',(-50.5,200.,52.));
#5801=CARTESIAN_POINT('Origin',(-50.5,0.,52.));
#5802=CARTESIAN_POINT('',(0.,0.,0.));
#5803=CARTESIAN_POINT('Origin',(78.,-50.,32.));
#5804=CARTESIAN_POINT('',(80.,98.,32.));
#5805=CARTESIAN_POINT('',(80.,-98.,32.));
#5806=CARTESIAN_POINT('',(80.,-50.,32.));
#5807=CARTESIAN_POINT('',(78.,-100.,30.));
#5808=CARTESIAN_POINT('Origin',(78.,-98.,32.));
#5809=CARTESIAN_POINT('',(78.,100.,30.));
#5810=CARTESIAN_POINT('',(78.,-50.,30.));
#5811=CARTESIAN_POINT('Origin',(78.,98.,32.));
#5812=CARTESIAN_POINT('Origin',(78.,-98.,30.));
#5813=CARTESIAN_POINT('',(78.,-100.,40.));
#5814=CARTESIAN_POINT('',(78.,-100.,30.));
#5815=CARTESIAN_POINT('',(80.,-98.,38.));
#5816=CARTESIAN_POINT('',(80.,-98.,30.));
#5817=CARTESIAN_POINT('Origin',(78.,-98.,38.));
#5818=CARTESIAN_POINT('Origin',(78.,98.,30.));
#5819=CARTESIAN_POINT('',(80.,98.,38.));
#5820=CARTESIAN_POINT('',(80.,98.,30.));
#5821=CARTESIAN_POINT('',(78.,100.,40.));
#5822=CARTESIAN_POINT('',(78.,100.,30.));
#5823=CARTESIAN_POINT('Origin',(78.,98.,38.));
#5824=CARTESIAN_POINT('Origin',(78.,-50.,38.));
#5825=CARTESIAN_POINT('',(78.,-50.,40.));
#5826=CARTESIAN_POINT('',(80.,-50.,38.));
#5827=CARTESIAN_POINT('Origin',(80.,100.,30.));
#5828=CARTESIAN_POINT('',(0.,100.,30.));
#5829=CARTESIAN_POINT('',(80.,100.,30.));
#5830=CARTESIAN_POINT('',(0.,100.,40.));
#5831=CARTESIAN_POINT('',(0.,100.,30.));
#5832=CARTESIAN_POINT('',(80.,100.,40.));
#5833=CARTESIAN_POINT('Origin',(40.,0.,30.));
#5834=CARTESIAN_POINT('',(0.,-100.,30.));
#5835=CARTESIAN_POINT('',(0.,-100.,30.));
#5836=CARTESIAN_POINT('',(0.,100.,30.));
#5837=CARTESIAN_POINT('Origin',(80.,-100.,30.));
#5838=CARTESIAN_POINT('Origin',(0.,-100.,30.));
#5839=CARTESIAN_POINT('',(0.,-100.,40.));
#5840=CARTESIAN_POINT('',(0.,-100.,40.));
#5841=CARTESIAN_POINT('',(0.,-100.,30.));
#5842=CARTESIAN_POINT('Origin',(0.,100.,30.));
#5843=CARTESIAN_POINT('',(0.,100.,40.));
#5844=CARTESIAN_POINT('Origin',(40.,0.,40.));
#5845=CARTESIAN_POINT('',(0.,0.,0.));
#5846=CARTESIAN_POINT('Origin',(-10.,10.,10.));
#5847=CARTESIAN_POINT('',(-10.,10.,10.));
#5848=CARTESIAN_POINT('',(-90.,10.,10.));
#5849=CARTESIAN_POINT('',(-10.,10.,10.));
#5850=CARTESIAN_POINT('',(-90.,10.,30.));
#5851=CARTESIAN_POINT('',(-90.,10.,10.));
#5852=CARTESIAN_POINT('',(-10.,10.,30.));
#5853=CARTESIAN_POINT('',(-10.,10.,30.));
#5854=CARTESIAN_POINT('',(-10.,10.,10.));
#5855=CARTESIAN_POINT('Origin',(-10.,-10.,10.));
#5856=CARTESIAN_POINT('',(-10.,-10.,10.));
#5857=CARTESIAN_POINT('',(-10.,-10.,10.));
#5858=CARTESIAN_POINT('',(-10.,-10.,30.));
#5859=CARTESIAN_POINT('',(-10.,-10.,30.));
#5860=CARTESIAN_POINT('',(-10.,-10.,10.));
#5861=CARTESIAN_POINT('Origin',(-90.,-10.,10.));
#5862=CARTESIAN_POINT('',(-90.,-10.,10.));
#5863=CARTESIAN_POINT('',(-90.,-10.,10.));
#5864=CARTESIAN_POINT('',(-90.,-10.,30.));
#5865=CARTESIAN_POINT('',(-90.,-10.,30.));
#5866=CARTESIAN_POINT('',(-90.,-10.,10.));
#5867=CARTESIAN_POINT('Origin',(-90.,10.,10.));
#5868=CARTESIAN_POINT('',(-90.,10.,10.));
#5869=CARTESIAN_POINT('',(-90.,10.,30.));
#5870=CARTESIAN_POINT('Origin',(-50.,0.,30.));
#5871=CARTESIAN_POINT('Origin',(-50.,0.,10.));
#5872=CARTESIAN_POINT('',(0.,0.,0.));
#5873=CARTESIAN_POINT('Origin',(0.,5.,42.));
#5874=CARTESIAN_POINT('',(7.34788079488412E-16,10.,36.));
#5875=CARTESIAN_POINT('Origin',(0.,10.,42.));
#5876=CARTESIAN_POINT('',(7.34788079488412E-16,0.,36.));
#5877=CARTESIAN_POINT('',(7.34788079488412E-16,5.,36.));
#5878=CARTESIAN_POINT('Origin',(0.,0.,42.));
#5879=CARTESIAN_POINT('Origin',(-60.,0.,54.));
#5880=CARTESIAN_POINT('',(0.,0.,54.));
#5881=CARTESIAN_POINT('',(-60.,0.,54.));
#5882=CARTESIAN_POINT('',(0.,0.,54.));
#5883=CARTESIAN_POINT('',(0.,10.,54.));
#5884=CARTESIAN_POINT('',(0.,0.,54.));
#5885=CARTESIAN_POINT('',(-60.,10.,54.));
#5886=CARTESIAN_POINT('',(0.,10.,54.));
#5887=CARTESIAN_POINT('',(-60.,0.,54.));
#5888=CARTESIAN_POINT('Origin',(-60.,0.,10.));
#5889=CARTESIAN_POINT('',(-60.,0.,10.));
#5890=CARTESIAN_POINT('',(-60.,0.,54.));
#5891=CARTESIAN_POINT('',(-60.,10.,10.));
#5892=CARTESIAN_POINT('',(-60.,10.,54.));
#5893=CARTESIAN_POINT('',(-60.,0.,10.));
#5894=CARTESIAN_POINT('Origin',(0.,0.,10.));
#5895=CARTESIAN_POINT('',(0.,0.,10.));
#5896=CARTESIAN_POINT('',(-60.,0.,10.));
#5897=CARTESIAN_POINT('',(0.,10.,10.));
#5898=CARTESIAN_POINT('',(-60.,10.,10.));
#5899=CARTESIAN_POINT('',(0.,0.,10.));
#5900=CARTESIAN_POINT('Origin',(0.,0.,30.));
#5901=CARTESIAN_POINT('',(-7.41220803802443E-15,0.,30.));
#5902=CARTESIAN_POINT('',(0.,0.,10.));
#5903=CARTESIAN_POINT('',(-7.41220803802443E-15,10.,30.));
#5904=CARTESIAN_POINT('',(0.,10.,10.));
#5905=CARTESIAN_POINT('',(-7.41220803802443E-15,0.,30.));
#5906=CARTESIAN_POINT('Origin',(-4.44089209850063E-15,0.,42.));
#5907=CARTESIAN_POINT('Origin',(-4.44089209850063E-15,0.,42.));
#5908=CARTESIAN_POINT('Origin',(-4.44089209850063E-15,10.,42.));
#5909=CARTESIAN_POINT('Origin',(-24.,10.,32.));
#5910=CARTESIAN_POINT('Origin',(-24.,0.,32.));
#5911=CARTESIAN_POINT('',(0.,0.,0.));
#5912=CARTESIAN_POINT('Origin',(0.,0.,-3.86474103256053));
#5913=CARTESIAN_POINT('',(3.72323265631142,-4.84928321986684,18.4846156531836));
#5914=CARTESIAN_POINT('',(3.72309647396852,-4.84910580413568,18.6301376785985));
#5915=CARTESIAN_POINT('',(3.72292453512038,-4.84888218750453,-3.86474103256053));
#5916=CARTESIAN_POINT('',(-6.11311691712474,0.000135883258949067,19.7602589674395));
#5917=CARTESIAN_POINT('Ctrl Pts',(3.72309647396852,-4.84910580413568,18.6301376785985));
#5918=CARTESIAN_POINT('Ctrl Pts',(4.41515761247881,-4.31670063397706,18.6699250225774));
#5919=CARTESIAN_POINT('Ctrl Pts',(5.66534840628249,-2.84103380498307,18.7560271920921));
#5920=CARTESIAN_POINT('Ctrl Pts',(6.37224631075142,0.0728805235909378,18.8884441871425));
#5921=CARTESIAN_POINT('Ctrl Pts',(5.56076804884914,3.1126581338182,19.0273886637497));
#5922=CARTESIAN_POINT('Ctrl Pts',(3.39386814118494,5.39375839285986,19.1663331403569));
#5923=CARTESIAN_POINT('Ctrl Pts',(0.399713947821312,6.3600905721262,19.3052776169641));
#5924=CARTESIAN_POINT('Ctrl Pts',(-2.69185701515731,5.77626560449043,19.4442220935712));
#5925=CARTESIAN_POINT('Ctrl Pts',(-5.12731864093646,3.78429047467954,19.5831665701784));
#5926=CARTESIAN_POINT('Ctrl Pts',(-6.02625257748595,1.57494231132565,19.6885121948012));
#5927=CARTESIAN_POINT('Ctrl Pts',(-6.11338345835182,0.279275489936728,19.7475429938882));
#5928=CARTESIAN_POINT('Ctrl Pts',(-6.11311691712474,0.000135883258949067,
19.7602589674395));
#5929=CARTESIAN_POINT('',(-3.98497178445977,-4.63592767842203,20.));
#5930=CARTESIAN_POINT('Ctrl Pts',(-6.11311691712474,0.000135883258949067,
19.7602589674395));
#5931=CARTESIAN_POINT('Ctrl Pts',(-6.11241264708201,-0.73742229818409,19.7938578194239));
#5932=CARTESIAN_POINT('Ctrl Pts',(-5.79464560539175,-2.49228840649804,19.8737714969441));
#5933=CARTESIAN_POINT('Ctrl Pts',(-4.7558725986553,-3.97327325275336,19.9536851744643));
#5934=CARTESIAN_POINT('Ctrl Pts',(-3.98497178445977,-4.63592767842204,20.));
#5935=CARTESIAN_POINT('',(-1.13987236463957,-6.00604000609645,20.));
#5936=CARTESIAN_POINT('Origin',(0.,0.,20.));
#5937=CARTESIAN_POINT('',(-6.11324999831214,0.000143654567398843,19.6147410325606));
#5938=CARTESIAN_POINT('Ctrl Pts',(-6.11324999831214,0.000143654567399398,
19.6147410325606));
#5939=CARTESIAN_POINT('Ctrl Pts',(-6.11325396531437,-0.168672950627852,
19.622433450954));
#5940=CARTESIAN_POINT('Ctrl Pts',(-6.10626081651799,-0.337517076952744,
19.6301258693473));
#5941=CARTESIAN_POINT('Ctrl Pts',(-6.09228978312654,-0.505797153918474,
19.6378182877407));
#5942=CARTESIAN_POINT('Ctrl Pts',(-6.07831886348921,-0.674075860724036,
19.6455106435012));
#5943=CARTESIAN_POINT('Ctrl Pts',(-6.05737019381285,-0.841790205929373,
19.6532029992618));
#5944=CARTESIAN_POINT('Ctrl Pts',(-6.02951500037806,-1.0083523306444,19.6608953550224));
#5945=CARTESIAN_POINT('Ctrl Pts',(-6.0016621563273,-1.17490040704931,19.6685870619885));
#5946=CARTESIAN_POINT('Ctrl Pts',(-5.96690400636522,-1.34029613956119,19.6762787689545));
#5947=CARTESIAN_POINT('Ctrl Pts',(-5.9253631909807,-1.50396031113559,19.6839704759205));
#5948=CARTESIAN_POINT('Ctrl Pts',(-5.88381107602692,-1.66766900120639,19.6916642751174));
#5949=CARTESIAN_POINT('Ctrl Pts',(-5.8354726859269,-1.82964487612697,19.6993580743143));
#5950=CARTESIAN_POINT('Ctrl Pts',(-5.78052122573528,-1.98932147259408,19.7070518735112));
#5951=CARTESIAN_POINT('Ctrl Pts',(-5.72561165011813,-2.14887636189871,19.7147398084143));
#5952=CARTESIAN_POINT('Ctrl Pts',(-5.66409920055024,-2.30613517773545,19.7224277433174));
#5953=CARTESIAN_POINT('Ctrl Pts',(-5.59620555660258,-2.46055053407776,19.7301156782206));
#5954=CARTESIAN_POINT('Ctrl Pts',(-5.5279872642072,-2.61570426153742,19.7378403746817));
#5955=CARTESIAN_POINT('Ctrl Pts',(-5.4533004837073,-2.76804675380112,19.7455650711429));
#5956=CARTESIAN_POINT('Ctrl Pts',(-5.37240216219969,-2.91703969292365,19.753289767604));
#5957=CARTESIAN_POINT('Ctrl Pts',(-5.29151965130044,-3.0660035131601,19.7610129543658));
#5958=CARTESIAN_POINT('Ctrl Pts',(-5.20442817283899,-3.21161880811471,19.7687361411275));
#5959=CARTESIAN_POINT('Ctrl Pts',(-5.11143070011772,-3.35337170030315,19.7764593278892));
#5960=CARTESIAN_POINT('Ctrl Pts',(-5.01842967837498,-3.49513000214461,19.7841828093875));
#5961=CARTESIAN_POINT('Ctrl Pts',(-4.91952238188278,-3.63302533909178,19.7919062908858));
#5962=CARTESIAN_POINT('Ctrl Pts',(-4.81505563463806,-3.76657202212307,19.7996297723841));
#5963=CARTESIAN_POINT('Ctrl Pts',(-4.71059592941913,-3.90010970287171,19.8073527332482));
#5964=CARTESIAN_POINT('Ctrl Pts',(-4.60057771869083,-4.02929906666183,19.8150756941124));
#5965=CARTESIAN_POINT('Ctrl Pts',(-4.4853888174845,-4.15368664182615,19.8227986549765));
#5966=CARTESIAN_POINT('Ctrl Pts',(-4.37016933986405,-4.27810723515429,19.8305236658685));
#5967=CARTESIAN_POINT('Ctrl Pts',(-4.24977664299735,-4.3977232586767,19.8382486767604));
#5968=CARTESIAN_POINT('Ctrl Pts',(-4.12463684300107,-4.51211662923934,19.8459736876524));
#5969=CARTESIAN_POINT('Ctrl Pts',(-3.99997527616071,-4.626072835106,19.8536691767108));
#5970=CARTESIAN_POINT('Ctrl Pts',(-3.8706030776783,-4.73484604870215,19.8613646657693));
#5971=CARTESIAN_POINT('Ctrl Pts',(-3.73697560381574,-4.83806148152191,19.8690601548277));
#5972=CARTESIAN_POINT('Ctrl Pts',(-3.60312312372883,-4.94145071179636,19.8767686017974));
#5973=CARTESIAN_POINT('Ctrl Pts',(-3.46495174590424,-5.03930142897327,19.884477048767));
#5974=CARTESIAN_POINT('Ctrl Pts',(-3.32294240358536,-5.13126488742828,19.8921854957366));
#5975=CARTESIAN_POINT('Ctrl Pts',(-3.18096171618241,-5.22320978932126,19.8998923872812));
#5976=CARTESIAN_POINT('Ctrl Pts',(-3.03514487758738,-5.30926962909826,19.9075992788257));
#5977=CARTESIAN_POINT('Ctrl Pts',(-2.88600157662509,-5.38913912069613,19.9153061703702));
#5978=CARTESIAN_POINT('Ctrl Pts',(-2.73685534953163,-5.4690101793011,19.9230132131208));
#5979=CARTESIAN_POINT('Ctrl Pts',(-2.58438280939639,-5.54269049241582,19.9307202558714));
#5980=CARTESIAN_POINT('Ctrl Pts',(-2.42911864174319,-5.60992051519767,19.938427298622));
#5981=CARTESIAN_POINT('Ctrl Pts',(-2.27386281068899,-5.6771469281979,19.9461339275583));
#5982=CARTESIAN_POINT('Ctrl Pts',(-2.11581594560642,-5.7379236174449,19.9538405564947));
#5983=CARTESIAN_POINT('Ctrl Pts',(-1.95553330485704,-5.79203893772262,19.961547185431));
#5984=CARTESIAN_POINT('Ctrl Pts',(-1.79521365570525,-5.84616675293765,19.9692555937867));
#5985=CARTESIAN_POINT('Ctrl Pts',(-1.63265750219451,-5.89363002317083,19.9769640021423));
#5986=CARTESIAN_POINT('Ctrl Pts',(-1.46843667238002,-5.93426653443452,19.984672410498));
#5987=CARTESIAN_POINT('Ctrl Pts',(-1.35958975479145,-5.96120074855098,19.9897816069986));
#5988=CARTESIAN_POINT('Ctrl Pts',(-1.25001184602099,-5.98513689007408,19.9948908034993));
#5989=CARTESIAN_POINT('Ctrl Pts',(-1.13987236463957,-6.00604000609645,20.));
#5990=CARTESIAN_POINT('Ctrl Pts',(3.72323265631121,-4.849283219867,18.4846156531836));
#5991=CARTESIAN_POINT('Ctrl Pts',(4.50011870853811,-4.25236686515347,18.5292637239101));
#5992=CARTESIAN_POINT('Ctrl Pts',(5.78590765134228,-2.64892088143011,18.6202266201722));
#5993=CARTESIAN_POINT('Ctrl Pts',(6.35970660055813,0.406155425428676,18.7575043419702));
#5994=CARTESIAN_POINT('Ctrl Pts',(5.39030758885895,3.39932504877934,18.8964488185774));
#5995=CARTESIAN_POINT('Ctrl Pts',(3.10703361081359,5.56391738475428,19.0353932951846));
#5996=CARTESIAN_POINT('Ctrl Pts',(0.0664258911141372,6.37231582181012,19.1743377717918));
#5997=CARTESIAN_POINT('Ctrl Pts',(-2.99037070298137,5.62747898115738,19.313282248399));
#5998=CARTESIAN_POINT('Ctrl Pts',(-5.31827554245858,3.51095143602872,19.4522267250062));
#5999=CARTESIAN_POINT('Ctrl Pts',(-6.06432482748073,1.36134653944802,19.5527129863934));
#6000=CARTESIAN_POINT('Ctrl Pts',(-6.11361696706913,0.1725691056159,19.6068844222448));
#6001=CARTESIAN_POINT('Ctrl Pts',(-6.11344525254193,0.000143659155656239,
19.6147410325606));
#6002=CARTESIAN_POINT('Origin',(0.,0.,-3.86474103256053));
#6003=CARTESIAN_POINT('',(3.72262360719132,-4.84849058816371,16.7346163843233));
#6004=CARTESIAN_POINT('',(3.72292453512041,-4.84888218750451,16.8801307087023));
#6005=CARTESIAN_POINT('',(3.72292453512038,-4.84888218750453,-3.86474103256053));
#6006=CARTESIAN_POINT('',(-6.11324999839426,-0.000140116351456561,18.0102589674395));
#6007=CARTESIAN_POINT('Ctrl Pts',(3.72292453512041,-4.84888218750451,16.8801307087023));
#6008=CARTESIAN_POINT('Ctrl Pts',(3.85740053234976,-4.74563282608259,16.8878537136735));
#6009=CARTESIAN_POINT('Ctrl Pts',(3.98757637825864,-4.63678758882545,16.8955767186447));
#6010=CARTESIAN_POINT('Ctrl Pts',(4.1129955847594,-4.52273068867136,16.9032997236158));
#6011=CARTESIAN_POINT('Ctrl Pts',(4.23844518939046,-4.40864614429426,16.9110246004288));
#6012=CARTESIAN_POINT('Ctrl Pts',(4.3591356159556,-4.28934762584183,16.9187494772418));
#6013=CARTESIAN_POINT('Ctrl Pts',(4.47464552596157,-4.16525785270158,16.9264743540547));
#6014=CARTESIAN_POINT('Ctrl Pts',(4.55811883171226,-4.07558430371053,16.9320567409171));
#6015=CARTESIAN_POINT('Ctrl Pts',(4.63888747862407,-3.98340945604354,16.9376391277795));
#6016=CARTESIAN_POINT('Ctrl Pts',(4.71680498577818,-3.88890425295329,16.9432215146419));
#6017=CARTESIAN_POINT('Ctrl Pts',(4.82462521105301,-3.75813040431511,16.9509462767789));
#6018=CARTESIAN_POINT('Ctrl Pts',(4.92702260263085,-3.62284664644924,16.9586710389159));
#6019=CARTESIAN_POINT('Ctrl Pts',(5.02363219797993,-3.48352481000486,16.966395801053));
#6020=CARTESIAN_POINT('Ctrl Pts',(5.12022294781536,-3.34423015089788,16.9741190563302));
#6021=CARTESIAN_POINT('Ctrl Pts',(5.2110279737326,-3.20089924524164,16.9818423116075));
#6022=CARTESIAN_POINT('Ctrl Pts',(5.29572486081124,-3.05403401439567,16.9895655668848));
#6023=CARTESIAN_POINT('Ctrl Pts',(5.38042502101611,-2.9071631079168,16.9972891206286));
#6024=CARTESIAN_POINT('Ctrl Pts',(5.45901640827553,-2.75675787549156,17.0050126743725));
#6025=CARTESIAN_POINT('Ctrl Pts',(5.53122152199489,-2.60334669936998,17.0127362281163));
#6026=CARTESIAN_POINT('Ctrl Pts',(5.60342178608984,-2.44994582704192,17.0204592631111));
#6027=CARTESIAN_POINT('Ctrl Pts',(5.66923650003499,-2.29353970182158,17.0281822981059));
#6028=CARTESIAN_POINT('Ctrl Pts',(5.72843538734755,-2.13467879913685,17.0359053331007));
#6029=CARTESIAN_POINT('Ctrl Pts',(5.78765000714097,-1.97577567815672,17.0436304205412));
#6030=CARTESIAN_POINT('Ctrl Pts',(5.84024517420761,-1.81441677253815,17.0513555079816));
#6031=CARTESIAN_POINT('Ctrl Pts',(5.8860394562852,-1.65117082143364,17.0590805954221));
#6032=CARTESIAN_POINT('Ctrl Pts',(5.93165616231051,-1.48855788760185,17.0667757273644));
#6033=CARTESIAN_POINT('Ctrl Pts',(5.97052457975955,-1.32407282631843,17.0744708593068));
#6034=CARTESIAN_POINT('Ctrl Pts',(6.0025151204945,-1.15829089210565,17.0821659912491));
#6035=CARTESIAN_POINT('Ctrl Pts',(6.03462884078278,-0.991870614678331,17.0898907532913));
#6036=CARTESIAN_POINT('Ctrl Pts',(6.05982295693695,-0.824084510481028,17.0976155153334));
#6037=CARTESIAN_POINT('Ctrl Pts',(6.07800272341131,-0.655521515058598,17.1053402773756));
#6038=CARTESIAN_POINT('Ctrl Pts',(6.09617894358047,-0.486991401017124,17.1130635325577));
#6039=CARTESIAN_POINT('Ctrl Pts',(6.10734351031671,-0.317685013049303,17.1207867877398));
#6040=CARTESIAN_POINT('Ctrl Pts',(6.11145343651841,-0.148197354116924,17.1285100429219));
#6041=CARTESIAN_POINT('Ctrl Pts',(6.11556352154921,0.0212968547069763,17.1362335965711));
#6042=CARTESIAN_POINT('Ctrl Pts',(6.11261840885681,0.190972031784622,17.1439571502203));
#6043=CARTESIAN_POINT('Ctrl Pts',(6.10262721144545,0.360231426482325,17.1516807038694));
#6044=CARTESIAN_POINT('Ctrl Pts',(6.0926366850879,0.529479452956983,17.15940373877));
#6045=CARTESIAN_POINT('Ctrl Pts',(6.07560103973935,0.698311436529602,17.1671267736705));
#6046=CARTESIAN_POINT('Ctrl Pts',(6.05158142715187,0.866133819366549,17.1748498085711));
#6047=CARTESIAN_POINT('Ctrl Pts',(6.0275554311944,1.03400080210532,17.1825748959189));
#6048=CARTESIAN_POINT('Ctrl Pts',(5.99654180196561,1.20085733370429,17.1902999832667));
#6049=CARTESIAN_POINT('Ctrl Pts',(5.95865332050269,1.36611718698005,17.1980250706146));
#6050=CARTESIAN_POINT('Ctrl Pts',(5.92091175607884,1.5307362257554,17.2057202030285));
#6051=CARTESIAN_POINT('Ctrl Pts',(5.87634866192639,1.69377064972148,17.2134153354424));
#6052=CARTESIAN_POINT('Ctrl Pts',(5.82512546194225,1.85465331400023,17.2211104678563));
#6053=CARTESIAN_POINT('Ctrl Pts',(5.77370502927614,2.01615544991232,17.2288352300396));
#6054=CARTESIAN_POINT('Ctrl Pts',(5.71555485987603,2.17554641288183,17.2365599922229));
#6055=CARTESIAN_POINT('Ctrl Pts',(5.65087351920439,2.33226371417442,17.2442847544062));
#6056=CARTESIAN_POINT('Ctrl Pts',(5.58620479584162,2.48895044481747,17.2520080097297));
#6057=CARTESIAN_POINT('Ctrl Pts',(5.51500756418546,2.64296426168065,17.2597312650533));
#6058=CARTESIAN_POINT('Ctrl Pts',(5.43752874296885,2.79376211082612,17.2674545203768));
#6059=CARTESIAN_POINT('Ctrl Pts',(5.36004692757343,2.94456578757346,17.2751780741665));
#6060=CARTESIAN_POINT('Ctrl Pts',(5.27628317816278,3.09215296421023,17.2829016279562));
#6061=CARTESIAN_POINT('Ctrl Pts',(5.18653100007008,3.23600397833687,17.2906251817459));
#6062=CARTESIAN_POINT('Ctrl Pts',(5.09678485014641,3.37984533076787,17.2983482167862));
#6063=CARTESIAN_POINT('Ctrl Pts',(5.00105124421418,3.51995075395075,17.3060712518265));
#6064=CARTESIAN_POINT('Ctrl Pts',(4.89966785666064,3.65582828602583,17.3137942868669));
#6065=CARTESIAN_POINT('Ctrl Pts',(4.79825752584036,3.7917419284014,17.3215193743518));
#6066=CARTESIAN_POINT('Ctrl Pts',(4.69119460102203,3.92342517897288,17.3292444618368));
#6067=CARTESIAN_POINT('Ctrl Pts',(4.5788585864185,4.0504172140758,17.3369695493218));
#6068=CARTESIAN_POINT('Ctrl Pts',(4.46695818007797,4.1769168088868,17.3446646810357));
#6069=CARTESIAN_POINT('Ctrl Pts',(4.34982573743811,4.29876129357617,17.3523598127496));
#6070=CARTESIAN_POINT('Ctrl Pts',(4.22787434760758,4.41552987345141,17.3600549444634));
#6071=CARTESIAN_POINT('Ctrl Pts',(4.105453380092,4.53274807443797,17.3677797065254));
#6072=CARTESIAN_POINT('Ctrl Pts',(3.97813290208805,4.64489269664158,17.3755044685874));
#6073=CARTESIAN_POINT('Ctrl Pts',(3.84635639015853,4.75156480355542,17.3832292306495));
#6074=CARTESIAN_POINT('Ctrl Pts',(3.71460558370688,4.85821610207599,17.3909524858519));
#6075=CARTESIAN_POINT('Ctrl Pts',(3.57840072394426,4.95939681610103,17.3986757410543));
#6076=CARTESIAN_POINT('Ctrl Pts',(3.43821844952761,5.05474820894453,17.4063989962567));
#6077=CARTESIAN_POINT('Ctrl Pts',(3.29803075772491,5.15010328667122,17.4141225499267));
#6078=CARTESIAN_POINT('Ctrl Pts',(3.15386560350442,5.23962841090903,17.4218461035966));
#6079=CARTESIAN_POINT('Ctrl Pts',(3.00622934323705,5.32300767408432,17.4295696572666));
#6080=CARTESIAN_POINT('Ctrl Pts',(2.85860299888143,5.40638133713526,17.4372926921881));
#6081=CARTESIAN_POINT('Ctrl Pts',(2.70750629100869,5.48360980931102,17.4450157271096));
#6082=CARTESIAN_POINT('Ctrl Pts',(2.5534711092405,5.55442263937253,17.4527387620311));
#6083=CARTESIAN_POINT('Ctrl Pts',(2.39939499160698,5.6252542884106,17.4604638494001));
#6084=CARTESIAN_POINT('Ctrl Pts',(2.24237912686077,5.68966675387982,17.4681889367691));
#6085=CARTESIAN_POINT('Ctrl Pts',(2.08297723906201,5.74743694041523,17.4759140241381));
#6086=CARTESIAN_POINT('Ctrl Pts',(1.92419345337507,5.80498311533579,17.4836091564489));
#6087=CARTESIAN_POINT('Ctrl Pts',(1.76304242048026,5.85593835633561,17.4913042887597));
#6088=CARTESIAN_POINT('Ctrl Pts',(1.60008820533714,5.90013078648609,17.4989994210706));
#6089=CARTESIAN_POINT('Ctrl Pts',(1.43650654518176,5.94449337682453,17.5067241830071));
#6090=CARTESIAN_POINT('Ctrl Pts',(1.27104984546179,5.98205665631764,17.5144489449435));
#6091=CARTESIAN_POINT('Ctrl Pts',(1.10429839739535,6.01268248055808,17.52217370688));
#6092=CARTESIAN_POINT('Ctrl Pts',(0.93757947735708,6.04330233065145,17.5298969619553));
#6093=CARTESIAN_POINT('Ctrl Pts',(0.769566624453821,6.06698736855961,17.5376202170306));
#6094=CARTESIAN_POINT('Ctrl Pts',(0.600850017635141,6.08365061610279,17.545343472106));
#6095=CARTESIAN_POINT('Ctrl Pts',(0.432126890741339,6.10031450759933,17.5530670256475));
#6096=CARTESIAN_POINT('Ctrl Pts',(0.262700270504094,6.10995603063614,17.560790579189));
#6097=CARTESIAN_POINT('Ctrl Pts',(0.0931659410739898,6.11254003421849,17.5685141327306));
#6098=CARTESIAN_POINT('Ctrl Pts',(-0.0763570016617557,6.11512386424745,
17.5762371675232));
#6099=CARTESIAN_POINT('Ctrl Pts',(-0.245987322192782,6.11065111857973,17.5839602023159));
#6100=CARTESIAN_POINT('Ctrl Pts',(-0.415128562593811,6.09913877846855,17.5916832371085));
#6101=CARTESIAN_POINT('Ctrl Pts',(-0.584314753407991,6.08762337887617,17.5994083243492));
#6102=CARTESIAN_POINT('Ctrl Pts',(-0.753011287801984,6.06906466585127,17.6071334115899));
#6103=CARTESIAN_POINT('Ctrl Pts',(-0.920625190894922,6.04353165131032,17.6148584988305));
#6104=CARTESIAN_POINT('Ctrl Pts',(-1.08758916531128,6.01809764191181,17.6225536317796));
#6105=CARTESIAN_POINT('Ctrl Pts',(-1.25347858560841,5.98574339992642,17.6302487647287));
#6106=CARTESIAN_POINT('Ctrl Pts',(-1.41771590051754,5.94658786094343,17.6379438976778));
#6107=CARTESIAN_POINT('Ctrl Pts',(-1.5825856064655,5.90728155468817,17.6456686605141));
#6108=CARTESIAN_POINT('Ctrl Pts',(-1.74584884389252,5.86110752076091,17.6533934233504));
#6109=CARTESIAN_POINT('Ctrl Pts',(-1.90692995148701,5.80822207931324,17.6611181861868));
#6110=CARTESIAN_POINT('Ctrl Pts',(-2.0679796372646,5.75534695413841,17.6688414421668));
#6111=CARTESIAN_POINT('Ctrl Pts',(-2.22684774163247,5.69576313253178,17.6765646981468));
#6112=CARTESIAN_POINT('Ctrl Pts',(-2.38297440002704,5.62967659562392,17.6842879541268));
#6113=CARTESIAN_POINT('Ctrl Pts',(-2.53910709193791,5.56358750480117,17.6920115085721));
#6114=CARTESIAN_POINT('Ctrl Pts',(-2.69249783248372,5.49099531570375,17.6997350630174));
#6115=CARTESIAN_POINT('Ctrl Pts',(-2.84260663067095,5.41215420195744,17.7074586174627));
#6116=CARTESIAN_POINT('Ctrl Pts',(-2.99270534682735,5.33331838356056,17.7151816531569));
#6117=CARTESIAN_POINT('Ctrl Pts',(-3.13952228113979,5.24823462780715,17.722904688851));
#6118=CARTESIAN_POINT('Ctrl Pts',(-3.28254179254823,5.15720320936399,17.7306277245452));
#6119=CARTESIAN_POINT('Ctrl Pts',(-3.42559931210905,5.06614759886487,17.7383528126748));
#6120=CARTESIAN_POINT('Ctrl Pts',(-3.56485712344945,4.96914133566764,17.7460779008044));
#6121=CARTESIAN_POINT('Ctrl Pts',(-3.69982753705317,4.86652871753194,17.753802988934));
#6122=CARTESIAN_POINT('Ctrl Pts',(-3.83427450416188,4.7643140548731,17.7614981173843));
#6123=CARTESIAN_POINT('Ctrl Pts',(-3.96446704044143,4.65653666005199,17.7691932458347));
#6124=CARTESIAN_POINT('Ctrl Pts',(-4.08995488612825,4.54357729019059,17.776888374285));
#6125=CARTESIAN_POINT('Ctrl Pts',(-4.21592595010033,4.43018294566921,17.7846131345037));
#6126=CARTESIAN_POINT('Ctrl Pts',(-4.33720061386398,4.3115264549399,17.7923378947224));
#6127=CARTESIAN_POINT('Ctrl Pts',(-4.45334816253895,4.18802049967654,17.800062654941));
#6128=CARTESIAN_POINT('Ctrl Pts',(-4.5694730543394,4.06453863669032,17.8077859082926));
#6129=CARTESIAN_POINT('Ctrl Pts',(-4.68047260971287,3.93620942747956,17.8155091616442));
#6130=CARTESIAN_POINT('Ctrl Pts',(-4.78595374457437,3.80348160470042,17.8232324149957));
#6131=CARTESIAN_POINT('Ctrl Pts',(-4.89143895586818,3.67074865251133,17.8309559668207));
#6132=CARTESIAN_POINT('Ctrl Pts',(-4.99140511961486,3.53361699224015,17.8386795186457));
#6133=CARTESIAN_POINT('Ctrl Pts',(-5.08549965992524,3.3925681675392,17.8464030704707));
#6134=CARTESIAN_POINT('Ctrl Pts',(-5.17958788050771,3.25152881618485,17.8541261035542));
#6135=CARTESIAN_POINT('Ctrl Pts',(-5.26780509094031,3.10657309056353,17.8618491366377));
#6136=CARTESIAN_POINT('Ctrl Pts',(-5.34984215373234,2.95821136713531,17.8695721697212));
#6137=CARTESIAN_POINT('Ctrl Pts',(-5.43190101873005,2.80981021503058,17.8772972552813));
#6138=CARTESIAN_POINT('Ctrl Pts',(-5.50777629871879,2.65800153284127,17.8850223408414));
#6139=CARTESIAN_POINT('Ctrl Pts',(-5.57720446312307,2.50332098201971,17.8927474264016));
#6140=CARTESIAN_POINT('Ctrl Pts',(-5.64636350929811,2.3492400056834,17.9004425678984));
#6141=CARTESIAN_POINT('Ctrl Pts',(-5.70912523340383,2.19230968310618,17.9081377093953));
#6142=CARTESIAN_POINT('Ctrl Pts',(-5.7652764148881,2.03307978752312,17.9158328508922));
#6143=CARTESIAN_POINT('Ctrl Pts',(-5.82269509056864,1.87025561372202,17.9237016939378));
#6144=CARTESIAN_POINT('Ctrl Pts',(-5.87322249350811,1.7049664635386,17.9315705369834));
#6145=CARTESIAN_POINT('Ctrl Pts',(-5.91666753870068,1.5378136424761,17.939439380029));
#6146=CARTESIAN_POINT('Ctrl Pts',(-5.95928261330902,1.37385409521363,17.9471578973417));
#6147=CARTESIAN_POINT('Ctrl Pts',(-5.99508342088484,1.20810176362181,17.9548764146544));
#6148=CARTESIAN_POINT('Ctrl Pts',(-6.02394029638027,1.04113825601887,17.9625949319671));
#6149=CARTESIAN_POINT('Ctrl Pts',(-6.053640196018,0.869297080082928,17.9705389378791));
#6150=CARTESIAN_POINT('Ctrl Pts',(-6.07598418494458,0.696173225030384,17.9784829437912));
#6151=CARTESIAN_POINT('Ctrl Pts',(-6.09088764263035,0.522411032954849,17.9864269497033));
#6152=CARTESIAN_POINT('Ctrl Pts',(-6.10579110031611,0.348648840879286,17.9943709556154));
#6153=CARTESIAN_POINT('Ctrl Pts',(-6.11325399540428,0.17424867745491,18.0023149615274));
#6154=CARTESIAN_POINT('Ctrl Pts',(-6.11324999839426,-0.000140116351456561,
18.0102589674395));
#6155=CARTESIAN_POINT('Ctrl Pts',(-6.11298206926134,-0.000140309528671095,
18.0102589765195));
#6156=CARTESIAN_POINT('Ctrl Pts',(-6.11325663468543,-0.325885343511412,
18.0250984268461));
#6157=CARTESIAN_POINT('Ctrl Pts',(-6.00780900954066,-1.6681244042226,18.0862527027085));
#6158=CARTESIAN_POINT('Ctrl Pts',(-5.03941570755938,-3.90065628250744,18.1937218041066));
#6159=CARTESIAN_POINT('Ctrl Pts',(-2.55905445660959,-5.83627165166331,18.3326662807137));
#6160=CARTESIAN_POINT('Ctrl Pts',(0.545070549309975,-6.34930960566648,18.4716107573209));
#6161=CARTESIAN_POINT('Ctrl Pts',(2.66550147956873,-5.61097601765261,18.5707678899492));
#6162=CARTESIAN_POINT('Ctrl Pts',(3.60955744708097,-4.93645179362417,18.6236101970417));
#6163=CARTESIAN_POINT('Ctrl Pts',(3.72309647396852,-4.84910580413568,18.6301376785985));
#6164=CARTESIAN_POINT('',(-6.11277358809404,-6.86038334901315E-5,17.8647410325606));
#6165=CARTESIAN_POINT('Ctrl Pts',(-6.11277358809404,-6.86038334901315E-5,
17.8647410325606));
#6166=CARTESIAN_POINT('Ctrl Pts',(-6.11294404322182,-0.432525236900348,
17.8844398491494));
#6167=CARTESIAN_POINT('Ctrl Pts',(-5.96131848459198,-1.88163345335141,17.950453491274));
#6168=CARTESIAN_POINT('Ctrl Pts',(-4.82844309209128,-4.15896220843452,18.0627819589343));
#6169=CARTESIAN_POINT('Ctrl Pts',(-2.25021276710887,-5.96216166444017,18.2017264355415));
#6170=CARTESIAN_POINT('Ctrl Pts',(0.876501925825786,-6.31209741621358,18.3406709121487));
#6171=CARTESIAN_POINT('Ctrl Pts',(2.85349283772427,-5.50542282114631,18.4349673180294));
#6172=CARTESIAN_POINT('Ctrl Pts',(3.69423076344769,-4.87156667330043,18.4829488983743));
#6173=CARTESIAN_POINT('Ctrl Pts',(3.72323265631121,-4.849283219867,18.4846156531836));
#6174=CARTESIAN_POINT('Ctrl Pts',(3.72262360719331,-4.84849058816218,16.7346163843234));
#6175=CARTESIAN_POINT('Ctrl Pts',(4.17330897152384,-4.50222738608563,16.7605048127054));
#6176=CARTESIAN_POINT('Ctrl Pts',(5.29718827570009,-3.36293425993741,16.8327080666233));
#6177=CARTESIAN_POINT('Ctrl Pts',(6.31182959594577,-0.878428397354582,16.9512261460768));
#6178=CARTESIAN_POINT('Ctrl Pts',(5.96284817531305,2.24839296747554,17.090170622684));
#6179=CARTESIAN_POINT('Ctrl Pts',(4.16043569152321,4.82717351599487,17.2291150992912));
#6180=CARTESIAN_POINT('Ctrl Pts',(1.34392620390646,6.22934118968737,17.3680595758984));
#6181=CARTESIAN_POINT('Ctrl Pts',(-1.80016232579228,6.11312071668258,17.5070040525056));
#6182=CARTESIAN_POINT('Ctrl Pts',(-4.50546526677362,4.50684058160178,17.6459485291127));
#6183=CARTESIAN_POINT('Ctrl Pts',(-5.88472401532739,2.18550210418407,17.7651941891311));
#6184=CARTESIAN_POINT('Ctrl Pts',(-6.11254327805558,0.584244142210199,17.8381250236137));
#6185=CARTESIAN_POINT('Ctrl Pts',(-6.11277358809404,-6.86038334901315E-5,
17.8647410325606));
#6186=CARTESIAN_POINT('Origin',(0.,0.,-3.86474103256053));
#6187=CARTESIAN_POINT('',(3.72292453512039,-4.84888218750452,14.984609455652));
#6188=CARTESIAN_POINT('',(3.7229245351204,-4.84888218750451,15.1301297587947));
#6189=CARTESIAN_POINT('',(3.72292453512038,-4.84888218750453,-3.86474103256053));
#6190=CARTESIAN_POINT('',(-6.11324999939832,8.57698500699812E-5,16.2602589674827));
#6191=CARTESIAN_POINT('Ctrl Pts',(3.7229245351204,-4.84888218750451,15.1301297587947));
#6192=CARTESIAN_POINT('Ctrl Pts',(3.76245440720127,-4.81853153658144,15.132400945446));
#6193=CARTESIAN_POINT('Ctrl Pts',(3.8016112547446,-4.78769889512472,15.1346721320972));
#6194=CARTESIAN_POINT('Ctrl Pts',(3.84038328103664,-4.75639378281848,15.1369433187484));
#6195=CARTESIAN_POINT('Ctrl Pts',(3.9722547321136,-4.6499188063791,15.1446680808516));
#6196=CARTESIAN_POINT('Ctrl Pts',(4.09971876394751,-4.53793737361086,15.1523928429548));
#6197=CARTESIAN_POINT('Ctrl Pts',(4.22232314811218,-4.42083847198877,15.160117605058));
#6198=CARTESIAN_POINT('Ctrl Pts',(4.34490361599038,-4.30376241270545,15.1678408603013));
#6199=CARTESIAN_POINT('Ctrl Pts',(4.46262609868169,-4.18157109521427,15.1755641155446));
#6200=CARTESIAN_POINT('Ctrl Pts',(4.57507401088148,-4.05469152432794,15.183287370788));
#6201=CARTESIAN_POINT('Ctrl Pts',(4.68752626865271,-3.92780705015592,15.191010924498));
#6202=CARTESIAN_POINT('Ctrl Pts',(4.79470333487811,-3.79623419458935,15.1987344782081));
#6203=CARTESIAN_POINT('Ctrl Pts',(4.89622731440188,-3.66043489877978,15.2064580319181));
#6204=CARTESIAN_POINT('Ctrl Pts',(4.99774447511432,-3.52464472386738,15.2141810668792));
#6205=CARTESIAN_POINT('Ctrl Pts',(5.0936091191614,-3.38462893063772,15.2219041018403));
#6206=CARTESIAN_POINT('Ctrl Pts',(5.18348518087997,-3.24088058127691,15.2296271368015));
#6207=CARTESIAN_POINT('Ctrl Pts',(5.27338512774033,-3.09709402986718,15.2373522242088));
#6208=CARTESIAN_POINT('Ctrl Pts',(5.35729314207805,-2.94957320792683,15.2450773116162));
#6209=CARTESIAN_POINT('Ctrl Pts',(5.4349173433979,-2.79883887227055,15.2528023990235));
#6210=CARTESIAN_POINT('Ctrl Pts',(5.51224054411334,-2.64868903378612,15.2604975311342));
#6211=CARTESIAN_POINT('Ctrl Pts',(5.58332846394801,-2.49535085144685,15.2681926632449));
#6212=CARTESIAN_POINT('Ctrl Pts',(5.64793870418822,-2.33936186944917,15.2758877953556));
#6213=CARTESIAN_POINT('Ctrl Pts',(5.71279772520409,-2.18277225418048,15.2836125574588));
#6214=CARTESIAN_POINT('Ctrl Pts',(5.77115202657654,-2.02345591412792,15.291337319562));
#6215=CARTESIAN_POINT('Ctrl Pts',(5.82279059770343,-1.86197078865287,15.2990620816653));
#6216=CARTESIAN_POINT('Ctrl Pts',(5.87441909575774,-1.70051716388269,15.3067853369086));
#6217=CARTESIAN_POINT('Ctrl Pts',(5.91933438107333,-1.53689589953577,15.314508592152));
#6218=CARTESIAN_POINT('Ctrl Pts',(5.95737493080978,-1.37168126627841,15.3222318473954));
#6219=CARTESIAN_POINT('Ctrl Pts',(5.99541695063063,-1.20646024826962,15.3299554011054));
#6220=CARTESIAN_POINT('Ctrl Pts',(6.0265836282697,-1.0396460460813,15.3376789548155));
#6221=CARTESIAN_POINT('Ctrl Pts',(6.05076413028251,-0.871825098392158,15.3454025085256));
#6222=CARTESIAN_POINT('Ctrl Pts',(6.07494300822306,-0.704015422319585,15.3531255434867));
#6223=CARTESIAN_POINT('Ctrl Pts',(6.09213660433438,-0.535199449778643,15.3608485784478));
#6224=CARTESIAN_POINT('Ctrl Pts',(6.10228570595457,-0.365970935188203,15.368571613409));
#6225=CARTESIAN_POINT('Ctrl Pts',(6.1124375047638,-0.196697447031413,15.3762967008163));
#6226=CARTESIAN_POINT('Ctrl Pts',(6.11554104697018,-0.0270115141970811,
15.3840217882237));
#6227=CARTESIAN_POINT('Ctrl Pts',(6.11158916998146,0.142489928996134,15.3917468756311));
#6228=CARTESIAN_POINT('Ctrl Pts',(6.10765261704564,0.311334102469584,15.3994420077416));
#6229=CARTESIAN_POINT('Ctrl Pts',(6.09671530424912,0.479994903183618,15.4071371398522));
#6230=CARTESIAN_POINT('Ctrl Pts',(6.07882155181818,0.64788432891283,15.4148322719628));
#6231=CARTESIAN_POINT('Ctrl Pts',(6.06085889975761,0.816420210397759,15.422557034066));
#6232=CARTESIAN_POINT('Ctrl Pts',(6.03587973868905,0.984238451982329,15.4302817961692));
#6233=CARTESIAN_POINT('Ctrl Pts',(6.00396570920228,1.15074815890495,15.4380065582724));
#6234=CARTESIAN_POINT('Ctrl Pts',(5.97205790514611,1.31722538498324,15.4457298135157));
#6235=CARTESIAN_POINT('Ctrl Pts',(5.93321799156638,1.48239427465142,15.453453068759));
#6236=CARTESIAN_POINT('Ctrl Pts',(5.88757887892222,1.64567326859523,15.4611763240023));
#6237=CARTESIAN_POINT('Ctrl Pts',(5.84193800254567,1.80895857248757,15.4688998777124));
#6238=CARTESIAN_POINT('Ctrl Pts',(5.78949748281174,1.97035352822206,15.4766234314224));
#6239=CARTESIAN_POINT('Ctrl Pts',(5.73044056339439,2.1292901427246,15.4843469851324));
#6240=CARTESIAN_POINT('Ctrl Pts',(5.67138761050764,2.28821608232317,15.4920700200935));
#6241=CARTESIAN_POINT('Ctrl Pts',(5.6057192576342,2.44468371400129,15.4997930550547));
#6242=CARTESIAN_POINT('Ctrl Pts',(5.53366757806885,2.59814331743451,15.5075160900158));
#6243=CARTESIAN_POINT('Ctrl Pts',(5.46159675030623,2.75164370374437,15.5152411774231));
#6244=CARTESIAN_POINT('Ctrl Pts',(5.38313933882879,2.90213417640021,15.5229662648305));
#6245=CARTESIAN_POINT('Ctrl Pts',(5.29857464481329,3.04908712500015,15.5306913522378));
#6246=CARTESIAN_POINT('Ctrl Pts',(5.21433786430333,3.19547023937927,15.5383864843485));
#6247=CARTESIAN_POINT('Ctrl Pts',(5.12404126469462,3.33834296108946,15.5460816164593));
#6248=CARTESIAN_POINT('Ctrl Pts',(5.02800508219621,3.47721015411912,15.55377674857));
#6249=CARTESIAN_POINT('Ctrl Pts',(4.9315991137962,3.61661205322351,15.5615015106732));
#6250=CARTESIAN_POINT('Ctrl Pts',(4.82937510558569,3.75202687088283,15.5692262727764));
#6251=CARTESIAN_POINT('Ctrl Pts',(4.72168744963309,3.88297478622735,15.5769510348796));
#6252=CARTESIAN_POINT('Ctrl Pts',(4.6140208001795,4.01389715772259,15.5846742901229));
#6253=CARTESIAN_POINT('Ctrl Pts',(4.50089283079175,4.140354120929,15.5923975453663));
#6254=CARTESIAN_POINT('Ctrl Pts',(4.38269848859789,4.26189858168185,15.6001208006096));
#6255=CARTESIAN_POINT('Ctrl Pts',(4.26449957876029,4.38344773954444,15.6078443543197));
#6256=CARTESIAN_POINT('Ctrl Pts',(4.14123412242871,4.500083785097,15.6155679080297));
#6257=CARTESIAN_POINT('Ctrl Pts',(4.01333477515508,4.61139561792641,15.6232914617398));
#6258=CARTESIAN_POINT('Ctrl Pts',(3.88544401818213,4.7226999745479,15.6310144967009));
#6259=CARTESIAN_POINT('Ctrl Pts',(3.75292023218975,4.82868062598211,15.6387375316621));
#6260=CARTESIAN_POINT('Ctrl Pts',(3.61623020907674,4.92896587911306,15.6464605666232));
#6261=CARTESIAN_POINT('Ctrl Pts',(3.47950385971076,5.02927778369517,15.6541856540306));
#6262=CARTESIAN_POINT('Ctrl Pts',(3.33860931518214,5.12389107609201,15.6619107414379));
#6263=CARTESIAN_POINT('Ctrl Pts',(3.19404426139221,5.21247607368777,15.6696358288453));
#6264=CARTESIAN_POINT('Ctrl Pts',(3.05003978237056,5.30071756838848,15.6773309609559));
#6265=CARTESIAN_POINT('Ctrl Pts',(2.90239349252378,5.38297730096494,15.6850260930666));
#6266=CARTESIAN_POINT('Ctrl Pts',(2.75162348717553,5.4589736899278,15.6927212251772));
#6267=CARTESIAN_POINT('Ctrl Pts',(2.60027294414747,5.53526270186446,15.7004459872804));
#6268=CARTESIAN_POINT('Ctrl Pts',(2.44572096485065,5.6052670331009,15.7081707493836));
#6269=CARTESIAN_POINT('Ctrl Pts',(2.28850831054869,5.66873489193573,15.7158955114869));
#6270=CARTESIAN_POINT('Ctrl Pts',(2.13132632352709,5.7321903701729,15.7236187667302));
#6271=CARTESIAN_POINT('Ctrl Pts',(1.97148499082358,5.78911180164311,15.7313420219735));
#6272=CARTESIAN_POINT('Ctrl Pts',(1.8095450287456,5.83929553554554,15.7390652772168));
#6273=CARTESIAN_POINT('Ctrl Pts',(1.64759880846544,5.88948120880839,15.7467888309269));
#6274=CARTESIAN_POINT('Ctrl Pts',(1.48355409806413,5.9329285658752,15.7545123846369));
#6275=CARTESIAN_POINT('Ctrl Pts',(1.31798750613703,5.96948360381086,15.762235938347));
#6276=CARTESIAN_POINT('Ctrl Pts',(1.15243203441399,6.0060361865442,15.7699589733081));
#6277=CARTESIAN_POINT('Ctrl Pts',(0.985355195221883,6.03569730819591,15.7776820082692));
#6278=CARTESIAN_POINT('Ctrl Pts',(0.817344719570005,6.05836390223392,15.7854050432304));
#6279=CARTESIAN_POINT('Ctrl Pts',(0.649289594052713,6.08103652006521,15.7931301306377));
#6280=CARTESIAN_POINT('Ctrl Pts',(0.480300650282989,6.09671085130451,15.8008552180451));
#6281=CARTESIAN_POINT('Ctrl Pts',(0.310972649048222,6.10533550053098,15.8085803054525));
#6282=CARTESIAN_POINT('Ctrl Pts',(0.142301244982609,6.11392670626184,15.8162754375631));
#6283=CARTESIAN_POINT('Ctrl Pts',(-0.0267062782955295,6.11552282170934,
15.8239705696738));
#6284=CARTESIAN_POINT('Ctrl Pts',(-0.195460250937893,6.11012445477204,15.8316657017844));
#6285=CARTESIAN_POINT('Ctrl Pts',(-0.364864008257741,6.10470530150263,15.8393904638875));
#6286=CARTESIAN_POINT('Ctrl Pts',(-0.534072255290258,6.09223574530779,15.8471152259906));
#6287=CARTESIAN_POINT('Ctrl Pts',(-0.702489670939348,6.0727533973251,15.8548399880937));
#6288=CARTESIAN_POINT('Ctrl Pts',(-0.870874233610243,6.05327484974007,15.8625632433369));
#6289=CARTESIAN_POINT('Ctrl Pts',(-1.03846795807886,6.0267862763673,15.8702864985802));
#6290=CARTESIAN_POINT('Ctrl Pts',(-1.20468103221891,5.99337710920245,15.8780097538234));
#6291=CARTESIAN_POINT('Ctrl Pts',(-1.37090052969557,5.95996665093384,15.8857333075334));
#6292=CARTESIAN_POINT('Ctrl Pts',(-1.53573895859188,5.91963512226245,15.8934568612434));
#6293=CARTESIAN_POINT('Ctrl Pts',(-1.6986163043397,5.87252315560623,15.9011804149533));
#6294=CARTESIAN_POINT('Ctrl Pts',(-1.86148271050534,5.82541435320363,15.9089034499143));
#6295=CARTESIAN_POINT('Ctrl Pts',(-2.02238799263181,5.77152611223166,15.9166264848753));
#6296=CARTESIAN_POINT('Ctrl Pts',(-2.18076673873388,5.71104911498159,15.9243495198363));
#6297=CARTESIAN_POINT('Ctrl Pts',(-2.33918757500708,5.65055604558026,15.9320746072436));
#6298=CARTESIAN_POINT('Ctrl Pts',(-2.49508023648761,5.58347083206893,15.9397996946509));
#6299=CARTESIAN_POINT('Ctrl Pts',(-2.64789785912929,5.51003289374197,15.9475247820581));
#6300=CARTESIAN_POINT('Ctrl Pts',(-2.80012290632238,5.43687972309099,15.9552199141693));
#6301=CARTESIAN_POINT('Ctrl Pts',(-2.94929645279987,5.35742317179202,15.9629150462804));
#6302=CARTESIAN_POINT('Ctrl Pts',(-3.09490098491087,5.27194588895767,15.9706101783916));
#6303=CARTESIAN_POINT('Ctrl Pts',(-3.24106616511833,5.18613947711053,15.9783349404951));
#6304=CARTESIAN_POINT('Ctrl Pts',(-3.38368654368243,5.09423546024153,15.9860597025986));
#6305=CARTESIAN_POINT('Ctrl Pts',(-3.52225734787587,4.9965516846956,15.9937844647021));
#6306=CARTESIAN_POINT('Ctrl Pts',(-3.6608011212315,4.89888696420466,16.0015077199456));
#6307=CARTESIAN_POINT('Ctrl Pts',(-3.79529663756409,4.79544491719618,16.0092309751892));
#6308=CARTESIAN_POINT('Ctrl Pts',(-3.92526875433068,4.68658625961107,16.0169542304328));
#6309=CARTESIAN_POINT('Ctrl Pts',(-4.0552458938957,4.57772339516137,16.0246777841431));
#6310=CARTESIAN_POINT('Ctrl Pts',(-4.18069903859237,4.46344370171458,16.0324013378534));
#6311=CARTESIAN_POINT('Ctrl Pts',(-4.30118614514863,4.34414816820069,16.0401248915637));
#6312=CARTESIAN_POINT('Ctrl Pts',(-4.42166515924376,4.22486064711649,16.0478479265251));
#6313=CARTESIAN_POINT('Ctrl Pts',(-4.53717857744093,4.1005581831413,16.0555709614865));
#6314=CARTESIAN_POINT('Ctrl Pts',(-4.64732112470052,3.97167872900267,16.0632939964478));
#6315=CARTESIAN_POINT('Ctrl Pts',(-4.75749294305095,3.84276502431962,16.0710190838555));
#6316=CARTESIAN_POINT('Ctrl Pts',(-4.86229083058074,3.7092721385642,16.0787441712631));
#6317=CARTESIAN_POINT('Ctrl Pts',(-4.96134911688746,3.57167194782219,16.0864692586707));
#6318=CARTESIAN_POINT('Ctrl Pts',(-5.06002328838043,3.43460532447378,16.0941643907801));
#6319=CARTESIAN_POINT('Ctrl Pts',(-5.15300213578692,3.29346346521625,16.1018595228894));
#6320=CARTESIAN_POINT('Ctrl Pts',(-5.23996644446237,3.1487421652794,16.1095546549988));
#6321=CARTESIAN_POINT('Ctrl Pts',(-5.32726560793197,3.00346361810126,16.1172794171014));
#6322=CARTESIAN_POINT('Ctrl Pts',(-5.4085347159692,2.85452654155278,16.125004179204));
#6323=CARTESIAN_POINT('Ctrl Pts',(-5.48348258145226,2.70245154284211,16.1327289413066));
#6324=CARTESIAN_POINT('Ctrl Pts',(-5.55841582694723,2.55040620921468,16.1404521965494));
#6325=CARTESIAN_POINT('Ctrl Pts',(-5.62703015030143,2.39522445891001,16.1481754517922));
#6326=CARTESIAN_POINT('Ctrl Pts',(-5.68908089349989,2.23745036810083,16.1558987070349));
#6327=CARTESIAN_POINT('Ctrl Pts',(-5.75113403466138,2.07967018008122,16.1636222607444));
#6328=CARTESIAN_POINT('Ctrl Pts',(-5.80662296841791,1.91929774456649,16.1713458144538));
#6329=CARTESIAN_POINT('Ctrl Pts',(-5.8553513698642,1.75689666683316,16.1790693681633));
#6330=CARTESIAN_POINT('Ctrl Pts',(-5.90407649848985,1.59450649669339,16.1867924031238));
#6331=CARTESIAN_POINT('Ctrl Pts',(-5.94604191238515,1.43008826058703,16.1945154380843));
#6332=CARTESIAN_POINT('Ctrl Pts',(-5.98110125835133,1.26422043166854,16.2022384730448));
#6333=CARTESIAN_POINT('Ctrl Pts',(-6.01616992156442,1.09830852230657,16.2099635604516));
#6334=CARTESIAN_POINT('Ctrl Pts',(-6.04432878169025,0.930946560175674,16.2176886478584));
#6335=CARTESIAN_POINT('Ctrl Pts',(-6.06548249332253,0.762723859399947,16.2254137352652));
#6336=CARTESIAN_POINT('Ctrl Pts',(-6.08655417796907,0.59515346973237,16.2331088673788));
#6337=CARTESIAN_POINT('Ctrl Pts',(-6.100674937807,0.426729318635894,16.2408039994924));
#6338=CARTESIAN_POINT('Ctrl Pts',(-6.10780166506172,0.258039498467358,16.2484991316059));
#6339=CARTESIAN_POINT('Ctrl Pts',(-6.11143206158205,0.172107918056641,16.2524190768838));
#6340=CARTESIAN_POINT('Ctrl Pts',(-6.11324879259944,0.0860994634106513,
16.2563390221616));
#6341=CARTESIAN_POINT('Ctrl Pts',(-6.1132499993983,8.57707989032423E-5,
16.2602589674395));
#6342=CARTESIAN_POINT('Ctrl Pts',(-6.11324999939832,8.5769850077377E-5,
16.2602589674827));
#6343=CARTESIAN_POINT('Ctrl Pts',(-6.11325237018008,-0.168891809259724,
16.2679598676903));
#6344=CARTESIAN_POINT('Ctrl Pts',(-6.10624428268917,-0.337901014722052,
16.2756607678979));
#6345=CARTESIAN_POINT('Ctrl Pts',(-6.09224393255344,-0.506349117473063,
16.2833616681055));
#6346=CARTESIAN_POINT('Ctrl Pts',(-6.07824623187471,-0.674765342735428,
16.2910611109779));
#6347=CARTESIAN_POINT('Ctrl Pts',(-6.05725893532342,-0.842620357625315,
16.2987605538503));
#6348=CARTESIAN_POINT('Ctrl Pts',(-6.02935220866743,-1.00932527281206,16.3064599967226));
#6349=CARTESIAN_POINT('Ctrl Pts',(-6.00144454055709,-1.17603581191415,16.3141596993414));
#6350=CARTESIAN_POINT('Ctrl Pts',(-5.9666170251134,-1.34159585676452,16.3218594019603));
#6351=CARTESIAN_POINT('Ctrl Pts',(-5.92499130018901,-1.5054247424513,16.3295591045791));
#6352=CARTESIAN_POINT('Ctrl Pts',(-5.88336701750354,-1.66924795183102,16.3372585404204));
#6353=CARTESIAN_POINT('Ctrl Pts',(-5.83494507717228,-1.83133981152082,16.3449579762616));
#6354=CARTESIAN_POINT('Ctrl Pts',(-5.77989758545023,-1.99113270883853,16.3526574121029));
#6355=CARTESIAN_POINT('Ctrl Pts',(-5.7248371957853,-2.1509630465481,16.360358651966));
#6356=CARTESIAN_POINT('Ctrl Pts',(-5.66314825791892,-2.3084930423638,16.3680598918293));
#6357=CARTESIAN_POINT('Ctrl Pts',(-5.59505208858061,-2.46317228154462,16.3757611316925));
#6358=CARTESIAN_POINT('Ctrl Pts',(-5.56061902266852,-2.54138637919064,16.3796552905327));
#6359=CARTESIAN_POINT('Ctrl Pts',(-5.5245484894734,-2.61887188728961,16.3835494493729));
#6360=CARTESIAN_POINT('Ctrl Pts',(-5.48687372986159,-2.69555972574432,16.3874436082131));
#6361=CARTESIAN_POINT('Ctrl Pts',(-5.41213909083035,-2.84768379990036,16.3951683703152));
#6362=CARTESIAN_POINT('Ctrl Pts',(-5.33106083836323,-2.99672486023318,16.4028931324173));
#6363=CARTESIAN_POINT('Ctrl Pts',(-5.24391852388584,-3.14215596006101,16.4106178945194));
#6364=CARTESIAN_POINT('Ctrl Pts',(-5.15679320815288,-3.28755869082253,16.4183411497616));
#6365=CARTESIAN_POINT('Ctrl Pts',(-5.06360635353548,-3.42935259449848,16.4260644050038));
#6366=CARTESIAN_POINT('Ctrl Pts',(-4.96468245966836,-3.56703709500775,16.4337876602461));
#6367=CARTESIAN_POINT('Ctrl Pts',(-4.86575474286792,-3.70472691636161,16.441511213955));
#6368=CARTESIAN_POINT('Ctrl Pts',(-4.76108972486681,-3.83830675707666,16.4492347676639));
#6369=CARTESIAN_POINT('Ctrl Pts',(-4.65105452122077,-3.96730606370769,16.4569583213729));
#6370=CARTESIAN_POINT('Ctrl Pts',(-4.54102670803836,-4.09629670615987,16.4646813563329));
#6371=CARTESIAN_POINT('Ctrl Pts',(-4.42562963670314,-4.22070718904318,16.4724043912929));
#6372=CARTESIAN_POINT('Ctrl Pts',(-4.30527001059718,-4.3401008857344,16.4801274262529));
#6373=CARTESIAN_POINT('Ctrl Pts',(-4.18487839814579,-4.45952631206909,16.4878525136592));
#6374=CARTESIAN_POINT('Ctrl Pts',(-4.05952181920495,-4.573932063167,16.4955776010655));
#6375=CARTESIAN_POINT('Ctrl Pts',(-3.92964374318109,-4.68291849322382,16.5033026884717));
#6376=CARTESIAN_POINT('Ctrl Pts',(-3.8002692906423,-4.79148231057025,16.5109978205879));
#6377=CARTESIAN_POINT('Ctrl Pts',(-3.66640860424335,-4.8946685847889,16.5186929527041));
#6378=CARTESIAN_POINT('Ctrl Pts',(-3.52853245062451,-4.99212222480478,16.5263880848203));
#6379=CARTESIAN_POINT('Ctrl Pts',(-3.39012540701131,-5.08995110855236,16.5341128469236));
#6380=CARTESIAN_POINT('Ctrl Pts',(-3.24762287481692,-5.18203774718436,16.5418376090268));
#6381=CARTESIAN_POINT('Ctrl Pts',(-3.1015224421497,-5.2680531606412,16.54956237113));
#6382=CARTESIAN_POINT('Ctrl Pts',(-2.95545050911474,-5.35405179517681,16.5572856263734));
#6383=CARTESIAN_POINT('Ctrl Pts',(-2.80578234896859,-5.43398140695962,16.5650088816168));
#6384=CARTESIAN_POINT('Ctrl Pts',(-2.65304240354883,-5.50755767718068,16.5727321368602));
#6385=CARTESIAN_POINT('Ctrl Pts',(-2.50029655546385,-5.58113679077117,16.5804556905702));
#6386=CARTESIAN_POINT('Ctrl Pts',(-2.34447896835884,-5.64836193038159,16.5881792442803));
#6387=CARTESIAN_POINT('Ctrl Pts',(-2.18613714251705,-5.70899552956625,16.5959027979904));
#6388=CARTESIAN_POINT('Ctrl Pts',(-2.02780595163096,-5.76962505632318,16.6036258329516));
#6389=CARTESIAN_POINT('Ctrl Pts',(-1.86695115728414,-5.82366381526525,16.6113488679128));
#6390=CARTESIAN_POINT('Ctrl Pts',(-1.70413879127973,-5.87092297194876,16.6190719028739));
#6391=CARTESIAN_POINT('Ctrl Pts',(-1.54128315684185,-5.91819468805713,16.6267969902813));
#6392=CARTESIAN_POINT('Ctrl Pts',(-1.37646921515672,-5.95868311112467,16.6345220776887));
#6393=CARTESIAN_POINT('Ctrl Pts',(-1.21027759052793,-5.99224947047149,16.6422471650961));
#6394=CARTESIAN_POINT('Ctrl Pts',(-1.0447304012558,-6.02568567073957,16.6499422972066));
#6395=CARTESIAN_POINT('Ctrl Pts',(-0.877816506823421,-6.05225336453254,
16.657637429317));
#6396=CARTESIAN_POINT('Ctrl Pts',(-0.710119185660943,-6.07186596563661,
16.6653325614275));
#6397=CARTESIAN_POINT('Ctrl Pts',(-0.541776148346675,-6.0915540847825,16.6730573235348));
#6398=CARTESIAN_POINT('Ctrl Pts',(-0.372584013597159,-6.10424038706862,
16.6807820856421));
#6399=CARTESIAN_POINT('Ctrl Pts',(-0.203137120202453,-6.10987404722027,
16.6885068477494));
#6400=CARTESIAN_POINT('Ctrl Pts',(-0.0337232806044481,-6.11550660842078,
16.6962301029969));
#6401=CARTESIAN_POINT('Ctrl Pts',(0.135944901919463,-6.11408926207646,16.7039533582444));
#6402=CARTESIAN_POINT('Ctrl Pts',(0.305270874867088,-6.1056232487321,16.7116766134919));
#6403=CARTESIAN_POINT('Ctrl Pts',(0.474603391450264,-6.09715690821698,16.7194001672061));
#6404=CARTESIAN_POINT('Ctrl Pts',(0.643593355273245,-6.08164136748782,16.7271237209203));
#6405=CARTESIAN_POINT('Ctrl Pts',(0.811646333308634,-6.05912995339485,16.7348472746345));
#6406=CARTESIAN_POINT('Ctrl Pts',(0.979688024142844,-6.03662005127067,16.7425703095997));
#6407=CARTESIAN_POINT('Ctrl Pts',(1.14679254097663,-6.00711525816716,16.750293344565));
#6408=CARTESIAN_POINT('Ctrl Pts',(1.31237249258622,-5.97072055979871,16.7580163795302));
#6409=CARTESIAN_POINT('Ctrl Pts',(1.47799644813229,-5.93431618930523,16.7657414669417));
#6410=CARTESIAN_POINT('Ctrl Pts',(1.64209471861648,-5.89101832064699,16.7734665543531));
#6411=CARTESIAN_POINT('Ctrl Pts',(1.80409105072818,-5.84098288331531,16.7811916417646));
#6412=CARTESIAN_POINT('Ctrl Pts',(1.96545921490648,-5.79114146677939,16.7888867738546));
#6413=CARTESIAN_POINT('Ctrl Pts',(2.12474142420005,-5.73461476372079,16.7965819059447));
#6414=CARTESIAN_POINT('Ctrl Pts',(2.2813840612205,-5.67160579798253,16.8042770380347));
#6415=CARTESIAN_POINT('Ctrl Pts',(2.43863116068549,-5.60835368929046,16.8120018645837));
#6416=CARTESIAN_POINT('Ctrl Pts',(2.59327395733649,-5.53854675995458,16.8197266911327));
#6417=CARTESIAN_POINT('Ctrl Pts',(2.74476621688423,-5.46242473423213,16.8274515176816));
#6418=CARTESIAN_POINT('Ctrl Pts',(2.89622663670497,-5.38631870737674,16.8351747206733));
#6419=CARTESIAN_POINT('Ctrl Pts',(3.04453755791828,-5.30390037524132,16.842897923665));
#6420=CARTESIAN_POINT('Ctrl Pts',(3.18917573645277,-5.21545622975794,16.8506211266566));
#6421=CARTESIAN_POINT('Ctrl Pts',(3.33380274604764,-5.12701891391892,16.8583437332636));
#6422=CARTESIAN_POINT('Ctrl Pts',(3.47475730820949,-5.03255687782452,16.8660663398706));
#6423=CARTESIAN_POINT('Ctrl Pts',(3.6115431297739,-4.93240121890778,16.8737889464777));
#6424=CARTESIAN_POINT('Ctrl Pts',(3.64898571879469,-4.90498545949619,16.8759028672192));
#6425=CARTESIAN_POINT('Ctrl Pts',(3.68611611652612,-4.87714333293649,16.8780167879608));
#6426=CARTESIAN_POINT('Ctrl Pts',(3.72292453512041,-4.84888218750451,16.8801307087023));
#6427=CARTESIAN_POINT('',(-6.11329971010691,-2.18371950135767E-5,16.1147410325606));
#6428=CARTESIAN_POINT('Ctrl Pts',(-6.11376907689637,-2.18388716277662E-5,
16.1147410325606));
#6429=CARTESIAN_POINT('Ctrl Pts',(-6.11377325293236,-0.0206356155618927,
16.1156804505183));
#6430=CARTESIAN_POINT('Ctrl Pts',(-6.10863870970093,-1.05753985300389,16.1629346940117));
#6431=CARTESIAN_POINT('Ctrl Pts',(-5.5648651016231,-3.10533503802479,16.2565037630409));
#6432=CARTESIAN_POINT('Ctrl Pts',(-3.400970216456,-5.38926997694936,16.3954482396481));
#6433=CARTESIAN_POINT('Ctrl Pts',(-0.40809635818025,-6.35958227087845,16.5343927162552));
#6434=CARTESIAN_POINT('Ctrl Pts',(2.10807756387106,-5.88779407064529,16.6474487644803));
#6435=CARTESIAN_POINT('Ctrl Pts',(3.36702541840832,-5.12169796795855,16.7141899871697));
#6436=CARTESIAN_POINT('Ctrl Pts',(3.72262360719331,-4.84849058816218,16.7346163843234));
#6437=CARTESIAN_POINT('Ctrl Pts',(3.72292453512039,-4.84888218750452,14.984609455652));
#6438=CARTESIAN_POINT('Ctrl Pts',(3.84706716304671,-4.75356668642837,14.9917407949601));
#6439=CARTESIAN_POINT('Ctrl Pts',(3.96753323261942,-4.65349207330933,14.9988721342681));
#6440=CARTESIAN_POINT('Ctrl Pts',(4.08396494501409,-4.54896206737274,15.0060034735762));
#6441=CARTESIAN_POINT('Ctrl Pts',(4.21008533287738,-4.43573376710187,15.0137282356794));
#6442=CARTESIAN_POINT('Ctrl Pts',(4.33151625523934,-4.31723713512184,15.0214529977826));
#6443=CARTESIAN_POINT('Ctrl Pts',(4.44782645370979,-4.19388428550185,15.0291777598858));
#6444=CARTESIAN_POINT('Ctrl Pts',(4.56411396369235,-4.07055549817109,15.0369010151291));
#6445=CARTESIAN_POINT('Ctrl Pts',(4.67528252564377,-3.94237261384261,15.0446242703725));
#6446=CARTESIAN_POINT('Ctrl Pts',(4.78093846444182,-3.80978384711267,15.0523475256158));
#6447=CARTESIAN_POINT('Ctrl Pts',(4.88659848633455,-3.67718995646359,15.0600710793258));
#6448=CARTESIAN_POINT('Ctrl Pts',(4.98674525817353,-3.54019008808067,15.0677946330359));
#6449=CARTESIAN_POINT('Ctrl Pts',(5.08102556976984,-3.39926532089584,15.0755181867459));
#6450=CARTESIAN_POINT('Ctrl Pts',(5.17529954907249,-3.25835001885802,15.0832412217071));
#6451=CARTESIAN_POINT('Ctrl Pts',(5.26370768038889,-3.11351060899576,15.0909642566682));
#6452=CARTESIAN_POINT('Ctrl Pts',(5.34594015390214,-2.96525706025578,15.0986872916293));
#6453=CARTESIAN_POINT('Ctrl Pts',(5.42819448122435,-2.8169641121813,15.1064123790367));
#6454=CARTESIAN_POINT('Ctrl Pts',(5.5042697154448,-2.66525548845014,15.114137466444));
#6455=CARTESIAN_POINT('Ctrl Pts',(5.57390162030798,-2.51066650306807,15.1218625538514));
#6456=CARTESIAN_POINT('Ctrl Pts',(5.64326351601011,-2.35667696189673,15.1295576859621));
#6457=CARTESIAN_POINT('Ctrl Pts',(5.70623186484387,-2.19982965540261,15.1372528180727));
#6458=CARTESIAN_POINT('Ctrl Pts',(5.76259272283903,-2.04067407323725,15.1449479501834));
#6459=CARTESIAN_POINT('Ctrl Pts',(5.81917059748546,-1.88090566485343,15.1526727122866));
#6460=CARTESIAN_POINT('Ctrl Pts',(5.86911000608853,-1.71875457430929,15.1603974743898));
#6461=CARTESIAN_POINT('Ctrl Pts',(5.91222941682117,-1.55478901635378,15.168122236493));
#6462=CARTESIAN_POINT('Ctrl Pts',(5.95534041630324,-1.39085544295861,15.1758454917363));
#6463=CARTESIAN_POINT('Ctrl Pts',(5.99163399192148,-1.22510841471985,15.1835687469797));
#6464=CARTESIAN_POINT('Ctrl Pts',(6.02097888624547,-1.05812986626704,15.191292002223));
#6465=CARTESIAN_POINT('Ctrl Pts',(6.0503249146087,-0.891144864895214,15.199015555933));
#6466=CARTESIAN_POINT('Ctrl Pts',(6.07272166557029,-0.722928559523004,15.2067391096431));
#6467=CARTESIAN_POINT('Ctrl Pts',(6.08808913827344,-0.554072384203525,15.2144626633531));
#6468=CARTESIAN_POINT('Ctrl Pts',(6.10345557882736,-0.385227550031262,15.2221856983143));
#6469=CARTESIAN_POINT('Ctrl Pts',(6.11179365718794,-0.215743247568319,15.2299087332754));
#6470=CARTESIAN_POINT('Ctrl Pts',(6.11307530532601,-0.0462155159367491,
15.2376317682365));
#6471=CARTESIAN_POINT('Ctrl Pts',(6.11435729407032,0.123357268780197,15.2453568556439));
#6472=CARTESIAN_POINT('Ctrl Pts',(6.10857910072673,0.292973188604178,15.2530819430512));
#6473=CARTESIAN_POINT('Ctrl Pts',(6.09576480241753,0.462035751979778,15.2608070304586));
#6474=CARTESIAN_POINT('Ctrl Pts',(6.08300019365714,0.630442747466239,15.2685021625693));
#6475=CARTESIAN_POINT('Ctrl Pts',(6.06325400597843,0.798300361477343,15.2761972946799));
#6476=CARTESIAN_POINT('Ctrl Pts',(6.03660126151578,0.965023715753177,15.2838924267906));
#6477=CARTESIAN_POINT('Ctrl Pts',(6.00984589105432,1.13238903584166,15.2916171888938));
#6478=CARTESIAN_POINT('Ctrl Pts',(5.97612116543257,1.29867061503148,15.2993419509969));
#6479=CARTESIAN_POINT('Ctrl Pts',(5.93553952736822,1.46328263898312,15.3070667131001));
#6480=CARTESIAN_POINT('Ctrl Pts',(5.89496580551407,1.62786255226983,15.3147899683434));
#6481=CARTESIAN_POINT('Ctrl Pts',(5.84753791596166,1.79077325263618,15.3225132235868));
#6482=CARTESIAN_POINT('Ctrl Pts',(5.79341901268092,1.95144093069898,15.3302364788301));
#6483=CARTESIAN_POINT('Ctrl Pts',(5.73929801796461,2.1121148177955,15.3379600325402));
#6484=CARTESIAN_POINT('Ctrl Pts',(5.67848558950548,2.27054520753042,15.3456835862502));
#6485=CARTESIAN_POINT('Ctrl Pts',(5.61119443581084,2.42617447147263,15.3534071399603));
#6486=CARTESIAN_POINT('Ctrl Pts',(5.54390780169532,2.58179328264751,15.3611301749214));
#6487=CARTESIAN_POINT('Ctrl Pts',(5.4701434389292,2.73461105359685,15.3688532098825));
#6488=CARTESIAN_POINT('Ctrl Pts',(5.3901618627911,2.88409095824185,15.3765762448437));
#6489=CARTESIAN_POINT('Ctrl Pts',(5.31015903103472,3.03361058813293,15.384301332251));
#6490=CARTESIAN_POINT('Ctrl Pts',(5.22393583198312,3.1797902984944,15.3920264196584));
#6491=CARTESIAN_POINT('Ctrl Pts',(5.13179878739104,3.3221178137194,15.3997515070657));
#6492=CARTESIAN_POINT('Ctrl Pts',(5.04001901933984,3.46389343060063,15.4074466391764));
#6493=CARTESIAN_POINT('Ctrl Pts',(4.94237138475036,3.60184642972867,15.4151417712871));
#6494=CARTESIAN_POINT('Ctrl Pts',(4.83920158538215,3.73549910701835,15.4228369033977));
#6495=CARTESIAN_POINT('Ctrl Pts',(4.73563453222546,3.86966641196766,15.4305616655009));
#6496=CARTESIAN_POINT('Ctrl Pts',(4.6264659997075,3.99954771240799,15.4382864276041));
#6497=CARTESIAN_POINT('Ctrl Pts',(4.51207499742677,4.12468238535965,15.4460111897073));
#6498=CARTESIAN_POINT('Ctrl Pts',(4.39770630925843,4.24979264844428,15.4537344449506));
#6499=CARTESIAN_POINT('Ctrl Pts',(4.27811739778417,4.37015789780446,15.4614577001939));
#6500=CARTESIAN_POINT('Ctrl Pts',(4.15372605995467,4.48535231407227,15.4691809554373));
#6501=CARTESIAN_POINT('Ctrl Pts',(4.02932991499747,4.60055118205093,15.4769045091473));
#6502=CARTESIAN_POINT('Ctrl Pts',(3.900131202141,4.71057859882912,15.4846280628574));
#6503=CARTESIAN_POINT('Ctrl Pts',(3.76658349202819,4.81504666229526,15.4923516165674));
#6504=CARTESIAN_POINT('Ctrl Pts',(3.63304475158556,4.91950770921224,15.5000746515285));
#6505=CARTESIAN_POINT('Ctrl Pts',(3.49515784807595,5.01840995475133,15.5077976864897));
#6506=CARTESIAN_POINT('Ctrl Pts',(3.35340838006248,5.11140663604714,15.5155207214508));
#6507=CARTESIAN_POINT('Ctrl Pts',(3.21162124121586,5.20442803180935,15.5232458088582));
#6508=CARTESIAN_POINT('Ctrl Pts',(3.06596975064604,5.29154055140843,15.5309708962655));
#6509=CARTESIAN_POINT('Ctrl Pts',(2.91696816073999,5.37244100123297,15.5386959836729));
#6510=CARTESIAN_POINT('Ctrl Pts',(2.76854434899991,5.45302774626044,15.5463911157836));
#6511=CARTESIAN_POINT('Ctrl Pts',(2.61679666260055,5.52745039188512,15.5540862478942));
#6512=CARTESIAN_POINT('Ctrl Pts',(2.46225721888687,5.59545484751146,15.5617813800049));
#6513=CARTESIAN_POINT('Ctrl Pts',(2.30712272332804,5.66372115328962,15.5695061421081));
#6514=CARTESIAN_POINT('Ctrl Pts',(2.14911997242034,5.7255438950742,15.5772309042113));
#6515=CARTESIAN_POINT('Ctrl Pts',(1.98880215989118,5.78069991707857,15.5849556663144));
#6516=CARTESIAN_POINT('Ctrl Pts',(1.82851562036121,5.83584517986533,15.5926789215578));
#6517=CARTESIAN_POINT('Ctrl Pts',(1.66591521981019,5.88432621473104,15.6004021768011));
#6518=CARTESIAN_POINT('Ctrl Pts',(1.50157156108632,5.92596898485276,15.6081254320444));
#6519=CARTESIAN_POINT('Ctrl Pts',(1.33722155126887,5.96761336426765,15.6158489857544));
#6520=CARTESIAN_POINT('Ctrl Pts',(1.17112845470606,6.00241886844284,15.6235725394645));
#6521=CARTESIAN_POINT('Ctrl Pts',(1.00387614733472,6.03026187186862,15.6312960931745));
#6522=CARTESIAN_POINT('Ctrl Pts',(0.836635073387881,6.05810300523184,15.6390191281356));
#6523=CARTESIAN_POINT('Ctrl Pts',(0.668235257094541,6.0789825216141,15.6467421630968));
#6524=CARTESIAN_POINT('Ctrl Pts',(0.499269016725837,6.09282824404542,15.6544651980579));
#6525=CARTESIAN_POINT('Ctrl Pts',(0.330257872491124,6.1066776460666,15.6621902854652));
#6526=CARTESIAN_POINT('Ctrl Pts',(0.16068031929641,6.11348949079551,15.6699153728726));
#6527=CARTESIAN_POINT('Ctrl Pts',(-0.00886700772179213,6.11324356938884,
15.67764046028));
#6528=CARTESIAN_POINT('Ctrl Pts',(-0.177756887100845,6.11299860158287,15.6853355923907));
#6529=CARTESIAN_POINT('Ctrl Pts',(-0.346616462158736,6.10575053832936,15.6930307245014));
#6530=CARTESIAN_POINT('Ctrl Pts',(-0.514856902391781,6.09153083654343,15.7007258566121));
#6531=CARTESIAN_POINT('Ctrl Pts',(-0.683745149953988,6.07725638200589,15.7084506187153));
#6532=CARTESIAN_POINT('Ctrl Pts',(-0.852069297951079,6.0559514084714,15.7161753808185));
#6533=CARTESIAN_POINT('Ctrl Pts',(-1.01923680827505,6.0276846210761,15.7239001429217));
#6534=CARTESIAN_POINT('Ctrl Pts',(-1.18637170943766,5.99942334764837,15.731623398165));
#6535=CARTESIAN_POINT('Ctrl Pts',(-1.35235011082691,5.96420302292877,15.7393466534083));
#6536=CARTESIAN_POINT('Ctrl Pts',(-1.51658768688012,5.92214381373026,15.7470699086516));
#6537=CARTESIAN_POINT('Ctrl Pts',(-1.68083160992742,5.88008297914517,15.7547934623617));
#6538=CARTESIAN_POINT('Ctrl Pts',(-1.84333426502474,5.83118280600485,15.7625170160718));
#6539=CARTESIAN_POINT('Ctrl Pts',(-2.00352378941037,5.77561407884622,15.7702405697819));
#6540=CARTESIAN_POINT('Ctrl Pts',(-2.16370255474059,5.72004908393549,15.777963604743));
#6541=CARTESIAN_POINT('Ctrl Pts',(-2.32156820081101,5.65781653519248,15.7856866397042));
#6542=CARTESIAN_POINT('Ctrl Pts',(-2.47656606591191,5.58913643451952,15.7934096746653));
#6543=CARTESIAN_POINT('Ctrl Pts',(-2.63160512269235,5.52043808166809,15.8011347620727));
#6544=CARTESIAN_POINT('Ctrl Pts',(-2.78377458473753,5.44528887943016,15.80885984948));
#6545=CARTESIAN_POINT('Ctrl Pts',(-2.93254086265715,5.36395652959138,15.8165849368874));
#6546=CARTESIAN_POINT('Ctrl Pts',(-3.08073027487097,5.28293955931342,15.824280068998));
#6547=CARTESIAN_POINT('Ctrl Pts',(-3.22554259039452,5.19578748657979,15.8319752011087));
#6548=CARTESIAN_POINT('Ctrl Pts',(-3.36647579169918,5.10280964826274,15.8396703332193));
#6549=CARTESIAN_POINT('Ctrl Pts',(-3.50795165421478,5.00947380015195,15.8473950953225));
#6550=CARTESIAN_POINT('Ctrl Pts',(-3.64556856027343,4.91023415150679,15.8551198574257));
#6551=CARTESIAN_POINT('Ctrl Pts',(-3.77883905724067,4.80543452166112,15.8628446195289));
#6552=CARTESIAN_POINT('Ctrl Pts',(-3.91208355729635,4.70065533495006,15.8705678747723));
#6553=CARTESIAN_POINT('Ctrl Pts',(-4.04098309104772,4.59031852694703,15.8782911300157));
#6554=CARTESIAN_POINT('Ctrl Pts',(-4.16508203828198,4.47480917770589,15.8860143852591));
#6555=CARTESIAN_POINT('Ctrl Pts',(-4.28918578134367,4.35929536458396,15.8937379389692));
#6556=CARTESIAN_POINT('Ctrl Pts',(-4.40848833197411,4.2386088232472,15.9014614926792));
#6557=CARTESIAN_POINT('Ctrl Pts',(-4.52256923087092,4.11317311992573,15.9091850463893));
#6558=CARTESIAN_POINT('Ctrl Pts',(-4.63664246757641,3.98774584143584,15.9169080813504));
#6559=CARTESIAN_POINT('Ctrl Pts',(-4.74549454112277,3.85757027377182,15.9246311163115));
#6560=CARTESIAN_POINT('Ctrl Pts',(-4.84874364392741,3.72310497273089,15.9323541512726));
#6561=CARTESIAN_POINT('Ctrl Pts',(-4.95202018584586,3.58860393667051,15.94007923868));
#6562=CARTESIAN_POINT('Ctrl Pts',(-5.04969058670783,3.44981113940905,15.9478043260874));
#6563=CARTESIAN_POINT('Ctrl Pts',(-5.14141436410374,3.30721694164259,15.9555294134948));
#6564=CARTESIAN_POINT('Ctrl Pts',(-5.23278246746901,3.16517567632729,15.9632245456053));
#6565=CARTESIAN_POINT('Ctrl Pts',(-5.31824984162882,3.01936271921126,15.9709196777159));
#6566=CARTESIAN_POINT('Ctrl Pts',(-5.39752364769265,2.87028988694499,15.9786148098265));
#6567=CARTESIAN_POINT('Ctrl Pts',(-5.4770292568796,2.72078115346736,15.9863324431357));
#6568=CARTESIAN_POINT('Ctrl Pts',(-5.55033365351206,2.56793952772914,15.9940500764449));
#6569=CARTESIAN_POINT('Ctrl Pts',(-5.6171735517017,2.41229908024748,16.0017677097541));
#6570=CARTESIAN_POINT('Ctrl Pts',(-5.68400019521871,2.25668949701362,16.0094838126196));
#6571=CARTESIAN_POINT('Ctrl Pts',(-5.74436477270071,2.09828249158631,16.0171999154851));
#6572=CARTESIAN_POINT('Ctrl Pts',(-5.79805168318064,1.93763315456412,16.0249160183505));
#6573=CARTESIAN_POINT('Ctrl Pts',(-5.85174033065206,1.77697861987778,16.0326323708635));
#6574=CARTESIAN_POINT('Ctrl Pts',(-5.8987507742332,1.61408190886903,16.0403487233766));
#6575=CARTESIAN_POINT('Ctrl Pts',(-5.93891670190994,1.44951508107891,16.0480650758896));
#6576=CARTESIAN_POINT('Ctrl Pts',(-5.97908014906332,1.28495841642665,16.0557809518645));
#6577=CARTESIAN_POINT('Ctrl Pts',(-6.01239985098338,1.11873215051005,16.0634968278395));
#6578=CARTESIAN_POINT('Ctrl Pts',(-6.03876017516021,0.95142057440389,16.0712127038145));
#6579=CARTESIAN_POINT('Ctrl Pts',(-6.0651272466124,0.784066172675864,16.0789305547705));
#6580=CARTESIAN_POINT('Ctrl Pts',(-6.08453132973179,0.615626219838155,16.0866484057265));
#6581=CARTESIAN_POINT('Ctrl Pts',(-6.09690830023527,0.446693117276577,16.0943662566825));
#6582=CARTESIAN_POINT('Ctrl Pts',(-6.10779984683707,0.298034545405651,16.1011578486418));
#6583=CARTESIAN_POINT('Ctrl Pts',(-6.11325053225869,0.148994340849137,16.1079494406012));
#6584=CARTESIAN_POINT('Ctrl Pts',(-6.113249999961,-2.1837017445121E-5,16.1147410325606));
#6585=CARTESIAN_POINT('Origin',(0.,0.,-3.86474103256053));
#6586=CARTESIAN_POINT('',(3.72288481551393,-4.8488307603735,13.2346211120867));
#6587=CARTESIAN_POINT('',(3.72270802987534,-4.84860079634452,13.3801373157199));
#6588=CARTESIAN_POINT('',(3.72292453512038,-4.84888218750453,-3.86474103256053));
#6589=CARTESIAN_POINT('',(-6.11319871911702,9.79097444517703E-6,14.5102589673365));
#6590=CARTESIAN_POINT('Ctrl Pts',(3.72270802987534,-4.84860079634452,13.3801373157199));
#6591=CARTESIAN_POINT('Ctrl Pts',(4.24171171221953,-4.44951091176983,13.4099614103007));
#6592=CARTESIAN_POINT('Ctrl Pts',(5.40481509300789,-3.21922256216121,13.4861003304172));
#6593=CARTESIAN_POINT('Ctrl Pts',(6.34339259002546,-0.610081612305798,13.6085540760694));
#6594=CARTESIAN_POINT('Ctrl Pts',(5.86217951430019,2.49913594407806,13.7474985526766));
#6595=CARTESIAN_POINT('Ctrl Pts',(3.9520731391245,4.99919463792661,13.8864430292838));
#6596=CARTESIAN_POINT('Ctrl Pts',(1.07865767154433,6.28071068848758,14.025387505891));
#6597=CARTESIAN_POINT('Ctrl Pts',(-2.05767821932051,6.03131739096838,14.1643319824981));
#6598=CARTESIAN_POINT('Ctrl Pts',(-4.69245959230686,4.31180381040591,14.3032764591053));
#6599=CARTESIAN_POINT('Ctrl Pts',(-5.92983339331411,2.01258115915036,14.4185854537362));
#6600=CARTESIAN_POINT('Ctrl Pts',(-6.11275550933371,0.497909914167423,14.4875796228312));
#6601=CARTESIAN_POINT('Ctrl Pts',(-6.11272776669357,9.81098628248876E-6,
14.5102589663906));
#6602=CARTESIAN_POINT('Ctrl Pts',(-6.11324999999216,9.78879540440889E-6,
14.5102589674395));
#6603=CARTESIAN_POINT('Ctrl Pts',(-6.11325027459207,-0.171481984661658,
14.5180697483018));
#6604=CARTESIAN_POINT('Ctrl Pts',(-6.10603005521547,-0.342959526338876,
14.5258805291642));
#6605=CARTESIAN_POINT('Ctrl Pts',(-6.0916189476117,-0.513813350934067,14.5336913100265));
#6606=CARTESIAN_POINT('Ctrl Pts',(-6.0770204414231,-0.686888917662023,14.5416036604087));
#6607=CARTESIAN_POINT('Ctrl Pts',(-6.05504273155774,-0.859324115509616,
14.5495160107909));
#6608=CARTESIAN_POINT('Ctrl Pts',(-6.02577085604886,-1.0304907340157,14.5574283611731));
#6609=CARTESIAN_POINT('Ctrl Pts',(-5.99649898053998,-1.20165735252176,14.5653407115553));
#6610=CARTESIAN_POINT('Ctrl Pts',(-5.95993300206572,-1.37155507669805,14.5732530619375));
#6611=CARTESIAN_POINT('Ctrl Pts',(-5.91621184517902,-1.53956583667718,14.5811654123197));
#6612=CARTESIAN_POINT('Ctrl Pts',(-5.873527242057,-1.70359334922727,14.5888901744229));
#6613=CARTESIAN_POINT('Ctrl Pts',(-5.82400936005968,-1.86587366244741,14.5966149365261));
#6614=CARTESIAN_POINT('Ctrl Pts',(-5.76782631097592,-2.02583444755831,14.6043396986293));
#6615=CARTESIAN_POINT('Ctrl Pts',(-5.71165422145075,-2.18576402931476,14.6120629538727));
#6616=CARTESIAN_POINT('Ctrl Pts',(-5.64881966409654,-2.3433746869595,14.619786209116));
#6617=CARTESIAN_POINT('Ctrl Pts',(-5.57954007672257,-2.49811090521352,14.6275094643593));
#6618=CARTESIAN_POINT('Ctrl Pts',(-5.51025781202523,-2.65285310327934,14.6352330180694));
#6619=CARTESIAN_POINT('Ctrl Pts',(-5.43453014479446,-2.80472034880149,14.6429565717794));
#6620=CARTESIAN_POINT('Ctrl Pts',(-5.35262228694381,-2.95317798579977,14.6506801254895));
#6621=CARTESIAN_POINT('Ctrl Pts',(-5.27071993039675,-3.10162565170919,14.6584031604506));
#6622=CARTESIAN_POINT('Ctrl Pts',(-5.18263836701313,-3.24666388985333,14.6661261954117));
#6623=CARTESIAN_POINT('Ctrl Pts',(-5.0886883998481,-3.38778333601064,14.6738492303728));
#6624=CARTESIAN_POINT('Ctrl Pts',(-4.99471346487469,-3.52894028556893,14.6815743177802));
#6625=CARTESIAN_POINT('Ctrl Pts',(-4.89486718366908,-3.66617609687749,14.6892994051876));
#6626=CARTESIAN_POINT('Ctrl Pts',(-4.78950379893765,-3.79901025564051,14.6970244925949));
#6627=CARTESIAN_POINT('Ctrl Pts',(-4.68454897805601,-3.93132932811027,14.7047196247056));
#6628=CARTESIAN_POINT('Ctrl Pts',(-4.57411998380422,-4.05928059906078,14.7124147568162));
#6629=CARTESIAN_POINT('Ctrl Pts',(-4.45860674238751,-4.18242172422111,14.7201098889269));
#6630=CARTESIAN_POINT('Ctrl Pts',(-4.3426487189408,-4.30603700246513,14.7278346510301));
#6631=CARTESIAN_POINT('Ctrl Pts',(-4.22152612618802,-4.42484877890641,14.7355594131333));
#6632=CARTESIAN_POINT('Ctrl Pts',(-4.09566040630592,-4.53843490629953,14.7432841752365));
#6633=CARTESIAN_POINT('Ctrl Pts',(-3.96981923889555,-4.65199887658597,14.7510074304798));
#6634=CARTESIAN_POINT('Ctrl Pts',(-3.83923702567417,-4.76033901961392,14.7587306857232));
#6635=CARTESIAN_POINT('Ctrl Pts',(-3.70437047921442,-4.86307155152222,14.7664539409665));
#6636=CARTESIAN_POINT('Ctrl Pts',(-3.56949872081038,-4.96580805354948,14.7741774946765));
#6637=CARTESIAN_POINT('Ctrl Pts',(-3.43034254756137,-5.06293631562267,14.7819010483866));
#6638=CARTESIAN_POINT('Ctrl Pts',(-3.2873906440296,-5.15411372750414,14.7896246020966));
#6639=CARTESIAN_POINT('Ctrl Pts',(-3.1444483417965,-5.24528501549679,14.7973476370577));
#6640=CARTESIAN_POINT('Ctrl Pts',(-2.99771108668624,-5.33050608269726,14.8050706720189));
#6641=CARTESIAN_POINT('Ctrl Pts',(-2.84769549771557,-5.4094783403569,14.81279370698));
#6642=CARTESIAN_POINT('Ctrl Pts',(-2.69764004113689,-5.48847158540215,14.8205187943874));
#6643=CARTESIAN_POINT('Ctrl Pts',(-2.54430478937575,-5.56121255283737,14.8282438817947));
#6644=CARTESIAN_POINT('Ctrl Pts',(-2.38823070429244,-5.62744877058644,14.8359689692021));
#6645=CARTESIAN_POINT('Ctrl Pts',(-2.23276182213772,-5.69342814650979,14.8436641013128));
#6646=CARTESIAN_POINT('Ctrl Pts',(-2.0745756094302,-5.75295303725884,14.8513592334234));
#6647=CARTESIAN_POINT('Ctrl Pts',(-1.91422610098583,-5.8058215608822,14.8590543655341));
#6648=CARTESIAN_POINT('Ctrl Pts',(-1.75325916912747,-5.85889365397492,14.8667791276373));
#6649=CARTESIAN_POINT('Ctrl Pts',(-1.59005522988538,-5.90527678573933,14.8745038897405));
#6650=CARTESIAN_POINT('Ctrl Pts',(-1.42518633022512,-5.94480188792187,14.8822286518438));
#6651=CARTESIAN_POINT('Ctrl Pts',(-1.26034959133956,-5.98431927999105,14.8899519070871));
#6652=CARTESIAN_POINT('Ctrl Pts',(-1.09384884809832,-6.01698123800301,14.8976751623304));
#6653=CARTESIAN_POINT('Ctrl Pts',(-0.926268765157316,-6.04266925598232,
14.9053984175737));
#6654=CARTESIAN_POINT('Ctrl Pts',(-0.758682206050966,-6.06835826668016,
14.9131219712838));
#6655=CARTESIAN_POINT('Ctrl Pts',(-0.590016536436749,-6.08707274610645,
14.9208455249938));
#6656=CARTESIAN_POINT('Ctrl Pts',(-0.420864797743603,-6.09874564025425,
14.9285690787038));
#6657=CARTESIAN_POINT('Ctrl Pts',(-0.251724420048848,-6.11041775039751,
14.936292113665));
#6658=CARTESIAN_POINT('Ctrl Pts',(-0.0820983548121702,-6.11504919988803,
14.9440151486261));
#6659=CARTESIAN_POINT('Ctrl Pts',(0.0874168877315281,-6.11262495579758,
14.9517381835872));
#6660=CARTESIAN_POINT('Ctrl Pts',(0.256977180041634,-6.11020006744866,14.9594632709946));
#6661=CARTESIAN_POINT('Ctrl Pts',(0.426426273658079,-6.10071574097748,14.9671883584019));
#6662=CARTESIAN_POINT('Ctrl Pts',(0.595168345824421,-6.0842090860381,14.9749134458093));
#6663=CARTESIAN_POINT('Ctrl Pts',(0.763256092859132,-6.0677664383675,14.9826085779199));
#6664=CARTESIAN_POINT('Ctrl Pts',(0.930641984313115,-6.04435588836248,14.9903037100306));
#6665=CARTESIAN_POINT('Ctrl Pts',(1.09674292152156,-6.01406522467061,14.9979988421413));
#6666=CARTESIAN_POINT('Ctrl Pts',(1.26348285838097,-5.98365803109124,15.0057235778581));
#6667=CARTESIAN_POINT('Ctrl Pts',(1.4289869835453,-5.94630688366497,15.013448313575));
#6668=CARTESIAN_POINT('Ctrl Pts',(1.59267208640143,-5.90213700177298,15.0211730492918));
#6669=CARTESIAN_POINT('Ctrl Pts',(1.75632506302105,-5.8579757890393,15.0288962688861));
#6670=CARTESIAN_POINT('Ctrl Pts',(1.91815942393135,-5.80699859479505,15.0366194884803));
#6671=CARTESIAN_POINT('Ctrl Pts',(2.07760507091788,-5.74938107380232,15.0443427080746));
#6672=CARTESIAN_POINT('Ctrl Pts',(2.23705274244332,-5.69176282121914,15.0520660257333));
#6673=CARTESIAN_POINT('Ctrl Pts',(2.39411133999764,-5.62750417717528,15.0597893433921));
#6674=CARTESIAN_POINT('Ctrl Pts',(2.54822806804752,-5.55682996642104,15.0675126610508));
#6675=CARTESIAN_POINT('Ctrl Pts',(2.70233483408483,-5.48616032400525,15.075235479479));
#6676=CARTESIAN_POINT('Ctrl Pts',(2.85349982309663,-5.40907607686579,15.0829582979071));
#6677=CARTESIAN_POINT('Ctrl Pts',(3.0011920750816,-5.3258493868084,15.0906811163352));
#6678=CARTESIAN_POINT('Ctrl Pts',(3.14891480881972,-5.24260551984844,15.0984055286523));
#6679=CARTESIAN_POINT('Ctrl Pts',(3.29316309677674,-5.15321683176344,15.1061299409694));
#6680=CARTESIAN_POINT('Ctrl Pts',(3.433431615175,-5.05800088042863,15.1138543532864));
#6681=CARTESIAN_POINT('Ctrl Pts',(3.53194728744746,-4.9911272614304,15.1192794884559));
#6682=CARTESIAN_POINT('Ctrl Pts',(3.62850037180794,-4.92138014078745,15.1247046236253));
#6683=CARTESIAN_POINT('Ctrl Pts',(3.7229245351204,-4.84888218750451,15.1301297587947));
#6684=CARTESIAN_POINT('',(-6.11324999916302,0.000101159726426482,14.3647410325606));
#6685=CARTESIAN_POINT('Ctrl Pts',(-6.11324999916302,0.000101159726426482,
14.3647410325606));
#6686=CARTESIAN_POINT('Ctrl Pts',(-6.11325281292563,-0.169939180116824,
14.3724862375428));
#6687=CARTESIAN_POINT('Ctrl Pts',(-6.10615676234947,-0.339980975408143,
14.3802314425249));
#6688=CARTESIAN_POINT('Ctrl Pts',(-6.09198753638617,-0.509424596005636,
14.3879766475071));
#6689=CARTESIAN_POINT('Ctrl Pts',(-6.07781849764592,-0.67886597768408,14.3957217501491));
#6690=CARTESIAN_POINT('Ctrl Pts',(-6.05657649931014,-0.847708888657797,
14.4034668527911));
#6691=CARTESIAN_POINT('Ctrl Pts',(-6.02833915632798,-1.01535834993506,14.4112119554332));
#6692=CARTESIAN_POINT('Ctrl Pts',(-6.00009448276363,-1.18305133400965,14.4189590687499));
#6693=CARTESIAN_POINT('Ctrl Pts',(-5.96485088767088,-1.34954994037174,14.4267061820666));
#6694=CARTESIAN_POINT('Ctrl Pts',(-5.92273736991832,-1.51426801111066,14.4344532953833));
#6695=CARTESIAN_POINT('Ctrl Pts',(-5.89415787113032,-1.6260506442002,14.4397107193047));
#6696=CARTESIAN_POINT('Ctrl Pts',(-5.8624155724781,-1.73701346732266,14.4449681432261));
#6697=CARTESIAN_POINT('Ctrl Pts',(-5.82756400566072,-1.84697680614231,14.4502255671475));
#6698=CARTESIAN_POINT('Ctrl Pts',(-5.77635640539604,-2.00854654926322,14.4579503292507));
#6699=CARTESIAN_POINT('Ctrl Pts',(-5.71841629279437,-2.16801398809637,14.4656750913539));
#6700=CARTESIAN_POINT('Ctrl Pts',(-5.65394149203249,-2.32481637278591,14.4733998534571));
#6701=CARTESIAN_POINT('Ctrl Pts',(-5.58947926829106,-2.48158817022624,14.4811231087004));
#6702=CARTESIAN_POINT('Ctrl Pts',(-5.51848502035082,-2.6356956579108,14.4888463639437));
#6703=CARTESIAN_POINT('Ctrl Pts',(-5.44120495122343,-2.78659545705537,14.496569619187));
#6704=CARTESIAN_POINT('Ctrl Pts',(-5.36392189559249,-2.93750108775251,14.504293172897));
#6705=CARTESIAN_POINT('Ctrl Pts',(-5.2803526736176,-3.08519849797062,14.5120167266071));
#6706=CARTESIAN_POINT('Ctrl Pts',(-5.19079010568986,-3.22916763906309,14.5197402803171));
#6707=CARTESIAN_POINT('Ctrl Pts',(-5.10123355319063,-3.37312711053468,14.5274633152782));
#6708=CARTESIAN_POINT('Ctrl Pts',(-5.00568462771779,-3.51335854486044,14.5351863502394));
#6709=CARTESIAN_POINT('Ctrl Pts',(-4.90448035517501,-3.64936953571468,14.5429093852005));
#6710=CARTESIAN_POINT('Ctrl Pts',(-4.80324918694549,-3.78541667236505,14.5506344726078));
#6711=CARTESIAN_POINT('Ctrl Pts',(-4.69635985597466,-3.91724086855353,14.5583595600152));
#6712=CARTESIAN_POINT('Ctrl Pts',(-4.58419125898163,-4.04438080100977,14.5660846474226));
#6713=CARTESIAN_POINT('Ctrl Pts',(-4.47245761416772,-4.17102772747184,14.5737797795333));
#6714=CARTESIAN_POINT('Ctrl Pts',(-4.35548580370585,-4.29302644085327,14.5814749116439));
#6715=CARTESIAN_POINT('Ctrl Pts',(-4.23368836199903,-4.40995560249465,14.5891700437546));
#6716=CARTESIAN_POINT('Ctrl Pts',(-4.11142194104218,-4.52733499814559,14.5968948058578));
#6717=CARTESIAN_POINT('Ctrl Pts',(-3.98424932910431,-4.63964727471922,14.604619567961));
#6718=CARTESIAN_POINT('Ctrl Pts',(-3.8526134767485,-4.74649291174819,14.6123443300642));
#6719=CARTESIAN_POINT('Ctrl Pts',(-3.72100330243681,-4.85331770652992,14.6200675853075));
#6720=CARTESIAN_POINT('Ctrl Pts',(-3.5849318708643,-4.95467778995039,14.6277908405509));
#6721=CARTESIAN_POINT('Ctrl Pts',(-3.44487534762473,-5.05021379763544,14.6355140957942));
#6722=CARTESIAN_POINT('Ctrl Pts',(-3.30481341187349,-5.14575349732815,14.6432376495042));
#6723=CARTESIAN_POINT('Ctrl Pts',(-3.16076633585919,-5.23546848904279,14.6509612032143));
#6724=CARTESIAN_POINT('Ctrl Pts',(-3.01324005929328,-5.31904219832577,14.6586847569243));
#6725=CARTESIAN_POINT('Ctrl Pts',(-2.86572369126158,-5.40261029441918,14.6664077918855));
#6726=CARTESIAN_POINT('Ctrl Pts',(-2.71472886609083,-5.48003777729016,14.6741308268466));
#6727=CARTESIAN_POINT('Ctrl Pts',(-2.56078711661227,-5.55105349513879,14.6818538618077));
#6728=CARTESIAN_POINT('Ctrl Pts',(-2.40680445612331,-5.62208808587137,14.6895789492151));
#6729=CARTESIAN_POINT('Ctrl Pts',(-2.24987359344524,-5.68670737180964,14.6973040366224));
#6730=CARTESIAN_POINT('Ctrl Pts',(-2.09054795822268,-5.74468752821866,14.7050291240298));
#6731=CARTESIAN_POINT('Ctrl Pts',(-1.93184013434901,-5.80244285703738,14.7127242561405));
#6732=CARTESIAN_POINT('Ctrl Pts',(-1.77075638155635,-5.85361037696616,14.7204193882511));
#6733=CARTESIAN_POINT('Ctrl Pts',(-1.60786053781036,-5.89801746805248,14.7281145203618));
#6734=CARTESIAN_POINT('Ctrl Pts',(-1.44433746602451,-5.94259554798699,14.735839282465));
#6735=CARTESIAN_POINT('Ctrl Pts',(-1.27893039782108,-5.9803767931299,14.7435640445682));
#6736=CARTESIAN_POINT('Ctrl Pts',(-1.11221944192877,-6.01122229463323,14.7512888066714));
#6737=CARTESIAN_POINT('Ctrl Pts',(-0.945541006138027,-6.04206177914244,
14.7590120619147));
#6738=CARTESIAN_POINT('Ctrl Pts',(-0.777559501621107,-6.06596816200061,
14.766735317158));
#6739=CARTESIAN_POINT('Ctrl Pts',(-0.608864992242848,-6.08285368751552,
14.7744585724014));
#6740=CARTESIAN_POINT('Ctrl Pts',(-0.440163963631982,-6.09973986557489,
14.7821821261114));
#6741=CARTESIAN_POINT('Ctrl Pts',(-0.270750189969728,-6.10960460785247,
14.7899056798215));
#6742=CARTESIAN_POINT('Ctrl Pts',(-0.101219408601492,-6.11241197841101,
14.7976292335315));
#6743=CARTESIAN_POINT('Ctrl Pts',(0.0682999863096924,-6.11521916041379,
14.8053522684926));
#6744=CARTESIAN_POINT('Ctrl Pts',(0.237936056286156,-6.11096991401799,14.8130753034537));
#6745=CARTESIAN_POINT('Ctrl Pts',(0.407092321521854,-6.0996804346013,14.8207983384149));
#6746=CARTESIAN_POINT('Ctrl Pts',(0.576293541123662,-6.08838795493281,14.8285234258222));
#6747=CARTESIAN_POINT('Ctrl Pts',(0.74501438459519,-6.07005152250148,14.8362485132296));
#6748=CARTESIAN_POINT('Ctrl Pts',(0.912661786618967,-6.04473936789217,14.8439736006369));
#6749=CARTESIAN_POINT('Ctrl Pts',(1.07965910827491,-6.01952536532448,14.8516687327476));
#6750=CARTESIAN_POINT('Ctrl Pts',(1.24559099469841,-5.98738972191345,14.8593638648583));
#6751=CARTESIAN_POINT('Ctrl Pts',(1.40987973861898,-5.94845061214529,14.867058996969));
#6752=CARTESIAN_POINT('Ctrl Pts',(1.57479970578628,-5.90936189218044,14.87478369499));
#6753=CARTESIAN_POINT('Ctrl Pts',(1.73812228136712,-5.86340344921617,14.8825083930111));
#6754=CARTESIAN_POINT('Ctrl Pts',(1.89927161296279,-5.8107308406683,14.8902330910321));
#6755=CARTESIAN_POINT('Ctrl Pts',(2.06334154419179,-5.75710361692166,14.8980977880838));
#6756=CARTESIAN_POINT('Ctrl Pts',(2.2251583716967,-5.69651659285686,14.9059624851354));
#6757=CARTESIAN_POINT('Ctrl Pts',(2.38413079366924,-5.62918696804237,14.9138271821871));
#6758=CARTESIAN_POINT('Ctrl Pts',(2.54023647548796,-5.56307149431523,14.9215500556284));
#6759=CARTESIAN_POINT('Ctrl Pts',(2.69359917291047,-5.49045467698622,14.9292729290696));
#6760=CARTESIAN_POINT('Ctrl Pts',(2.84367910684593,-5.41159077349608,14.9369958025109));
#6761=CARTESIAN_POINT('Ctrl Pts',(2.99789316486852,-5.33055447324061,14.9449314113678));
#6762=CARTESIAN_POINT('Ctrl Pts',(3.14864068572877,-5.24292211613975,14.9528670202246));
#6763=CARTESIAN_POINT('Ctrl Pts',(3.29536275830877,-5.14902028095167,14.9608026290815));
#6764=CARTESIAN_POINT('Ctrl Pts',(3.44208483088875,-5.0551184457636,14.9687382379383));
#6765=CARTESIAN_POINT('Ctrl Pts',(3.58478115207154,-4.95494733205319,14.9766738467952));
#6766=CARTESIAN_POINT('Ctrl Pts',(3.72292453512039,-4.84888218750452,14.984609455652));
#6767=CARTESIAN_POINT('Ctrl Pts',(3.72288481551393,-4.8488307603735,13.2346211120867));
#6768=CARTESIAN_POINT('Ctrl Pts',(4.32622015324387,-4.38460469236938,13.2693039928211));
#6769=CARTESIAN_POINT('Ctrl Pts',(5.53405973259451,-3.03738285194378,13.3503016990913));
#6770=CARTESIAN_POINT('Ctrl Pts',(6.36662318807926,-0.277377862609176,13.4776142308971));
#6771=CARTESIAN_POINT('Ctrl Pts',(5.72340370477089,2.80240598947921,13.6165587075043));
#6772=CARTESIAN_POINT('Ctrl Pts',(3.68511721884909,5.19910957578276,13.7555031841115));
#6773=CARTESIAN_POINT('Ctrl Pts',(0.748591556037913,6.32854169456779,13.8944476607187));
#6774=CARTESIAN_POINT('Ctrl Pts',(-2.3704016439475,5.9154057632613,14.0333921373259));
#6775=CARTESIAN_POINT('Ctrl Pts',(-4.91161468251336,4.06040275196602,14.1723366139331));
#6776=CARTESIAN_POINT('Ctrl Pts',(-5.98000021356576,1.79908250121632,14.2827862424113));
#6777=CARTESIAN_POINT('Ctrl Pts',(-6.11306665977086,0.391299537207678,14.3469210453537));
#6778=CARTESIAN_POINT('Ctrl Pts',(-6.11283634071177,0.000101368021089277,
14.3647410227605));
#6779=CARTESIAN_POINT('Origin',(0.,0.,-3.86474103256053));
#6780=CARTESIAN_POINT('',(3.72292453512038,-4.84888218750453,11.484610425966));
#6781=CARTESIAN_POINT('',(3.72292453512038,-4.84888218750453,11.6301271545495));
#6782=CARTESIAN_POINT('',(3.72292453512038,-4.84888218750453,-3.86474103256053));
#6783=CARTESIAN_POINT('',(-6.11324999912966,-0.000103156033837302,12.7602589674395));
#6784=CARTESIAN_POINT('Ctrl Pts',(3.72292453512038,-4.84888218750453,11.6301271545495));
#6785=CARTESIAN_POINT('Ctrl Pts',(3.8574118287249,-4.74562415283574,11.6378518926703));
#6786=CARTESIAN_POINT('Ctrl Pts',(3.98758795371617,-4.63677720859856,11.6455766307911));
#6787=CARTESIAN_POINT('Ctrl Pts',(4.11299847765816,-4.52272805785199,11.6533013689119));
#6788=CARTESIAN_POINT('Ctrl Pts',(4.16727742242853,-4.47336643045504,11.6566447137975));
#6789=CARTESIAN_POINT('Ctrl Pts',(4.22066408427948,-4.42303080373098,11.6599880586832));
#6790=CARTESIAN_POINT('Ctrl Pts',(4.27312366791289,-4.37175475995883,11.6633314035688));
#6791=CARTESIAN_POINT('Ctrl Pts',(4.39433096702921,-4.2532820168577,11.671056165672));
#6792=CARTESIAN_POINT('Ctrl Pts',(4.51062969223976,-4.1297444630101,11.6787809277752));
#6793=CARTESIAN_POINT('Ctrl Pts',(4.62160644222549,-4.00157212301363,11.6865056898784));
#6794=CARTESIAN_POINT('Ctrl Pts',(4.73256154411224,-3.87342478543887,11.6942289451217));
#6795=CARTESIAN_POINT('Ctrl Pts',(4.83819653493191,-3.74064470517301,11.701952200365));
#6796=CARTESIAN_POINT('Ctrl Pts',(4.93813709314584,-3.60369638174432,11.7096754556083));
#6797=CARTESIAN_POINT('Ctrl Pts',(5.03808151358274,-3.46674276592013,11.7173990093183));
#6798=CARTESIAN_POINT('Ctrl Pts',(5.13233087103584,-3.32562083826061,11.7251225630284));
#6799=CARTESIAN_POINT('Ctrl Pts',(5.22055266564044,-3.18082621778909,11.7328461167384));
#6800=CARTESIAN_POINT('Ctrl Pts',(5.30876853486909,-3.03604132238117,11.7405691516996));
#6801=CARTESIAN_POINT('Ctrl Pts',(5.39095748648467,-2.8875844984743,11.7482921866607));
#6802=CARTESIAN_POINT('Ctrl Pts',(5.46683160662606,-2.73597838940558,11.7560152216218));
#6803=CARTESIAN_POINT('Ctrl Pts',(5.54272589080293,-2.58433199003818,11.7637403090292));
#6804=CARTESIAN_POINT('Ctrl Pts',(5.61230184615108,-2.42953491573295,11.7714653964366));
#6805=CARTESIAN_POINT('Ctrl Pts',(5.67531816577891,-2.27213320025035,11.7791904838439));
#6806=CARTESIAN_POINT('Ctrl Pts',(5.73809012926561,-2.11534183580111,11.7868856159546));
#6807=CARTESIAN_POINT('Ctrl Pts',(5.79435315262763,-1.95596629592201,11.7945807480653));
#6808=CARTESIAN_POINT('Ctrl Pts',(5.84391677695614,-1.79456464539747,11.802275880176));
#6809=CARTESIAN_POINT('Ctrl Pts',(5.89367124528793,-1.63254152020196,11.8100006422792));
#6810=CARTESIAN_POINT('Ctrl Pts',(5.93669221314727,-1.46841925778513,11.8177254043824));
#6811=CARTESIAN_POINT('Ctrl Pts',(5.972822398388,-1.30277325725339,11.8254501664856));
#6812=CARTESIAN_POINT('Ctrl Pts',(6.00894553575759,-1.13715956908482,11.8331734217289));
#6813=CARTESIAN_POINT('Ctrl Pts',(6.03818050512413,-0.970023045347367,11.8408966769722));
#6814=CARTESIAN_POINT('Ctrl Pts',(6.06042083513189,-0.801950661574166,11.8486199322155));
#6815=CARTESIAN_POINT('Ctrl Pts',(6.08266202462166,-0.633871782610093,11.8563434859256));
#6816=CARTESIAN_POINT('Ctrl Pts',(6.09790798834629,-0.464857284898449,11.8640670396356));
#6817=CARTESIAN_POINT('Ctrl Pts',(6.10610386813031,-0.295501462101399,11.8717905933457));
#6818=CARTESIAN_POINT('Ctrl Pts',(6.11429919744185,-0.126157014009869,11.8795136283068));
#6819=CARTESIAN_POINT('Ctrl Pts',(6.11544537508058,0.0435283967033413,11.8872366632679));
#6820=CARTESIAN_POINT('Ctrl Pts',(6.10953962422672,0.212958076868715,11.894959698229));
#6821=CARTESIAN_POINT('Ctrl Pts',(6.10363230388156,0.382432784061904,11.9026847856364));
#6822=CARTESIAN_POINT('Ctrl Pts',(6.09066931901598,0.551651307869135,11.9104098730438));
#6823=CARTESIAN_POINT('Ctrl Pts',(6.07070001026945,0.720018713516863,11.9181349604511));
#6824=CARTESIAN_POINT('Ctrl Pts',(6.0508081358012,0.887733246863995,11.9258300925618));
#6825=CARTESIAN_POINT('Ctrl Pts',(6.02396424599014,1.05460294480008,11.9335252246725));
#6826=CARTESIAN_POINT('Ctrl Pts',(5.9902680884105,1.22004663495739,11.9412203567832));
#6827=CARTESIAN_POINT('Ctrl Pts',(5.95644218427393,1.38612736359938,11.9489451188864));
#6828=CARTESIAN_POINT('Ctrl Pts',(5.91569912895541,1.55082989587953,11.9566698809895));
#6829=CARTESIAN_POINT('Ctrl Pts',(5.86817609665716,1.71357371044303,11.9643946430927));
#6830=CARTESIAN_POINT('Ctrl Pts',(5.82066233461842,1.87628577877065,11.9721178983361));
#6831=CARTESIAN_POINT('Ctrl Pts',(5.76637132336642,2.03703958774093,11.9798411535794));
#6832=CARTESIAN_POINT('Ctrl Pts',(5.70549039388603,2.19526875980466,11.9875644088227));
#6833=CARTESIAN_POINT('Ctrl Pts',(5.64460711165028,2.35350404666548,11.9952879625328));
#6834=CARTESIAN_POINT('Ctrl Pts',(5.57713351168681,2.50921420418439,12.0030115162428));
#6835=CARTESIAN_POINT('Ctrl Pts',(5.50330574906832,2.66185112182698,12.0107350699528));
#6836=CARTESIAN_POINT('Ctrl Pts',(5.42948294505744,2.81447778768144,12.0184581049139));
#6837=CARTESIAN_POINT('Ctrl Pts',(5.34930697045353,2.96403134139491,12.0261811398751));
#6838=CARTESIAN_POINT('Ctrl Pts',(5.26306086232182,3.10998648260668,12.0339041748362));
#6839=CARTESIAN_POINT('Ctrl Pts',(5.1767918337319,3.25598041233643,12.0416292622435));
#6840=CARTESIAN_POINT('Ctrl Pts',(5.08444960756162,3.39837374449056,12.0493543496509));
#6841=CARTESIAN_POINT('Ctrl Pts',(4.9863621453097,3.53666765731846,12.0570794370582));
#6842=CARTESIAN_POINT('Ctrl Pts',(4.88865503332114,3.67442531275977,12.0647745691689));
#6843=CARTESIAN_POINT('Ctrl Pts',(4.78524736914535,3.80811504871322,12.0724697012796));
#6844=CARTESIAN_POINT('Ctrl Pts',(4.67650479358892,3.93727424470785,12.0801648333903));
#6845=CARTESIAN_POINT('Ctrl Pts',(4.56734350635197,4.06693076627836,12.0878895954935));
#6846=CARTESIAN_POINT('Ctrl Pts',(4.45276745753514,4.19206769022086,12.0956143575967));
#6847=CARTESIAN_POINT('Ctrl Pts',(4.33317484178046,4.31224087372921,12.1033391196999));
#6848=CARTESIAN_POINT('Ctrl Pts',(4.2136055548106,4.43239061520211,12.1110623749432));
#6849=CARTESIAN_POINT('Ctrl Pts',(4.08902187693335,4.54757832378144,12.1187856301866));
#6850=CARTESIAN_POINT('Ctrl Pts',(3.95985927996066,4.65739627317769,12.1265088854299));
#6851=CARTESIAN_POINT('Ctrl Pts',(3.83069169147391,4.76721846651028,12.13423243914));
#6852=CARTESIAN_POINT('Ctrl Pts',(3.69694506867638,4.87167027710725,12.14195599285));
#6853=CARTESIAN_POINT('Ctrl Pts',(3.55908901761198,4.97038337829324,12.1496795465601));
#6854=CARTESIAN_POINT('Ctrl Pts',(3.42124222558574,5.06908984945928,12.1574025815212));
#6855=CARTESIAN_POINT('Ctrl Pts',(3.27928681533585,5.16205819801352,12.1651256164823));
#6856=CARTESIAN_POINT('Ctrl Pts',(3.13372264815355,5.2489625572059,12.1728486514435));
#6857=CARTESIAN_POINT('Ctrl Pts',(2.98811979635727,5.33589001179087,12.1805737388508));
#6858=CARTESIAN_POINT('Ctrl Pts',(2.83890654240731,5.41675009231119,12.1882988262582));
#6859=CARTESIAN_POINT('Ctrl Pts',(2.68660952877123,5.49126167673838,12.1960239136655));
#6860=CARTESIAN_POINT('Ctrl Pts',(2.53490307184868,5.56548433024455,12.2037190457762));
#6861=CARTESIAN_POINT('Ctrl Pts',(2.38013702289031,5.63340752656996,12.2114141778868));
#6862=CARTESIAN_POINT('Ctrl Pts',(2.22285379179657,5.69479995985773,12.2191093099975));
#6863=CARTESIAN_POINT('Ctrl Pts',(2.06496494394432,5.7564287838032,12.2268340721007));
#6864=CARTESIAN_POINT('Ctrl Pts',(1.90448356028117,5.81149825078665,12.2345588342039));
#6865=CARTESIAN_POINT('Ctrl Pts',(1.74197179682505,5.85980885537797,12.2422835963071));
#6866=CARTESIAN_POINT('Ctrl Pts',(1.57949173433975,5.90811003607877,12.2500068515504));
#6867=CARTESIAN_POINT('Ctrl Pts',(1.41498238595332,5.94965489490004,12.2577301067937));
#6868=CARTESIAN_POINT('Ctrl Pts',(1.24902121901313,5.98429373919387,12.265453362037));
#6869=CARTESIAN_POINT('Ctrl Pts',(1.08305363847061,6.01893392211273,12.2731769157471));
#6870=CARTESIAN_POINT('Ctrl Pts',(0.915634436526519,6.04666748782398,12.2809004694571));
#6871=CARTESIAN_POINT('Ctrl Pts',(0.747352204760735,6.06739567232427,12.2886240231672));
#6872=CARTESIAN_POINT('Ctrl Pts',(0.579081275593571,6.08812246462559,12.2963470581283));
#6873=CARTESIAN_POINT('Ctrl Pts',(0.409947747182909,6.10184477854802,12.3040700930894));
#6874=CARTESIAN_POINT('Ctrl Pts',(0.240546464961092,6.10851561025219,12.3117931280505));
#6875=CARTESIAN_POINT('Ctrl Pts',(0.071100163258296,6.11518821477283,12.3195182154579));
#6876=CARTESIAN_POINT('Ctrl Pts',(-0.0986137176265944,6.11480557775733,
12.3272433028653));
#6877=CARTESIAN_POINT('Ctrl Pts',(-0.267998222194625,6.10737279977246,12.3349683902726));
#6878=CARTESIAN_POINT('Ctrl Pts',(-0.436725910494112,6.09996884360641,12.3426635223833));
#6879=CARTESIAN_POINT('Ctrl Pts',(-0.605126461881987,6.08556937133074,12.350358654494));
#6880=CARTESIAN_POINT('Ctrl Pts',(-0.772612908578236,6.06423077199395,12.3580537866047));
#6881=CARTESIAN_POINT('Ctrl Pts',(-0.940744259362647,6.04281000869571,12.3657785487079));
#6882=CARTESIAN_POINT('Ctrl Pts',(-1.10801399531538,6.01438895786286,12.3735033108111));
#6883=CARTESIAN_POINT('Ctrl Pts',(-1.27383302332941,5.9790613804489,12.3812280729142));
#6884=CARTESIAN_POINT('Ctrl Pts',(-1.43961970523002,5.94374069434191,12.3889513281576));
#6885=CARTESIAN_POINT('Ctrl Pts',(-1.60395593407248,5.90151623589398,12.396674583401));
#6886=CARTESIAN_POINT('Ctrl Pts',(-1.76626300336345,5.85253283335083,12.4043978386443));
#6887=CARTESIAN_POINT('Ctrl Pts',(-1.92857634504233,5.80354753783468,12.4121213923544));
#6888=CARTESIAN_POINT('Ctrl Pts',(-2.08886006570547,5.74780286331757,12.4198449460644));
#6889=CARTESIAN_POINT('Ctrl Pts',(-2.24655005613366,5.68549368197572,12.4275684997745));
#6890=CARTESIAN_POINT('Ctrl Pts',(-2.40422945538646,5.62318868560126,12.4352915347356));
#6891=CARTESIAN_POINT('Ctrl Pts',(-2.5593151782436,5.55432018120364,12.4430145696967));
#6892=CARTESIAN_POINT('Ctrl Pts',(-2.71126238739099,5.47913148493618,12.4507376046578));
#6893=CARTESIAN_POINT('Ctrl Pts',(-2.8632499774869,5.40392280678889,12.4584626920652));
#6894=CARTESIAN_POINT('Ctrl Pts',(-3.01209710195909,5.32239071916427,12.4661877794726));
#6895=CARTESIAN_POINT('Ctrl Pts',(-3.15728199886066,5.2348253019724,12.4739128668799));
#6896=CARTESIAN_POINT('Ctrl Pts',(-3.30190391745105,5.14759943408449,12.4816079989906));
#6897=CARTESIAN_POINT('Ctrl Pts',(-3.44289170908152,5.05438713274775,12.4893031311012));
#6898=CARTESIAN_POINT('Ctrl Pts',(-3.57975692019151,4.95551873721016,12.4969982632119));
#6899=CARTESIAN_POINT('Ctrl Pts',(-3.71714912877526,4.85626965037592,12.5047230253151));
#6900=CARTESIAN_POINT('Ctrl Pts',(-3.85043558859554,4.75128565004825,12.5124477874183));
#6901=CARTESIAN_POINT('Ctrl Pts',(-3.979143859599,4.64093090953911,12.5201725495215));
#6902=CARTESIAN_POINT('Ctrl Pts',(-4.10782702363795,4.53059769579382,12.5278958047648));
#6903=CARTESIAN_POINT('Ctrl Pts',(-4.2319335403864,4.41489603849501,12.5356190600081));
#6904=CARTESIAN_POINT('Ctrl Pts',(-4.35102452263382,4.29422998521727,12.5433423152515));
#6905=CARTESIAN_POINT('Ctrl Pts',(-4.47012010717551,4.17355926877634,12.5510658689615));
#6906=CARTESIAN_POINT('Ctrl Pts',(-4.5841995439207,4.04792399523236,12.5587894226715));
#6907=CARTESIAN_POINT('Ctrl Pts',(-4.69286070638614,3.91776517327889,12.5665129763816));
#6908=CARTESIAN_POINT('Ctrl Pts',(-4.80151457067522,3.78761509338206,12.5742360113427));
#6909=CARTESIAN_POINT('Ctrl Pts',(-4.9047506858181,3.65294231639115,12.5819590463039));
#6910=CARTESIAN_POINT('Ctrl Pts',(-5.00220702551001,3.51422117067755,12.589682081265));
#6911=CARTESIAN_POINT('Ctrl Pts',(-5.09968926485099,3.37546315892729,12.5974071686724));
#6912=CARTESIAN_POINT('Ctrl Pts',(-5.1913884753169,3.23265488684195,12.6051322560797));
#6913=CARTESIAN_POINT('Ctrl Pts',(-5.27698526683414,3.08630070733806,12.6128573434871));
#6914=CARTESIAN_POINT('Ctrl Pts',(-5.36225014271723,2.94051404023082,12.6205524755977));
#6915=CARTESIAN_POINT('Ctrl Pts',(-5.44145971200606,2.79120920225685,12.6282476077084));
#6916=CARTESIAN_POINT('Ctrl Pts',(-5.51434309483528,2.63890996340202,12.6359427398191));
#6917=CARTESIAN_POINT('Ctrl Pts',(-5.58725262910215,2.48655607774165,12.643640633036));
#6918=CARTESIAN_POINT('Ctrl Pts',(-5.65385889793136,2.33114811101626,12.651338526253));
#6919=CARTESIAN_POINT('Ctrl Pts',(-5.71392213225727,2.17322788243676,12.65903641947));
#6920=CARTESIAN_POINT('Ctrl Pts',(-5.77397291614694,2.01534038895316,12.6667327169998));
#6921=CARTESIAN_POINT('Ctrl Pts',(-5.8274832574358,1.85494197281612,12.6744290145297));
#6922=CARTESIAN_POINT('Ctrl Pts',(-5.87426190130256,1.69259347671116,12.6821253120596));
#6923=CARTESIAN_POINT('Ctrl Pts',(-5.92104057981929,1.53024486035111,12.6898216152902));
#6924=CARTESIAN_POINT('Ctrl Pts',(-5.96108745831491,1.36594646882379,12.6975179185209));
#6925=CARTESIAN_POINT('Ctrl Pts',(-5.99426125300097,1.20027396592247,12.7052142217516));
#6926=CARTESIAN_POINT('Ctrl Pts',(-6.02743352763924,1.03460905425766,12.712910172332));
#6927=CARTESIAN_POINT('Ctrl Pts',(-6.05373328646756,0.86757047246313,12.7206061229124));
#6928=CARTESIAN_POINT('Ctrl Pts',(-6.07307039063346,0.69974394810615,12.7283020734927));
#6929=CARTESIAN_POINT('Ctrl Pts',(-6.0924113036645,0.531884366648455,12.7359995399587));
#6930=CARTESIAN_POINT('Ctrl Pts',(-6.10478678589844,0.363236851908962,12.7436970064247));
#6931=CARTESIAN_POINT('Ctrl Pts',(-6.11015850685667,0.194392858889112,12.7513944728907));
#6932=CARTESIAN_POINT('Ctrl Pts',(-6.11222055291481,0.129578604210711,12.754349304407));
#6933=CARTESIAN_POINT('Ctrl Pts',(-6.1132510932271,0.0647354281208469,12.7573041359232));
#6934=CARTESIAN_POINT('Ctrl Pts',(-6.11324999912966,-0.000103156033837302,
12.7602589674395));
#6935=CARTESIAN_POINT('Ctrl Pts',(-6.11362854109631,-0.000103162421420267,
12.7602589674395));
#6936=CARTESIAN_POINT('Ctrl Pts',(-6.11371354863409,-0.107106860351694,
12.7651350504351));
#6937=CARTESIAN_POINT('Ctrl Pts',(-6.08482838106602,-1.23042505733209,12.8163259589664));
#6938=CARTESIAN_POINT('Ctrl Pts',(-5.42822856457523,-3.3384373253954,12.9138316930335));
#6939=CARTESIAN_POINT('Ctrl Pts',(-3.16946315476177,-5.52859226525806,13.0527761696406));
#6940=CARTESIAN_POINT('Ctrl Pts',(-0.138148106431394,-6.37116506029729,
13.1917206462478));
#6941=CARTESIAN_POINT('Ctrl Pts',(2.26894793050691,-5.81326278514897,13.3008410282742));
#6942=CARTESIAN_POINT('Ctrl Pts',(3.43573368210399,-5.06927082860839,13.363646584765));
#6943=CARTESIAN_POINT('Ctrl Pts',(3.72270802987534,-4.84860079634452,13.3801373157199));
#6944=CARTESIAN_POINT('',(-6.11324999800781,-0.000156069087590843,12.6147410325606));
#6945=CARTESIAN_POINT('Ctrl Pts',(-6.11331623078485,-0.000156070778496338,
12.6147410325606));
#6946=CARTESIAN_POINT('Ctrl Pts',(-6.11353700954689,-0.21382808103462,12.6244764787917));
#6947=CARTESIAN_POINT('Ctrl Pts',(-6.05029720305683,-1.44388040587524,12.6805267505586));
#6948=CARTESIAN_POINT('Ctrl Pts',(-5.24613718046346,-3.6178548867268,12.7828918478612));
#6949=CARTESIAN_POINT('Ctrl Pts',(-2.8758824236554,-5.68683827649109,12.9218363244684));
#6950=CARTESIAN_POINT('Ctrl Pts',(0.195362317363167,-6.36966740596466,13.0607808010756));
#6951=CARTESIAN_POINT('Ctrl Pts',(2.46424006555832,-5.71701172825789,13.1650423969484));
#6952=CARTESIAN_POINT('Ctrl Pts',(3.52053820541315,-5.00452290254849,13.2229891672854));
#6953=CARTESIAN_POINT('Ctrl Pts',(3.72288481551393,-4.8488307603735,13.2346211120867));
#6954=CARTESIAN_POINT('Ctrl Pts',(3.72292453512039,-4.84888218750453,11.484610425966));
#6955=CARTESIAN_POINT('Ctrl Pts',(3.86158194725542,-4.74242237642805,11.4925739480377));
#6956=CARTESIAN_POINT('Ctrl Pts',(3.99566183533874,-4.63001736623254,11.5005374701095));
#6957=CARTESIAN_POINT('Ctrl Pts',(4.12466559379199,-4.51209034726573,11.5085009921812));
#6958=CARTESIAN_POINT('Ctrl Pts',(4.25366935224525,-4.39416332829891,11.516464514253));
#6959=CARTESIAN_POINT('Ctrl Pts',(4.37759671475846,-4.27071455614831,11.5244280363247));
#6960=CARTESIAN_POINT('Ctrl Pts',(4.49598948302034,-4.14221005395315,11.5323915583965));
#6961=CARTESIAN_POINT('Ctrl Pts',(4.61083263424427,-4.01755833581853,11.5401163204997));
#6962=CARTESIAN_POINT('Ctrl Pts',(4.72050895726609,-3.88810554571865,11.5478410826029));
#6963=CARTESIAN_POINT('Ctrl Pts',(4.82462811457528,-3.75430274732203,11.5555658447061));
#6964=CARTESIAN_POINT('Ctrl Pts',(4.92872696148876,-3.62052604967242,11.5632890999494));
#6965=CARTESIAN_POINT('Ctrl Pts',(5.02727061120222,-3.48240128685783,11.5710123551928));
#6966=CARTESIAN_POINT('Ctrl Pts',(5.11990955609688,-3.34041190572179,11.5787356104362));
#6967=CARTESIAN_POINT('Ctrl Pts',(5.21255208104128,-3.19841703737895,11.5864591641462));
#6968=CARTESIAN_POINT('Ctrl Pts',(5.29928926805948,-3.05255751511587,11.5941827178563));
#6969=CARTESIAN_POINT('Ctrl Pts',(5.37981500201618,-2.90334567466253,11.6019062715663));
#6970=CARTESIAN_POINT('Ctrl Pts',(5.46033532749914,-2.75414385595356,11.6096293065274));
#6971=CARTESIAN_POINT('Ctrl Pts',(5.53464488425912,-2.60159044856381,11.6173523414886));
#6972=CARTESIAN_POINT('Ctrl Pts',(5.60248349593993,-2.44622244291494,11.6250753764497));
#6973=CARTESIAN_POINT('Ctrl Pts',(5.6703401361683,-2.29081314721885,11.6328004638571));
#6974=CARTESIAN_POINT('Ctrl Pts',(5.73172226604339,-2.13258804836254,11.6405255512644));
#6975=CARTESIAN_POINT('Ctrl Pts',(5.78641747607167,-1.97210505681425,11.6482506386718));
#6976=CARTESIAN_POINT('Ctrl Pts',(5.84090059642908,-1.81224436445526,11.6559457707824));
#6977=CARTESIAN_POINT('Ctrl Pts',(5.8887484938185,-1.65014356487504,11.6636409028931));
#6978=CARTESIAN_POINT('Ctrl Pts',(5.92980016652284,-1.4863699228677,11.6713360350037));
#6979=CARTESIAN_POINT('Ctrl Pts',(5.97100990808674,-1.32196567287013,11.6790607971069));
#6980=CARTESIAN_POINT('Ctrl Pts',(6.00538554968506,-1.15581743796826,11.6867855592101));
#6981=CARTESIAN_POINT('Ctrl Pts',(6.03280012781083,-0.988508057825365,11.6945103213133));
#6982=CARTESIAN_POINT('Ctrl Pts',(6.06020935820837,-0.821231314518607,11.7022335765566));
#6983=CARTESIAN_POINT('Ctrl Pts',(6.08066018338688,-0.652794190491557,11.7099568317999));
#6984=CARTESIAN_POINT('Ctrl Pts',(6.09407698669119,-0.483788427704495,11.7176800870432));
#6985=CARTESIAN_POINT('Ctrl Pts',(6.10749430849052,-0.314776133656291,11.7254036407533));
#6986=CARTESIAN_POINT('Ctrl Pts',(6.11387703543591,-0.145195472484922,11.7331271944633));
#6987=CARTESIAN_POINT('Ctrl Pts',(6.11320147623289,0.0243572059971047,11.7408507481733));
#6988=CARTESIAN_POINT('Ctrl Pts',(6.1125259624035,0.193898496552499,11.7485737831345));
#6989=CARTESIAN_POINT('Ctrl Pts',(6.10479311237982,0.363411491224797,11.7562968180956));
#6990=CARTESIAN_POINT('Ctrl Pts',(6.0900313704341,0.532300168728613,11.7640198530568));
#6991=CARTESIAN_POINT('Ctrl Pts',(6.07526570546054,0.701233729484569,11.7717449404641));
#6992=CARTESIAN_POINT('Ctrl Pts',(6.05346744134481,0.869542325395739,11.7794700278715));
#6993=CARTESIAN_POINT('Ctrl Pts',(6.02471697645032,1.0366344178018,11.7871951152789));
#6994=CARTESIAN_POINT('Ctrl Pts',(5.99607799621096,1.20307858314427,11.7948902473895));
#6995=CARTESIAN_POINT('Ctrl Pts',(5.96054072066098,1.36831536039421,11.8025853795002));
#6996=CARTESIAN_POINT('Ctrl Pts',(5.91823516605736,1.53176959159725,11.8102805116109));
#6997=CARTESIAN_POINT('Ctrl Pts',(5.87576671454066,1.69585320090303,11.8180052737141));
#6998=CARTESIAN_POINT('Ctrl Pts',(5.82646268805614,1.85819861558642,11.8257300358173));
#6999=CARTESIAN_POINT('Ctrl Pts',(5.77049044417457,2.01823328586911,11.8334547979205));
#7000=CARTESIAN_POINT('Ctrl Pts',(5.71452911872981,2.17823673838537,11.8411780531639));
#7001=CARTESIAN_POINT('Ctrl Pts',(5.65190227593882,2.33593004694149,11.8489013084072));
#7002=CARTESIAN_POINT('Ctrl Pts',(5.58282662150262,2.4907574102553,11.8566245636506));
#7003=CARTESIAN_POINT('Ctrl Pts',(5.51374829762438,2.64559075690253,11.8643481173606));
#7004=CARTESIAN_POINT('Ctrl Pts',(5.43822078891153,2.7975576456458,11.8720716710707));
#7005=CARTESIAN_POINT('Ctrl Pts',(5.3565086026111,2.94612307153881,11.8797952247807));
#7006=CARTESIAN_POINT('Ctrl Pts',(5.27480190447206,3.09467851910336,11.8875182597419));
#7007=CARTESIAN_POINT('Ctrl Pts',(5.18691151276608,3.23983268327991,11.895241294703));
#7008=CARTESIAN_POINT('Ctrl Pts',(5.09314755916535,3.38107579079027,11.9029643296641));
#7009=CARTESIAN_POINT('Ctrl Pts',(4.99935868719056,3.52235643456537,11.9106894170714));
#7010=CARTESIAN_POINT('Ctrl Pts',(4.89969330778148,3.65972367929024,11.9184145044788));
#7011=CARTESIAN_POINT('Ctrl Pts',(4.79450503023508,3.79269654435344,11.9261395918862));
#7012=CARTESIAN_POINT('Ctrl Pts',(4.68972463753176,3.92515378526663,11.9338347239968));
#7013=CARTESIAN_POINT('Ctrl Pts',(4.57946432140999,4.05325044095243,11.9415298561074));
#7014=CARTESIAN_POINT('Ctrl Pts',(4.46411342492558,4.17654365377631,11.9492249882181));
#7015=CARTESIAN_POINT('Ctrl Pts',(4.34831837151762,4.30031160529552,11.9569497503213));
#7016=CARTESIAN_POINT('Ctrl Pts',(4.22735242442935,4.41928286376296,11.9646745124245));
#7017=CARTESIAN_POINT('Ctrl Pts',(4.10163646927133,4.53303472702818,11.9723992745277));
#7018=CARTESIAN_POINT('Ctrl Pts',(3.9759450373703,4.64676440085713,11.980122529771));
#7019=CARTESIAN_POINT('Ctrl Pts',(3.84550568111629,4.75527649852969,11.9878457850144));
#7020=CARTESIAN_POINT('Ctrl Pts',(3.71077460703088,4.85818663477586,11.9955690402577));
#7021=CARTESIAN_POINT('Ctrl Pts',(3.57603832623683,4.96110074800433,12.0032925939678));
#7022=CARTESIAN_POINT('Ctrl Pts',(3.43701024517634,5.05841227108009,12.0110161476778));
#7023=CARTESIAN_POINT('Ctrl Pts',(3.29417859658111,5.14977795019619,12.0187397013879));
#7024=CARTESIAN_POINT('Ctrl Pts',(3.15135654120784,5.24113749277849,12.026462736349));
#7025=CARTESIAN_POINT('Ctrl Pts',(3.00473169653404,5.32655181977587,12.0341857713101));
#7026=CARTESIAN_POINT('Ctrl Pts',(2.85482028772225,5.40572166202714,12.0419088062712));
#7027=CARTESIAN_POINT('Ctrl Pts',(2.70486903898894,5.48491254417341,12.0496338936786));
#7028=CARTESIAN_POINT('Ctrl Pts',(2.55162976022748,5.55785547543274,12.0573589810859));
#7029=CARTESIAN_POINT('Ctrl Pts',(2.39564308018388,5.6242972712035,12.0650840684933));
#7030=CARTESIAN_POINT('Ctrl Pts',(2.24026126414162,5.69048142798587,12.072779200604));
#7031=CARTESIAN_POINT('Ctrl Pts',(2.08215361579399,5.75021468541692,12.0804743327146));
#7032=CARTESIAN_POINT('Ctrl Pts',(1.92187390348632,5.80329443175152,12.0881694648253));
#7033=CARTESIAN_POINT('Ctrl Pts',(1.76097703651381,5.85657856086538,12.0958942269285));
#7034=CARTESIAN_POINT('Ctrl Pts',(1.59783435105387,5.90317668182732,12.1036189890317));
#7035=CARTESIAN_POINT('Ctrl Pts',(1.43301767081955,5.94291897282968,12.1113437511349));
#7036=CARTESIAN_POINT('Ctrl Pts',(1.26823314117254,5.98265351135215,12.1190670063782));
#7037=CARTESIAN_POINT('Ctrl Pts',(1.10177557623251,6.0155348141777,12.1267902616215));
#7038=CARTESIAN_POINT('Ctrl Pts',(0.934229484010322,6.04144360510845,12.1345135168649));
#7039=CARTESIAN_POINT('Ctrl Pts',(0.766676916936759,6.06735339728948,12.1422370705749));
#7040=CARTESIAN_POINT('Ctrl Pts',(0.59803605099373,6.08629008603538,12.149960624285));
#7041=CARTESIAN_POINT('Ctrl Pts',(0.428899838748377,6.0981858360353,12.157684177995));
#7042=CARTESIAN_POINT('Ctrl Pts',(0.259774986458183,6.1100807870627,12.1654072129562));
#7043=CARTESIAN_POINT('Ctrl Pts',(0.0901551706205841,6.11493572346633,12.1731302479173));
#7044=CARTESIAN_POINT('Ctrl Pts',(-0.0793631188539132,6.11273482639855,
12.1808532828785));
#7045=CARTESIAN_POINT('Ctrl Pts',(-0.248926458904212,6.11053334442823,12.1885783702858));
#7046=CARTESIAN_POINT('Ctrl Pts',(-0.418387901524658,6.10127228395309,12.1963034576932));
#7047=CARTESIAN_POINT('Ctrl Pts',(-0.587151575582146,6.08498796956834,12.2040285451006));
#7048=CARTESIAN_POINT('Ctrl Pts',(-0.755260840741822,6.06876680029042,12.2117236772112));
#7049=CARTESIAN_POINT('Ctrl Pts',(-0.922677431494252,6.04557680999582,12.2194188093218));
#7050=CARTESIAN_POINT('Ctrl Pts',(-1.08881813401474,6.01550501899389,12.2271139414324));
#7051=CARTESIAN_POINT('Ctrl Pts',(-1.25559855885688,5.98531743700477,12.2348387035356));
#7052=CARTESIAN_POINT('Ctrl Pts',(-1.4211523137012,5.94818423147259,12.2425634656388));
#7053=CARTESIAN_POINT('Ctrl Pts',(-1.58489601749832,5.9042298546227,12.250288227742));
#7054=CARTESIAN_POINT('Ctrl Pts',(-1.74860778001208,5.86028405189916,12.2580114829853));
#7055=CARTESIAN_POINT('Ctrl Pts',(-1.91050989010417,5.80951981499163,12.2657347382286));
#7056=CARTESIAN_POINT('Ctrl Pts',(-2.07003201081014,5.75211205008398,12.2734579934719));
#7057=CARTESIAN_POINT('Ctrl Pts',(-2.2295602962801,5.69470206664187,12.281181547182));
#7058=CARTESIAN_POINT('Ctrl Pts',(-2.3867081087786,5.63064814503191,12.288905100892));
#7059=CARTESIAN_POINT('Ctrl Pts',(-2.54092230678068,5.56017440314639,12.2966286546021));
#7060=CARTESIAN_POINT('Ctrl Pts',(-2.69512614705694,5.48970539459741,12.3043516895632));
#7061=CARTESIAN_POINT('Ctrl Pts',(-2.84639647885681,5.41281756038992,12.3120747245243));
#7062=CARTESIAN_POINT('Ctrl Pts',(-2.99420194061909,5.32978238779904,12.3197977594854));
#7063=CARTESIAN_POINT('Ctrl Pts',(-3.14204668263394,5.24672514807673,12.3275228468927));
#7064=CARTESIAN_POINT('Ctrl Pts',(-3.28642443703427,5.15751745888855,12.3352479343001));
#7065=CARTESIAN_POINT('Ctrl Pts',(-3.42682933257148,5.06247629998677,12.3429730217074));
#7066=CARTESIAN_POINT('Ctrl Pts',(-3.56668978504021,4.96780367880574,12.3506681538182));
#7067=CARTESIAN_POINT('Ctrl Pts',(-3.70260789424474,4.8673429496621,12.3583632859289));
#7068=CARTESIAN_POINT('Ctrl Pts',(-3.8341131579617,4.7614495539116,12.3660584180396));
#7069=CARTESIAN_POINT('Ctrl Pts',(-3.96612478075329,4.65514841720559,12.3737831801428));
#7070=CARTESIAN_POINT('Ctrl Pts',(-4.09373624316244,4.54333502195203,12.381507942246));
#7071=CARTESIAN_POINT('Ctrl Pts',(-4.2164948046448,4.42639775945445,12.3892327043492));
#7072=CARTESIAN_POINT('Ctrl Pts',(-4.33922941976432,4.30948330776602,12.3969559595925));
#7073=CARTESIAN_POINT('Ctrl Pts',(-4.4571127935254,4.18744720166812,12.4046792148358));
#7074=CARTESIAN_POINT('Ctrl Pts',(-4.56972777838454,4.06071589673061,12.4124024700791));
#7075=CARTESIAN_POINT('Ctrl Pts',(-4.68234711527243,3.93397969423632,12.4201260237892));
#7076=CARTESIAN_POINT('Ctrl Pts',(-4.78969744237316,3.8025481640848,12.4278495774992));
#7077=CARTESIAN_POINT('Ctrl Pts',(-4.89140025622809,3.66688274913063,12.4355731312092));
#7078=CARTESIAN_POINT('Ctrl Pts',(-4.99309623926017,3.53122644608183,12.4432961661703));
#7079=CARTESIAN_POINT('Ctrl Pts',(-5.08914527799931,3.39133708090647,12.4510192011314));
#7080=CARTESIAN_POINT('Ctrl Pts',(-5.17921065743964,3.24770727257917,12.4587422360925));
#7081=CARTESIAN_POINT('Ctrl Pts',(-5.26929997233436,3.10403929370568,12.4664673234999));
#7082=CARTESIAN_POINT('Ctrl Pts',(-5.35340227999785,2.9566291528682,12.4741924109073));
#7083=CARTESIAN_POINT('Ctrl Pts',(-5.43122501406473,2.80599722186206,12.4819174983146));
#7084=CARTESIAN_POINT('Ctrl Pts',(-5.50874597768429,2.65594939093599,12.4896126304254));
#7085=CARTESIAN_POINT('Ctrl Pts',(-5.58003586663959,2.50270500362402,12.4973077625361));
#7086=CARTESIAN_POINT('Ctrl Pts',(-5.6448515741856,2.34680128428343,12.5050028946468));
#7087=CARTESIAN_POINT('Ctrl Pts',(-5.70967202129114,2.19088616469765,12.5126985894535));
#7088=CARTESIAN_POINT('Ctrl Pts',(-5.76804186624444,2.03225215979232,12.5203942842602));
#7089=CARTESIAN_POINT('Ctrl Pts',(-5.81975006970807,1.87145256114946,12.5280899790669));
#7090=CARTESIAN_POINT('Ctrl Pts',(-5.87145192307247,1.71067270972931,12.5357847287929));
#7091=CARTESIAN_POINT('Ctrl Pts',(-5.91649366547352,1.54772810027992,12.5434794785189));
#7092=CARTESIAN_POINT('Ctrl Pts',(-5.95471365910835,1.3831886351935,12.5511742282449));
#7093=CARTESIAN_POINT('Ctrl Pts',(-5.99292850060074,1.21867135040279,12.558867940701));
#7094=CARTESIAN_POINT('Ctrl Pts',(-6.02432335703991,1.05255995264312,12.5665616531572));
#7095=CARTESIAN_POINT('Ctrl Pts',(-6.04878732671191,0.885436298504514,12.5742553656133));
#7096=CARTESIAN_POINT('Ctrl Pts',(-6.07325456934187,0.718290285415124,12.5819501073872));
#7097=CARTESIAN_POINT('Ctrl Pts',(-6.09078902373148,0.550132063452321,12.5896448491611));
#7098=CARTESIAN_POINT('Ctrl Pts',(-6.10133135165719,0.381551175840124,12.5973395909349));
#7099=CARTESIAN_POINT('Ctrl Pts',(-6.10927841080438,0.254470867356085,12.6031400714768));
#7100=CARTESIAN_POINT('Ctrl Pts',(-6.11325324810064,0.127150563502077,12.6089405520187));
#7101=CARTESIAN_POINT('Ctrl Pts',(-6.11324999800781,-0.000156069087590843,
12.6147410325606));
#7102=CARTESIAN_POINT('Origin',(0.,0.,-3.86474103256053));
#7103=CARTESIAN_POINT('',(3.72292453512039,-4.84888218750452,9.73461637809168));
#7104=CARTESIAN_POINT('',(3.72292453512037,-4.84888218750454,9.88013638533173));
#7105=CARTESIAN_POINT('',(3.72292453512038,-4.84888218750453,-3.86474103256053));
#7106=CARTESIAN_POINT('',(-6.1132499981976,0.000148448865203969,11.0102589674072));
#7107=CARTESIAN_POINT('Ctrl Pts',(3.72292453512037,-4.84888218750454,9.88013638533173));
#7108=CARTESIAN_POINT('Ctrl Pts',(3.85737370293807,-4.74565342544368,9.88785964524372));
#7109=CARTESIAN_POINT('Ctrl Pts',(3.98754260366794,-4.63681706701032,9.89558290515572));
#7110=CARTESIAN_POINT('Ctrl Pts',(4.11297118110572,-4.52275288136482,9.90330616506772));
#7111=CARTESIAN_POINT('Ctrl Pts',(4.23841654062291,-4.4086734341716,9.91103045833562));
#7112=CARTESIAN_POINT('Ctrl Pts',(4.35912007031516,-4.28936497025535,9.91875475160352));
#7113=CARTESIAN_POINT('Ctrl Pts',(4.47465630588625,-4.16524627203391,9.92647904487143));
#7114=CARTESIAN_POINT('Ctrl Pts',(4.59017373171417,-4.04114778081355,9.9342020805947));
#7115=CARTESIAN_POINT('Ctrl Pts',(4.70052533083415,-3.91224085440095,9.94192511631798));
#7116=CARTESIAN_POINT('Ctrl Pts',(4.80532400580619,-3.77897959265762,9.94964815204125));
#7117=CARTESIAN_POINT('Ctrl Pts',(4.91015056888418,-3.64568286859392,9.95737324295118));
#7118=CARTESIAN_POINT('Ctrl Pts',(5.00942105723682,-3.50802974169527,9.96509833386111));
#7119=CARTESIAN_POINT('Ctrl Pts',(5.10278932642359,-3.36650659477113,9.97282342477104));
#7120=CARTESIAN_POINT('Ctrl Pts',(5.19615351356833,-3.22498963521062,9.98054817794154));
#7121=CARTESIAN_POINT('Ctrl Pts',(5.28361582994328,-3.07960326306029,9.98827293111204));
#7122=CARTESIAN_POINT('Ctrl Pts',(5.36487414676132,-2.93086181044279,9.99599768428254));
#7123=CARTESIAN_POINT('Ctrl Pts',(5.44613255754426,-2.78212018582472,10.0037224463857));
#7124=CARTESIAN_POINT('Ctrl Pts',(5.52121573322926,-2.62997079402401,10.0114472084889));
#7125=CARTESIAN_POINT('Ctrl Pts',(5.58985411552551,-2.47494576296988,10.0191719705921));
#7126=CARTESIAN_POINT('Ctrl Pts',(5.65847910861668,-2.31995097245847,10.0268952258355));
#7127=CARTESIAN_POINT('Ctrl Pts',(5.7206616886098,-2.1620819516009,10.0346184810788));
#7128=CARTESIAN_POINT('Ctrl Pts',(5.77617975100661,-2.00189236637769,10.0423417363221));
#7129=CARTESIAN_POINT('Ctrl Pts',(5.83169995890988,-1.84169659059638,10.0500652900322));
#7130=CARTESIAN_POINT('Ctrl Pts',(5.88055502631713,-1.67918036914357,10.0577888437422));
#7131=CARTESIAN_POINT('Ctrl Pts',(5.92257194317969,-1.51491489541849,10.0655123974523));
#7132=CARTESIAN_POINT('Ctrl Pts',(5.96458603799538,-1.35066045450827,10.0732354324134));
#7133=CARTESIAN_POINT('Ctrl Pts',(5.99976282282497,-1.18465730351075,10.0809584673745));
#7134=CARTESIAN_POINT('Ctrl Pts',(6.02797982783107,-1.01748943864871,10.0886815023356));
#7135=CARTESIAN_POINT('Ctrl Pts',(6.05620433168782,-0.850277147850894,10.096406589743));
#7136=CARTESIAN_POINT('Ctrl Pts',(6.07746530482299,-0.681899837035541,10.1041316771503));
#7137=CARTESIAN_POINT('Ctrl Pts',(6.09169168742327,-0.512950239183375,10.1118567645577));
#7138=CARTESIAN_POINT('Ctrl Pts',(6.10586290488572,-0.344655771177826,10.1195518966684));
#7139=CARTESIAN_POINT('Ctrl Pts',(6.11305399632487,-0.175793760313002,10.127247028779));
#7140=CARTESIAN_POINT('Ctrl Pts',(6.11324604529533,-0.00695357325546233,
10.1349421608897));
#7141=CARTESIAN_POINT('Ctrl Pts',(6.11343883374751,0.162536730448309,10.1426669229929));
#7142=CARTESIAN_POINT('Ctrl Pts',(6.10657861157093,0.332065070403449,10.1503916850961));
#7143=CARTESIAN_POINT('Ctrl Pts',(6.09268325815753,0.501035206614228,10.1581164471993));
#7144=CARTESIAN_POINT('Ctrl Pts',(6.07879061529368,0.669972382027743,10.1658397024426));
#7145=CARTESIAN_POINT('Ctrl Pts',(6.05786560545085,0.838351255299317,10.1735629576859));
#7146=CARTESIAN_POINT('Ctrl Pts',(6.02997808286865,1.00557937659029,10.1812862129293));
#7147=CARTESIAN_POINT('Ctrl Pts',(6.00208948256765,1.17281396044494,10.1890097666393));
#7148=CARTESIAN_POINT('Ctrl Pts',(5.96723787932955,1.33889739007713,10.1967333203494));
#7149=CARTESIAN_POINT('Ctrl Pts',(5.92554462414148,1.50324531258475,10.2044568740594));
#7150=CARTESIAN_POINT('Ctrl Pts',(5.88385416926168,1.6675821967399,10.2121799090205));
#7151=CARTESIAN_POINT('Ctrl Pts',(5.8353230599455,1.83018349981151,10.2199029439816));
#7152=CARTESIAN_POINT('Ctrl Pts',(5.78012315310418,1.99047780631912,10.2276259789428));
#7153=CARTESIAN_POINT('Ctrl Pts',(5.72490857653243,2.15081471207011,10.2353510663501));
#7154=CARTESIAN_POINT('Ctrl Pts',(5.66302176220145,2.3088430955587,10.2430761537575));
#7155=CARTESIAN_POINT('Ctrl Pts',(5.59468389142722,2.46400846538822,10.2508012411648));
#7156=CARTESIAN_POINT('Ctrl Pts',(5.5266110119838,2.61857215598217,10.2584963732755));
#7157=CARTESIAN_POINT('Ctrl Pts',(5.45213717255982,2.77029472434611,10.2661915053862));
#7158=CARTESIAN_POINT('Ctrl Pts',(5.37152773238069,2.91864958204393,10.2738866374969));
#7159=CARTESIAN_POINT('Ctrl Pts',(5.29060790674295,3.06757567792972,10.2816113996001));
#7160=CARTESIAN_POINT('Ctrl Pts',(5.20347645069713,3.21316080788342,10.2893361617033));
#7161=CARTESIAN_POINT('Ctrl Pts',(5.11043432325565,3.35488995202385,10.2970609238065));
#7162=CARTESIAN_POINT('Ctrl Pts',(5.01741034542794,3.49659144923383,10.3047841790498));
#7163=CARTESIAN_POINT('Ctrl Pts',(4.91847817064782,3.63443819672686,10.3125074342932));
#7164=CARTESIAN_POINT('Ctrl Pts',(4.81398258507628,3.7679433691448,10.3202306895365));
#7165=CARTESIAN_POINT('Ctrl Pts',(4.70948296125224,3.90145370089646,10.3279542432465));
#7166=CARTESIAN_POINT('Ctrl Pts',(4.5994196886256,4.03062186982901,10.3356777969566));
#7167=CARTESIAN_POINT('Ctrl Pts',(4.48417890018445,4.15499279826579,10.3434013506666));
#7168=CARTESIAN_POINT('Ctrl Pts',(4.36894585183767,4.27935537338655,10.3511243856278));
#7169=CARTESIAN_POINT('Ctrl Pts',(4.24853619900322,4.39892112030591,10.3588474205889));
#7170=CARTESIAN_POINT('Ctrl Pts',(4.12337423559869,4.51327048554603,10.36657045555));
#7171=CARTESIAN_POINT('Ctrl Pts',(3.99817900959706,4.62765023986573,10.3742955429574));
#7172=CARTESIAN_POINT('Ctrl Pts',(3.86822918200473,4.736810626842,10.3820206303647));
#7173=CARTESIAN_POINT('Ctrl Pts',(3.73398426281008,4.8403705527146,10.3897457177721));
#7174=CARTESIAN_POINT('Ctrl Pts',(3.60025990036412,4.94352890794579,10.3974408498828));
#7175=CARTESIAN_POINT('Ctrl Pts',(3.46227396382763,5.04112999312155,10.4051359819934));
#7176=CARTESIAN_POINT('Ctrl Pts',(3.32051140737212,5.13283835280361,10.4128311141041));
#7177=CARTESIAN_POINT('Ctrl Pts',(3.17820299628681,5.22489983417008,10.4205558762073));
#7178=CARTESIAN_POINT('Ctrl Pts',(3.03203840619653,5.31105570048242,10.4282806383105));
#7179=CARTESIAN_POINT('Ctrl Pts',(2.88252831764012,5.39099768693169,10.4360054004137));
#7180=CARTESIAN_POINT('Ctrl Pts',(2.73304739383332,5.47092407919571,10.443728655657));
#7181=CARTESIAN_POINT('Ctrl Pts',(2.58022255304897,5.5446388608911,10.4514519109004));
#7182=CARTESIAN_POINT('Ctrl Pts',(2.42458947250475,5.61187949374531,10.4591751661437));
#7183=CARTESIAN_POINT('Ctrl Pts',(2.26895037748954,5.67912272512699,10.4668987198538));
#7184=CARTESIAN_POINT('Ctrl Pts',(2.11050311490458,5.73989117768262,10.4746222735638));
#7185=CARTESIAN_POINT('Ctrl Pts',(1.94980448067649,5.79396997313879,10.4823458272738));
#7186=CARTESIAN_POINT('Ctrl Pts',(1.78911663969801,5.84804513641761,10.490068862235));
#7187=CARTESIAN_POINT('Ctrl Pts',(1.6261780300826,5.89543144064883,10.4977918971961));
#7188=CARTESIAN_POINT('Ctrl Pts',(1.46156196204963,5.93596345959016,10.5055149321572));
#7189=CARTESIAN_POINT('Ctrl Pts',(1.29690214623741,5.97650625017632,10.5132400195646));
#7190=CARTESIAN_POINT('Ctrl Pts',(1.13056428863167,6.01019103759166,10.520965106972));
#7191=CARTESIAN_POINT('Ctrl Pts',(0.963134223349178,6.03690301647406,10.5286901943793));
#7192=CARTESIAN_POINT('Ctrl Pts',(0.796353395676169,6.06351141526596,10.53638532649));
#7193=CARTESIAN_POINT('Ctrl Pts',(0.628489129067831,6.0832009684698,10.5440804586006));
#7194=CARTESIAN_POINT('Ctrl Pts',(0.460127766134396,6.09590912016675,10.5517755907113));
#7195=CARTESIAN_POINT('Ctrl Pts',(0.291118130259757,6.1086662044141,10.5595003528145));
#7196=CARTESIAN_POINT('Ctrl Pts',(0.121547701892418,6.11439250510157,10.5672251149177));
#7197=CARTESIAN_POINT('Ctrl Pts',(-0.0479875941549688,6.11306165135828,
10.5749498770209));
#7198=CARTESIAN_POINT('Ctrl Pts',(-0.217489819160041,6.111731057223,10.5826731322642));
#7199=CARTESIAN_POINT('Ctrl Pts',(-0.386956608795583,6.10334605801405,10.5903963875075));
#7200=CARTESIAN_POINT('Ctrl Pts',(-0.555791964925009,6.08793239566807,10.5981196427509));
#7201=CARTESIAN_POINT('Ctrl Pts',(-0.724633845730077,6.07251813765807,10.6058431964609));
#7202=CARTESIAN_POINT('Ctrl Pts',(-0.892843928233819,6.05007469784273,10.613566750171));
#7203=CARTESIAN_POINT('Ctrl Pts',(-1.0598304713475,6.02067977345609,10.621290303881));
#7204=CARTESIAN_POINT('Ctrl Pts',(-1.22680579888697,5.99128682336601,10.6290133388421));
#7205=CARTESIAN_POINT('Ctrl Pts',(-1.39255743933224,5.95494337799063,10.6367363738032));
#7206=CARTESIAN_POINT('Ctrl Pts',(-1.55650280926096,5.91177846060411,10.6444594087644));
#7207=CARTESIAN_POINT('Ctrl Pts',(-1.72049174872666,5.86860207186305,10.6521844961717));
#7208=CARTESIAN_POINT('Ctrl Pts',(-1.8826731512105,5.81860066723842,10.6599095835791));
#7209=CARTESIAN_POINT('Ctrl Pts',(-2.04247765423843,5.76195371331953,10.6676346709864));
#7210=CARTESIAN_POINT('Ctrl Pts',(-2.20166248902901,5.70552641727898,10.6753298030971));
#7211=CARTESIAN_POINT('Ctrl Pts',(-2.35848854175393,5.64250515343708,10.6830249352078));
#7212=CARTESIAN_POINT('Ctrl Pts',(-2.5124110010795,5.57311551326139,10.6907200673185));
#7213=CARTESIAN_POINT('Ctrl Pts',(-2.6669261365608,5.50345868930129,10.6984448294217));
#7214=CARTESIAN_POINT('Ctrl Pts',(-2.81856998609195,5.42735965122814,10.7061695915249));
#7215=CARTESIAN_POINT('Ctrl Pts',(-2.9668066359424,5.34508034995061,10.7138943536281));
#7216=CARTESIAN_POINT('Ctrl Pts',(-3.1150143694511,5.26281709879562,10.7216176088714));
#7217=CARTESIAN_POINT('Ctrl Pts',(-3.25981595253619,5.17437614370629,10.7293408641148));
#7218=CARTESIAN_POINT('Ctrl Pts',(-3.40070033937066,5.08006523228829,10.7370641193581));
#7219=CARTESIAN_POINT('Ctrl Pts',(-3.54159017071021,4.98575067620641,10.7447876730681));
#7220=CARTESIAN_POINT('Ctrl Pts',(-3.67856223731683,4.88556588286836,10.7525112267782));
#7221=CARTESIAN_POINT('Ctrl Pts',(-3.81113408852214,4.7798621864866,10.7602347804882));
#7222=CARTESIAN_POINT('Ctrl Pts',(-3.94369703560019,4.67416558964487,10.7679578154493));
#7223=CARTESIAN_POINT('Ctrl Pts',(-4.07186011087741,4.56295102914326,10.7756808504105));
#7224=CARTESIAN_POINT('Ctrl Pts',(-4.19517346114997,4.44661052863447,10.7834038853716));
#7225=CARTESIAN_POINT('Ctrl Pts',(-4.31851958273881,4.33023910988911,10.7911289727789));
#7226=CARTESIAN_POINT('Ctrl Pts',(-4.43701317171454,4.20873924508374,10.7988540601863));
#7227=CARTESIAN_POINT('Ctrl Pts',(-4.5502401180904,4.08254092817459,10.8065791475937));
#7228=CARTESIAN_POINT('Ctrl Pts',(-4.66302800836339,3.95683196599049,10.8142742797043));
#7229=CARTESIAN_POINT('Ctrl Pts',(-4.77058984348464,3.82646117886875,10.821969411815));
#7230=CARTESIAN_POINT('Ctrl Pts',(-4.8725551399554,3.69188731824174,10.8296645439257));
#7231=CARTESIAN_POINT('Ctrl Pts',(-4.97491305229397,3.55679528295234,10.8373893060289));
#7232=CARTESIAN_POINT('Ctrl Pts',(-5.0716674698435,3.41741987844759,10.8451140681321));
#7233=CARTESIAN_POINT('Ctrl Pts',(-5.16247311774284,3.2742475274607,10.8528388302353));
#7234=CARTESIAN_POINT('Ctrl Pts',(-5.25326105229573,3.13110310492886,10.8605620854786));
#7235=CARTESIAN_POINT('Ctrl Pts',(-5.33810236300809,2.98416348128143,10.8682853407219));
#7236=CARTESIAN_POINT('Ctrl Pts',(-5.41669552265323,2.83394339699445,10.8760085959652));
#7237=CARTESIAN_POINT('Ctrl Pts',(-5.49529171954659,2.68371750742258,10.8837321496752));
#7238=CARTESIAN_POINT('Ctrl Pts',(-5.56763913176966,2.53021118249997,10.8914557033853));
#7239=CARTESIAN_POINT('Ctrl Pts',(-5.63348219535846,2.3739637564797,10.8991792570953));
#7240=CARTESIAN_POINT('Ctrl Pts',(-5.69932083662819,2.21772682474591,10.9069022920564));
#7241=CARTESIAN_POINT('Ctrl Pts',(-5.75865588041691,2.05874945242341,10.9146253270175));
#7242=CARTESIAN_POINT('Ctrl Pts',(-5.81127985446346,1.89759110864463,10.9223483619787));
#7243=CARTESIAN_POINT('Ctrl Pts',(-5.86391781366978,1.73638993599882,10.930073449386));
#7244=CARTESIAN_POINT('Ctrl Pts',(-5.90984103873066,1.57300693450831,10.9377985367934));
#7245=CARTESIAN_POINT('Ctrl Pts',(-5.9488916105406,1.40801781541984,10.9455236242007));
#7246=CARTESIAN_POINT('Ctrl Pts',(-5.9877907573374,1.24366846876924,10.9532187563114));
#7247=CARTESIAN_POINT('Ctrl Pts',(-6.01987041528838,1.07772574956919,10.9609138884221));
#7248=CARTESIAN_POINT('Ctrl Pts',(-6.04502473326368,0.910769749569233,10.9686090205329));
#7249=CARTESIAN_POINT('Ctrl Pts',(-6.07131356640451,0.73628366609961,10.9766512200572));
#7250=CARTESIAN_POINT('Ctrl Pts',(-6.09004507716572,0.560647910903114,10.9846934195815));
#7251=CARTESIAN_POINT('Ctrl Pts',(-6.10114591531853,0.3845049837025,10.9927356191058));
#7252=CARTESIAN_POINT('Ctrl Pts',(-6.10920854597905,0.256570917289429,10.9985767352062));
#7253=CARTESIAN_POINT('Ctrl Pts',(-6.11324688458893,0.128369490857254,11.0044178513067));
#7254=CARTESIAN_POINT('Ctrl Pts',(-6.1132499981976,0.000148448865220258,
11.0102589674072));
#7255=CARTESIAN_POINT('Ctrl Pts',(-6.11324999819761,0.000148448155509828,
11.0102589674395));
#7256=CARTESIAN_POINT('Ctrl Pts',(-6.11325432008344,-0.177831321518247,
11.0183668449145));
#7257=CARTESIAN_POINT('Ctrl Pts',(-6.1054808407098,-0.355826038601997,11.0264747223896));
#7258=CARTESIAN_POINT('Ctrl Pts',(-6.08995748975051,-0.533144760390352,
11.0345825998646));
#7259=CARTESIAN_POINT('Ctrl Pts',(-6.07519299148024,-0.701795328685575,
11.0422941270516));
#7260=CARTESIAN_POINT('Ctrl Pts',(-6.05341828534077,-0.869834073479806,
11.0500056542386));
#7261=CARTESIAN_POINT('Ctrl Pts',(-6.02471068005017,-1.03667101058602,11.0577171814256));
#7262=CARTESIAN_POINT('Ctrl Pts',(-5.99600293607759,-1.20350875365554,11.0654287458658));
#7263=CARTESIAN_POINT('Ctrl Pts',(-5.96036228338477,-1.36914436384791,11.073140310306));
#7264=CARTESIAN_POINT('Ctrl Pts',(-5.91791733732643,-1.5329970486179,11.0808518747462));
#7265=CARTESIAN_POINT('Ctrl Pts',(-5.87546318887851,-1.69688525790565,11.0885651111127));
#7266=CARTESIAN_POINT('Ctrl Pts',(-5.82620188186118,-1.85898946144971,11.0962783474791));
#7267=CARTESIAN_POINT('Ctrl Pts',(-5.77031237251077,-2.01874235259212,11.1039915838456));
#7268=CARTESIAN_POINT('Ctrl Pts',(-5.76170925716808,-2.04333323851688,11.1051788882771));
#7269=CARTESIAN_POINT('Ctrl Pts',(-5.75294918397543,-2.06786844275859,11.1063661927086));
#7270=CARTESIAN_POINT('Ctrl Pts',(-5.74403290914135,-2.09234593248851,11.1075534971401));
#7271=CARTESIAN_POINT('Ctrl Pts',(-5.68602242748835,-2.25159976834616,11.1152782592433));
#7272=CARTESIAN_POINT('Ctrl Pts',(-5.62137460129056,-2.40846779971063,11.1230030213465));
#7273=CARTESIAN_POINT('Ctrl Pts',(-5.55031093176515,-2.56239616828239,11.1307277834497));
#7274=CARTESIAN_POINT('Ctrl Pts',(-5.47926112454274,-2.71629451023577,11.138451038693));
#7275=CARTESIAN_POINT('Ctrl Pts',(-5.40179810400514,-2.86725404603998,11.1461742939363));
#7276=CARTESIAN_POINT('Ctrl Pts',(-5.31819088558314,-3.0147423218246,11.1538975491796));
#7277=CARTESIAN_POINT('Ctrl Pts',(-5.23458043614362,-3.16223629732286,11.1616211028896));
#7278=CARTESIAN_POINT('Ctrl Pts',(-5.14482546652191,-3.30625846670951,11.1693446565997));
#7279=CARTESIAN_POINT('Ctrl Pts',(-5.04924057866619,-3.44630166138292,11.1770682103097));
#7280=CARTESIAN_POINT('Ctrl Pts',(-4.95366211072529,-3.58633545011988,11.1847912452708));
#7281=CARTESIAN_POINT('Ctrl Pts',(-4.85225468682151,-3.72239053715926,11.192514280232));
#7282=CARTESIAN_POINT('Ctrl Pts',(-4.74537590292885,-3.85398924523697,11.2002373151931));
#7283=CARTESIAN_POINT('Ctrl Pts',(-4.63846871531182,-3.98562292651792,11.2079624026004));
#7284=CARTESIAN_POINT('Ctrl Pts',(-4.52608746041239,-4.1127976147355,11.2156874900078));
#7285=CARTESIAN_POINT('Ctrl Pts',(-4.40863024977982,-4.23506846263744,11.2234125774151));
#7286=CARTESIAN_POINT('Ctrl Pts',(-4.29162849879485,-4.35686518522179,11.2311077095258));
#7287=CARTESIAN_POINT('Ctrl Pts',(-4.16959032732782,-4.47379582797459,11.2388028416365));
#7288=CARTESIAN_POINT('Ctrl Pts',(-4.04294575943689,-4.58545691820906,11.2464979737472));
#7289=CARTESIAN_POINT('Ctrl Pts',(-3.91581354850853,-4.69754795782161,11.2542227358504));
#7290=CARTESIAN_POINT('Ctrl Pts',(-3.78399435071139,-4.80436846048071,11.2619474979536));
#7291=CARTESIAN_POINT('Ctrl Pts',(-3.64794765405522,-4.90553804141534,11.2696722600568));
#7292=CARTESIAN_POINT('Ctrl Pts',(-3.51192749586135,-5.00668788732386,11.2773955153001));
#7293=CARTESIAN_POINT('Ctrl Pts',(-3.3716817384477,-5.1021888220238,11.2851187705434));
#7294=CARTESIAN_POINT('Ctrl Pts',(-3.22770135279048,-5.19170198872147,11.2928420257868));
#7295=CARTESIAN_POINT('Ctrl Pts',(-3.08371540298281,-5.28121861467317,11.3005655794968));
#7296=CARTESIAN_POINT('Ctrl Pts',(-2.93599480317987,-5.36474683888825,11.3082891332069));
#7297=CARTESIAN_POINT('Ctrl Pts',(-2.78505845785681,-5.4419918181508,11.3160126869169));
#7298=CARTESIAN_POINT('Ctrl Pts',(-2.63413225010372,-5.51923160928996,11.323735721878));
#7299=CARTESIAN_POINT('Ctrl Pts',(-2.47999101120721,-5.59018885559742,11.3314587568391));
#7300=CARTESIAN_POINT('Ctrl Pts',(-2.32317729030046,-5.65461518056996,11.3391817918003));
#7301=CARTESIAN_POINT('Ctrl Pts',(-2.16632189513849,-5.71905862725286,11.3469068792076));
#7302=CARTESIAN_POINT('Ctrl Pts',(-2.00679289128386,-5.77696756184149,11.354631966615));
#7303=CARTESIAN_POINT('Ctrl Pts',(-1.84515269881625,-5.8281418205592,11.3623570540223));
#7304=CARTESIAN_POINT('Ctrl Pts',(-1.68413929277372,-5.87911764267406,11.370052186133));
#7305=CARTESIAN_POINT('Ctrl Pts',(-1.52103134933433,-5.92341086220521,11.3777473182437));
#7306=CARTESIAN_POINT('Ctrl Pts',(-1.3563995169827,-5.96087291533959,11.3854424503544));
#7307=CARTESIAN_POINT('Ctrl Pts',(-1.19113377219271,-5.99847921555614,11.3931672124576));
#7308=CARTESIAN_POINT('Ctrl Pts',(-1.02427384089955,-6.02921492809192,11.4008919745608));
#7309=CARTESIAN_POINT('Ctrl Pts',(-0.856405198718806,-6.05296585965156,
11.408616736664));
#7310=CARTESIAN_POINT('Ctrl Pts',(-0.688569302468551,-6.07671215814607,
11.4163399919073));
#7311=CARTESIAN_POINT('Ctrl Pts',(-0.519725401563922,-6.09347634999393,
11.4240632471506));
#7312=CARTESIAN_POINT('Ctrl Pts',(-0.350466749436321,-6.10319577107269,
11.4317865023939));
#7313=CARTESIAN_POINT('Ctrl Pts',(-0.181201556274503,-6.1129155677604,11.439510056104));
#7314=CARTESIAN_POINT('Ctrl Pts',(-0.011521895986023,-6.11559002677367,
11.447233609814));
#7315=CARTESIAN_POINT('Ctrl Pts',(0.15797550624594,-6.11120849766446,11.454957163524));
#7316=CARTESIAN_POINT('Ctrl Pts',(0.327461524263035,-6.10682726283863,11.4626801984852));
#7317=CARTESIAN_POINT('Ctrl Pts',(0.496764991869067,-6.09539099646342,11.4704032334463));
#7318=CARTESIAN_POINT('Ctrl Pts',(0.665290651923686,-6.07694116402018,11.4781262684074));
#7319=CARTESIAN_POINT('Ctrl Pts',(0.833861098756827,-6.05848642841525,11.4858513558147));
#7320=CARTESIAN_POINT('Ctrl Pts',(1.00165300948352,-6.03301443456494,11.4935764432221));
#7321=CARTESIAN_POINT('Ctrl Pts',(1.16807674414498,-6.00061849164631,11.5013015306295));
#7322=CARTESIAN_POINT('Ctrl Pts',(1.3338551434107,-5.96834816932313,11.5089966627402));
#7323=CARTESIAN_POINT('Ctrl Pts',(1.49827565812717,-5.92920759127325,11.5166917948509));
#7324=CARTESIAN_POINT('Ctrl Pts',(1.66076610969009,-5.88333931465837,11.5243869269616));
#7325=CARTESIAN_POINT('Ctrl Pts',(1.82388062639612,-5.83729487512232,11.532111613201));
#7326=CARTESIAN_POINT('Ctrl Pts',(1.98510798689638,-5.78445462130408,11.5398362994405));
#7327=CARTESIAN_POINT('Ctrl Pts',(2.1438794530364,-5.72499838020486,11.5475609856799));
#7328=CARTESIAN_POINT('Ctrl Pts',(2.30263024492791,-5.66554988113345,11.555284666058));
#7329=CARTESIAN_POINT('Ctrl Pts',(2.45892548300991,-5.59948722248188,11.5630083464361));
#7330=CARTESIAN_POINT('Ctrl Pts',(2.61221414498486,-5.52703924567585,11.5707320268142));
#7331=CARTESIAN_POINT('Ctrl Pts',(2.76548164713755,-5.45460126952017,11.5784546410227));
#7332=CARTESIAN_POINT('Ctrl Pts',(2.91574311557921,-5.37577987086759,11.5861772552312));
#7333=CARTESIAN_POINT('Ctrl Pts',(3.06246964751821,-5.29085108659559,11.5938998694397));
#7334=CARTESIAN_POINT('Ctrl Pts',(3.20920613520849,-5.20591653969945,11.6016230076464));
#7335=CARTESIAN_POINT('Ctrl Pts',(3.35240693209947,-5.11487393661046,11.609346145853));
#7336=CARTESIAN_POINT('Ctrl Pts',(3.49156914352686,-5.01804448749422,11.6170692840597));
#7337=CARTESIAN_POINT('Ctrl Pts',(3.56999849375895,-4.96347313008603,11.6214219075563));
#7338=CARTESIAN_POINT('Ctrl Pts',(3.6471455837845,-4.90706452856059,11.6257745310529));
#7339=CARTESIAN_POINT('Ctrl Pts',(3.72292453512038,-4.84888218750453,11.6301271545495));
#7340=CARTESIAN_POINT('',(-6.11324999809968,0.000152427850000879,10.8647410325957));
#7341=CARTESIAN_POINT('Ctrl Pts',(-6.11324999809968,0.000152427850000879,
10.8647410325958));
#7342=CARTESIAN_POINT('Ctrl Pts',(-6.11325420804908,-0.168691212844257,
10.8724343082978));
#7343=CARTESIAN_POINT('Ctrl Pts',(-6.10625906233778,-0.337560295901734,
10.8801275839998));
#7344=CARTESIAN_POINT('Ctrl Pts',(-6.09228430785177,-0.505863098874644,
10.8878208597019));
#7345=CARTESIAN_POINT('Ctrl Pts',(-6.07830951280065,-0.674166390387332,
10.8955141577355));
#7346=CARTESIAN_POINT('Ctrl Pts',(-6.05735509004427,-0.84190307733042,10.9032074557691));
#7347=CARTESIAN_POINT('Ctrl Pts',(-6.02949277637401,-1.00848521166826,10.9109007538028));
#7348=CARTESIAN_POINT('Ctrl Pts',(-6.00163240587938,-1.17505572822209,10.9185935152898));
#7349=CARTESIAN_POINT('Ctrl Pts',(-5.96686516142572,-1.340471535738,10.9262862767769));
#7350=CARTESIAN_POINT('Ctrl Pts',(-5.92531418314416,-1.50415338098566,10.933979038264));
#7351=CARTESIAN_POINT('Ctrl Pts',(-5.88375244490362,-1.66787761295956,10.9416737918533));
#7352=CARTESIAN_POINT('Ctrl Pts',(-5.83540354042846,-1.82986667285239,10.9493685454426));
#7353=CARTESIAN_POINT('Ctrl Pts',(-5.78044114402197,-1.98955415683966,10.957063299032));
#7354=CARTESIAN_POINT('Ctrl Pts',(-5.73389279409895,-2.12479551036418,10.9635800833439));
#7355=CARTESIAN_POINT('Ctrl Pts',(-5.68260173604348,-2.25838616153482,10.9700968676558));
#7356=CARTESIAN_POINT('Ctrl Pts',(-5.62670098309795,-2.38999196846026,10.9766136519677));
#7357=CARTESIAN_POINT('Ctrl Pts',(-5.5604382379733,-2.54599276597585,10.9843384140709));
#7358=CARTESIAN_POINT('Ctrl Pts',(-5.48767205651953,-2.69926377932432,10.9920631761741));
#7359=CARTESIAN_POINT('Ctrl Pts',(-5.40865261290302,-2.84926349701766,10.9997879382773));
#7360=CARTESIAN_POINT('Ctrl Pts',(-5.32964858351237,-2.99923395445022,11.0075111935207));
#7361=CARTESIAN_POINT('Ctrl Pts',(-5.24439387355246,-3.14593410929278,11.015234448764));
#7362=CARTESIAN_POINT('Ctrl Pts',(-5.15318498651466,-3.288846310982,11.0229577040073));
#7363=CARTESIAN_POINT('Ctrl Pts',(-5.06197257469154,-3.43176403554126,11.0306812577174));
#7364=CARTESIAN_POINT('Ctrl Pts',(-4.96480569250414,-3.57089324474132,11.0384048114274));
#7365=CARTESIAN_POINT('Ctrl Pts',(-4.86202504467805,-3.70574392361687,11.0461283651375));
#7366=CARTESIAN_POINT('Ctrl Pts',(-4.75925130006677,-3.84058554530878,11.0538514000986));
#7367=CARTESIAN_POINT('Ctrl Pts',(-4.6508647364867,-3.97114895966124,11.0615744350597));
#7368=CARTESIAN_POINT('Ctrl Pts',(-4.53724745090694,-4.09697585198381,11.0692974700209));
#7369=CARTESIAN_POINT('Ctrl Pts',(-4.42359997080255,-4.22283618361256,11.0770225574282));
#7370=CARTESIAN_POINT('Ctrl Pts',(-4.30471920187486,-4.34395724105177,11.0847476448356));
#7371=CARTESIAN_POINT('Ctrl Pts',(-4.18102598361013,-4.45991561432242,11.0924727322429));
#7372=CARTESIAN_POINT('Ctrl Pts',(-4.05781240613828,-4.57542433993351,11.1001678643536));
#7373=CARTESIAN_POINT('Ctrl Pts',(-3.92982388491662,-4.6858101585198,11.1078629964643));
#7374=CARTESIAN_POINT('Ctrl Pts',(-3.79751096363715,-4.79069264757777,11.115558128575));
#7375=CARTESIAN_POINT('Ctrl Pts',(-3.66468857340899,-4.89597898511039,11.1232828906782));
#7376=CARTESIAN_POINT('Ctrl Pts',(-3.52746135454797,-4.9957567937649,11.1310076527814));
#7377=CARTESIAN_POINT('Ctrl Pts',(-3.38630806645332,-5.08967024880524,11.1387324148845));
#7378=CARTESIAN_POINT('Ctrl Pts',(-3.24518231295707,-5.18356538426334,11.1464556701279));
#7379=CARTESIAN_POINT('Ctrl Pts',(-3.10013228208042,-5.2715982732535,11.1541789253712));
#7380=CARTESIAN_POINT('Ctrl Pts',(-2.95166600044813,-5.3534562092445,11.1619021806146));
#7381=CARTESIAN_POINT('Ctrl Pts',(-2.80319398130754,-5.43531730865135,11.1696257343246));
#7382=CARTESIAN_POINT('Ctrl Pts',(-2.6513057228446,-5.51100282105464,11.1773492880347));
#7383=CARTESIAN_POINT('Ctrl Pts',(-2.49653484426342,-5.5802454546264,11.1850728417447));
#7384=CARTESIAN_POINT('Ctrl Pts',(-2.3417743607967,-5.64948343754871,11.1927958767058));
#7385=CARTESIAN_POINT('Ctrl Pts',(-2.18413193398178,-5.71227927817567,11.200518911667));
#7386=CARTESIAN_POINT('Ctrl Pts',(-2.02416236429372,-5.76841332477804,11.2082419466281));
#7387=CARTESIAN_POINT('Ctrl Pts',(-1.86415028166353,-5.82456228936437,11.2159670340355));
#7388=CARTESIAN_POINT('Ctrl Pts',(-1.70181011887905,-5.87404581513944,11.2236921214428));
#7389=CARTESIAN_POINT('Ctrl Pts',(-1.53771399779626,-5.91669343666557,11.2314172088502));
#7390=CARTESIAN_POINT('Ctrl Pts',(-1.37425418640611,-5.95917568502648,11.2391123409608));
#7391=CARTESIAN_POINT('Ctrl Pts',(-1.20905232080402,-5.99487490225665,11.2468074730715));
#7392=CARTESIAN_POINT('Ctrl Pts',(-1.04268604041893,-6.02367258270364,11.2545026051821));
#7393=CARTESIAN_POINT('Ctrl Pts',(-0.875679169128143,-6.05258114819389,
11.2622273672853));
#7394=CARTESIAN_POINT('Ctrl Pts',(-0.707439744144012,-6.07454513183358,
11.2699521293885));
#7395=CARTESIAN_POINT('Ctrl Pts',(-0.538558413553295,-6.08948112713152,
11.2776768914917));
#7396=CARTESIAN_POINT('Ctrl Pts',(-0.369710026436769,-6.10441420888316,
11.285400146735));
#7397=CARTESIAN_POINT('Ctrl Pts',(-0.200220299066371,-6.11232200990819,
11.2931234019784));
#7398=CARTESIAN_POINT('Ctrl Pts',(-0.0306849508333739,-6.11317298923336,
11.3008466572217));
#7399=CARTESIAN_POINT('Ctrl Pts',(0.138856949126425,-6.1140240014448,11.3085702109317));
#7400=CARTESIAN_POINT('Ctrl Pts',(0.308444156582704,-6.10781764069055,11.3162937646418));
#7401=CARTESIAN_POINT('Ctrl Pts',(0.477480206354419,-6.09457449007227,11.3240173183518));
#7402=CARTESIAN_POINT('Ctrl Pts',(0.646504902897834,-6.0813322289241,11.3317403533129));
#7403=CARTESIAN_POINT('Ctrl Pts',(0.814978199847684,-6.06105414847014,11.3394633882741));
#7404=CARTESIAN_POINT('Ctrl Pts',(0.98230782461247,-6.03381279956589,11.3471864232352));
#7405=CARTESIAN_POINT('Ctrl Pts',(1.14968191830179,-6.00656421109787,11.3549115106425));
#7406=CARTESIAN_POINT('Ctrl Pts',(1.31591141908453,-5.97234870517448,11.3626365980499));
#7407=CARTESIAN_POINT('Ctrl Pts',(1.48041237617283,-5.93129031147307,11.3703616854573));
#7408=CARTESIAN_POINT('Ctrl Pts',(1.64427545375064,-5.8903911284446,11.3780568175679));
#7409=CARTESIAN_POINT('Ctrl Pts',(1.80642307413885,-5.84270213902499,11.3857519496786));
#7410=CARTESIAN_POINT('Ctrl Pts',(1.96629130050559,-5.78839563990369,11.3934470817893));
#7411=CARTESIAN_POINT('Ctrl Pts',(2.12678130988935,-5.73387792395942,11.4011721429395));
#7412=CARTESIAN_POINT('Ctrl Pts',(2.28503099222204,-5.67267178152857,11.4088972040896));
#7413=CARTESIAN_POINT('Ctrl Pts',(2.44048171537531,-5.60498657977152,11.4166222652398));
#7414=CARTESIAN_POINT('Ctrl Pts',(2.59589888624497,-5.53731598710112,11.4243456590227));
#7415=CARTESIAN_POINT('Ctrl Pts',(2.74851801325822,-5.4631692526716,11.4320690528057));
#7416=CARTESIAN_POINT('Ctrl Pts',(2.89780086164218,-5.38280370520474,11.4397924465886));
#7417=CARTESIAN_POINT('Ctrl Pts',(3.04708476294043,-5.30243759090763,11.4475158948458));
#7418=CARTESIAN_POINT('Ctrl Pts',(3.19303205762039,-5.21585272257969,11.455239343103));
#7419=CARTESIAN_POINT('Ctrl Pts',(3.33512884395811,-5.12335253097995,11.4629627913602));
#7420=CARTESIAN_POINT('Ctrl Pts',(3.46788730481097,-5.03693127275254,11.4701786695621));
#7421=CARTESIAN_POINT('Ctrl Pts',(3.59728477563354,-4.94534717161686,11.477394547764));
#7422=CARTESIAN_POINT('Ctrl Pts',(3.72292453512039,-4.84888218750453,11.484610425966));
#7423=CARTESIAN_POINT('Ctrl Pts',(3.72292453512039,-4.84888218750452,9.73461637809168));
#7424=CARTESIAN_POINT('Ctrl Pts',(3.85736574640416,-4.74565953439295,9.74234051282505));
#7425=CARTESIAN_POINT('Ctrl Pts',(3.98753222395988,-4.63682608808731,9.75006464755842));
#7426=CARTESIAN_POINT('Ctrl Pts',(4.112962928074,-4.52276038662109,9.75778878229179));
#7427=CARTESIAN_POINT('Ctrl Pts',(4.23837298429734,-4.40871346218528,9.76551164550961));
#7428=CARTESIAN_POINT('Ctrl Pts',(4.35904858845556,-4.28943621450911,9.77323450872743));
#7429=CARTESIAN_POINT('Ctrl Pts',(4.47456347729856,-4.16534599404729,9.78095737194525));
#7430=CARTESIAN_POINT('Ctrl Pts',(4.59008473161228,-4.04124893556941,9.78868066073298));
#7431=CARTESIAN_POINT('Ctrl Pts',(4.70044448374109,-3.91233860380513,9.7964039495207));
#7432=CARTESIAN_POINT('Ctrl Pts',(4.80525437749419,-3.7790681298533,9.80412723830842));
#7433=CARTESIAN_POINT('Ctrl Pts',(4.910060430352,-3.64580253977185,9.81185024406615));
#7434=CARTESIAN_POINT('Ctrl Pts',(5.00931683705915,-3.50817737726526,9.81957324982388));
#7435=CARTESIAN_POINT('Ctrl Pts',(5.1026763534931,-3.36667782747361,9.82729625558161));
#7436=CARTESIAN_POINT('Ctrl Pts',(5.19605783455074,-3.22514498718856,9.83502107832513));
#7437=CARTESIAN_POINT('Ctrl Pts',(5.28353947846812,-3.07973620280037,9.84274590106866));
#7438=CARTESIAN_POINT('Ctrl Pts',(5.36481763811116,-2.93096524583821,9.85047072381218));
#7439=CARTESIAN_POINT('Ctrl Pts',(5.41597798725634,-2.83732171190149,9.85533309557822));
#7440=CARTESIAN_POINT('Ctrl Pts',(5.46468137364533,-2.74234662089777,9.86019546734425));
#7441=CARTESIAN_POINT('Ctrl Pts',(5.51086141100289,-2.64617309925469,9.86505783911028));
#7442=CARTESIAN_POINT('Ctrl Pts',(5.58422680132456,-2.49338396443177,9.87278260121348));
#7443=CARTESIAN_POINT('Ctrl Pts',(5.65124712872478,-2.33751480002962,9.88050736331668));
#7444=CARTESIAN_POINT('Ctrl Pts',(5.71168104348704,-2.17911110776178,9.88823212541987));
#7445=CARTESIAN_POINT('Ctrl Pts',(5.77210316947964,-2.020738315108,9.8959553806632));
#7446=CARTESIAN_POINT('Ctrl Pts',(5.82594133357522,-1.85983227703631,9.90367863590652));
#7447=CARTESIAN_POINT('Ctrl Pts',(5.87300270167234,-1.69695752116821,9.91140189114985));
#7448=CARTESIAN_POINT('Ctrl Pts',(5.92006588846532,-1.53407647097304,9.9191254448599));
#7449=CARTESIAN_POINT('Ctrl Pts',(5.96035166342292,-1.3692268541014,9.92684899856995));
#7450=CARTESIAN_POINT('Ctrl Pts',(5.99371713664409,-1.20298813310812,9.93457255227999));
#7451=CARTESIAN_POINT('Ctrl Pts',(6.02708036888863,-1.03676057746192,9.94229558724112));
#7452=CARTESIAN_POINT('Ctrl Pts',(6.05352416716979,-0.869144415160902,9.95001862220223));
#7453=CARTESIAN_POINT('Ctrl Pts',(6.07295678239129,-0.700729249930136,9.95774165716336));
#7454=CARTESIAN_POINT('Ctrl Pts',(6.09239456195533,-0.532269327285528,9.96546674457071));
#7455=CARTESIAN_POINT('Ctrl Pts',(6.10481739668134,-0.363010292213752,9.97319183197807));
#7456=CARTESIAN_POINT('Ctrl Pts',(6.11018533417448,-0.193547783606798,9.98091691938543));
#7457=CARTESIAN_POINT('Ctrl Pts',(6.11553245660733,-0.0247423937419612,
9.98861205149611));
#7458=CARTESIAN_POINT('Ctrl Pts',(6.11387931993266,0.144264581405888,9.9963071836068));
#7459=CARTESIAN_POINT('Ctrl Pts',(6.10523786759826,0.312883592641504,10.0040023157175));
#7460=CARTESIAN_POINT('Ctrl Pts',(6.0965631414793,0.48215186888887,10.0117270778207));
#7461=CARTESIAN_POINT('Ctrl Pts',(6.08084307374087,0.65108913584488,10.0194518399239));
#7462=CARTESIAN_POINT('Ctrl Pts',(6.05812671286995,0.819100905451548,10.0271766020271));
#7463=CARTESIAN_POINT('Ctrl Pts',(6.03541478325168,0.987079901208335,10.0348998572704));
#7464=CARTESIAN_POINT('Ctrl Pts',(6.00570932612104,1.15413344597106,10.0426231125137));
#7465=CARTESIAN_POINT('Ctrl Pts',(5.9691110953439,1.31967355582444,10.050346367757));
#7466=CARTESIAN_POINT('Ctrl Pts',(5.93251145022092,1.48522006300799,10.0580699214671));
#7467=CARTESIAN_POINT('Ctrl Pts',(5.88901856296916,1.64925270794545,10.0657934751771));
#7468=CARTESIAN_POINT('Ctrl Pts',(5.83878419006957,1.81119428673283,10.0735170288872));
#7469=CARTESIAN_POINT('Ctrl Pts',(5.78855319113848,1.97312498878872,10.0812400638483));
#7470=CARTESIAN_POINT('Ctrl Pts',(5.73158170657638,2.13296460302393,10.0889630988094));
#7471=CARTESIAN_POINT('Ctrl Pts',(5.66807125277237,2.29015148756484,10.0966861337705));
#7472=CARTESIAN_POINT('Ctrl Pts',(5.60454392065661,2.44738014553172,10.1044112211779));
#7473=CARTESIAN_POINT('Ctrl Pts',(5.53447426359638,2.60195437021206,10.1121363085853));
#7474=CARTESIAN_POINT('Ctrl Pts',(5.45811216941679,2.75333200115139,10.1198613959926));
#7475=CARTESIAN_POINT('Ctrl Pts',(5.3820461818139,2.90412264043515,10.1275565281033));
#7476=CARTESIAN_POINT('Ctrl Pts',(5.29973663965096,3.05174116833154,10.135251660214));
#7477=CARTESIAN_POINT('Ctrl Pts',(5.21147608835822,3.19567560039665,10.1429467923246));
#7478=CARTESIAN_POINT('Ctrl Pts',(5.12287569111643,3.34016424986636,10.1506715544278));
#7479=CARTESIAN_POINT('Ctrl Pts',(5.02824696000459,3.48099153395726,10.158396316531));
#7480=CARTESIAN_POINT('Ctrl Pts',(4.92791738625288,3.61765888341708,10.1661210786342));
#7481=CARTESIAN_POINT('Ctrl Pts',(4.82760738366812,3.7542995733446,10.1738443338775));
#7482=CARTESIAN_POINT('Ctrl Pts',(4.72159894482899,3.88678169250037,10.1815675891209));
#7483=CARTESIAN_POINT('Ctrl Pts',(4.61026185303658,4.01463712045506,10.1892908443642));
#7484=CARTESIAN_POINT('Ctrl Pts',(4.49892045860029,4.14249748940799,10.1970143980743));
#7485=CARTESIAN_POINT('Ctrl Pts',(4.38225020427461,4.26573056776866,10.2047379517843));
#7486=CARTESIAN_POINT('Ctrl Pts',(4.26066050261565,4.38390210245974,10.2124615054943));
#7487=CARTESIAN_POINT('Ctrl Pts',(4.13907896747297,4.50206570021416,10.2201845404555));
#7488=CARTESIAN_POINT('Ctrl Pts',(4.01257887350575,4.61516821370677,10.2279075754166));
#7489=CARTESIAN_POINT('Ctrl Pts',(3.88160588341402,4.72281286188069,10.2356306103777));
#7490=CARTESIAN_POINT('Ctrl Pts',(3.75059808640744,4.83048611731249,10.2433556977851));
#7491=CARTESIAN_POINT('Ctrl Pts',(3.61511526159468,4.93269840599053,10.2510807851924));
#7492=CARTESIAN_POINT('Ctrl Pts',(3.47563622741577,5.02909319631035,10.2588058725998));
#7493=CARTESIAN_POINT('Ctrl Pts',(3.33669804612664,5.12511419998037,10.2665010047105));
#7494=CARTESIAN_POINT('Ctrl Pts',(3.19379486744877,5.21536259073196,10.2741961368212));
#7495=CARTESIAN_POINT('Ctrl Pts',(3.0474285314929,5.29952874394913,10.2818912689319));
#7496=CARTESIAN_POINT('Ctrl Pts',(2.9004986141226,5.38401897769593,10.2896160310351));
#7497=CARTESIAN_POINT('Ctrl Pts',(2.75002676368807,5.46240993969483,10.2973407931383));
#7498=CARTESIAN_POINT('Ctrl Pts',(2.59653908889921,5.53442050465254,10.3050655552415));
#7499=CARTESIAN_POINT('Ctrl Pts',(2.44308135476278,5.60641702259767,10.3127888104848));
#7500=CARTESIAN_POINT('Ctrl Pts',(2.28660925687176,5.67203549242728,10.3205120657281));
#7501=CARTESIAN_POINT('Ctrl Pts',(2.12767147410012,5.73104176051794,10.3282353209715));
#7502=CARTESIAN_POINT('Ctrl Pts',(1.96872754914669,5.79005030891742,10.3359588746815));
#7503=CARTESIAN_POINT('Ctrl Pts',(1.80731804436292,5.84244603023263,10.3436824283916));
#7504=CARTESIAN_POINT('Ctrl Pts',(1.64401023497448,5.88804347044068,10.3514059821016));
#7505=CARTESIAN_POINT('Ctrl Pts',(1.48071339407973,5.9336378481177,10.3591290170627));
#7506=CARTESIAN_POINT('Ctrl Pts',(1.31551880900891,5.97243477319408,10.3668520520239));
#7507=CARTESIAN_POINT('Ctrl Pts',(1.14900765947488,6.00429903993531,10.374575086985));
#7508=CARTESIAN_POINT('Ctrl Pts',(0.982452258531474,6.03617177481044,10.3823001743923));
#7509=CARTESIAN_POINT('Ctrl Pts',(0.814579905056783,6.06110810804048,10.3900252617997));
#7510=CARTESIAN_POINT('Ctrl Pts',(0.645981637169343,6.07902404066146,10.3977503492071));
#7511=CARTESIAN_POINT('Ctrl Pts',(0.478037136789328,6.09687050130768,10.4054454813177));
#7512=CARTESIAN_POINT('Ctrl Pts',(0.309372655541613,6.10775090914417,10.4131406134284));
#7513=CARTESIAN_POINT('Ctrl Pts',(0.140577005799611,6.11163346969862,10.420835745539));
#7514=CARTESIAN_POINT('Ctrl Pts',(-0.0288685890988558,6.11553097999515,
10.4285605076422));
#7515=CARTESIAN_POINT('Ctrl Pts',(-0.198506377900037,6.11237799618206,10.4362852697454));
#7516=CARTESIAN_POINT('Ctrl Pts',(-0.367739872249517,6.10217936059388,10.4440100318486));
#7517=CARTESIAN_POINT('Ctrl Pts',(-0.536940354428697,6.09198271444104,10.4517332870919));
#7518=CARTESIAN_POINT('Ctrl Pts',(-0.705736383360155,6.07474317795971,10.4594565423353));
#7519=CARTESIAN_POINT('Ctrl Pts',(-0.873534123859799,6.05051763876055,10.4671797975786));
#7520=CARTESIAN_POINT('Ctrl Pts',(-1.04133834893615,6.02629116336065,10.4749033512886));
#7521=CARTESIAN_POINT('Ctrl Pts',(-1.20814389414981,5.99507818636999,10.4826269049987));
#7522=CARTESIAN_POINT('Ctrl Pts',(-1.37336389368796,5.95698725682826,10.4903504587087));
#7523=CARTESIAN_POINT('Ctrl Pts',(-1.53857279630091,5.91889888564627,10.4980734936698));
#7524=CARTESIAN_POINT('Ctrl Pts',(-1.70219605749311,5.87393355757187,10.5057965286309));
#7525=CARTESIAN_POINT('Ctrl Pts',(-1.86365864180932,5.82225059829182,10.5135195635921));
#7526=CARTESIAN_POINT('Ctrl Pts',(-2.02516413584634,5.77055390393275,10.5212446509994));
#7527=CARTESIAN_POINT('Ctrl Pts',(-2.18450750287111,5.71213610560674,10.5289697384068));
#7528=CARTESIAN_POINT('Ctrl Pts',(-2.34112954932161,5.64720621155215,10.5366948258141));
#7529=CARTESIAN_POINT('Ctrl Pts',(-2.49714426803351,5.58252809383823,10.5443899579248));
#7530=CARTESIAN_POINT('Ctrl Pts',(-2.65045845734697,5.51138844339849,10.5520850900355));
#7531=CARTESIAN_POINT('Ctrl Pts',(-2.80053985434043,5.43404104573667,10.5597802221462));
#7532=CARTESIAN_POINT('Ctrl Pts',(-2.95119913753571,5.35639582306288,10.5675049842494));
#7533=CARTESIAN_POINT('Ctrl Pts',(-3.09865402863322,5.27246742627327,10.5752297463526));
#7534=CARTESIAN_POINT('Ctrl Pts',(-3.24238305235198,5.18254548502188,10.5829545084558));
#7535=CARTESIAN_POINT('Ctrl Pts',(-3.38608403902615,5.09264108473341,10.5906777636991));
#7536=CARTESIAN_POINT('Ctrl Pts',(-3.52606034003548,4.99674564085416,10.5984010189424));
#7537=CARTESIAN_POINT('Ctrl Pts',(-3.66181770989931,4.89519321599952,10.6061242741858));
#7538=CARTESIAN_POINT('Ctrl Pts',(-3.79758032613371,4.79363686663122,10.6138478278958));
#7539=CARTESIAN_POINT('Ctrl Pts',(-3.92912342882153,4.68642328548612,10.6215713816059));
#7540=CARTESIAN_POINT('Ctrl Pts',(-4.05598360880754,4.57392856607802,10.6292949353159));
#7541=CARTESIAN_POINT('Ctrl Pts',(-4.18283526828806,4.46144140232588,10.637017970277));
#7542=CARTESIAN_POINT('Ctrl Pts',(-4.3050043973426,4.34367402043189,10.6447410052382));
#7543=CARTESIAN_POINT('Ctrl Pts',(-4.42206226839468,4.22104144222016,10.6524640401993));
#7544=CARTESIAN_POINT('Ctrl Pts',(-4.53915124832916,4.09837627361174,10.6601891276067));
#7545=CARTESIAN_POINT('Ctrl Pts',(-4.65112603538813,3.97084355295081,10.667914215014));
#7546=CARTESIAN_POINT('Ctrl Pts',(-4.75759558276085,3.83889435038194,10.6756393024214));
#7547=CARTESIAN_POINT('Ctrl Pts',(-4.86365227695647,3.70745680254293,10.683334434532));
#7548=CARTESIAN_POINT('Ctrl Pts',(-4.96424617955939,3.5716372263821,10.6910295666427));
#7549=CARTESIAN_POINT('Ctrl Pts',(-5.05903131501063,3.43191312772364,10.6987246987534));
#7550=CARTESIAN_POINT('Ctrl Pts',(-5.15418141922566,3.29165102348744,10.7064494608566));
#7551=CARTESIAN_POINT('Ctrl Pts',(-5.24351160883361,3.14740457493227,10.7141742229598));
#7552=CARTESIAN_POINT('Ctrl Pts',(-5.32670253007409,2.99967760244368,10.721898985063));
#7553=CARTESIAN_POINT('Ctrl Pts',(-5.40987722336353,2.85197944687454,10.7296222403063));
#7554=CARTESIAN_POINT('Ctrl Pts',(-5.48691488246913,2.70080239808559,10.7373454955496));
#7555=CARTESIAN_POINT('Ctrl Pts',(-5.55754132285721,2.54667626667281,10.7450687507929));
#7556=CARTESIAN_POINT('Ctrl Pts',(-5.62817049261808,2.39254417902511,10.7527923045029));
#7557=CARTESIAN_POINT('Ctrl Pts',(-5.69238781224909,2.23546306715605,10.760515858213));
#7558=CARTESIAN_POINT('Ctrl Pts',(-5.74996628420993,2.07598489709079,10.768239411923));
#7559=CARTESIAN_POINT('Ctrl Pts',(-5.80754088893923,1.91651743830334,10.7759624468841));
#7560=CARTESIAN_POINT('Ctrl Pts',(-5.85847743067887,1.75465354162588,10.7836854818453));
#7561=CARTESIAN_POINT('Ctrl Pts',(-5.90259799113035,1.59096276436752,10.7914085168064));
#7562=CARTESIAN_POINT('Ctrl Pts',(-5.94673027690468,1.42722848523175,10.7991336042137));
#7563=CARTESIAN_POINT('Ctrl Pts',(-5.98404287714979,1.26166666101199,10.8068586916211));
#7564=CARTESIAN_POINT('Ctrl Pts',(-6.014408208602,1.09486047640825,10.8145837790284));
#7565=CARTESIAN_POINT('Ctrl Pts',(-6.04465579348868,0.928701110212442,10.8222789111392));
#7566=CARTESIAN_POINT('Ctrl Pts',(-6.06800986796465,0.76130732981663,10.8299740432499));
#7567=CARTESIAN_POINT('Ctrl Pts',(-6.08439507461123,0.593263970376244,10.8376691753606));
#7568=CARTESIAN_POINT('Ctrl Pts',(-6.10189384394049,0.413800137689429,10.8458872799392));
#7569=CARTESIAN_POINT('Ctrl Pts',(-6.11144867149434,0.23355642126168,10.8541053845179));
#7570=CARTESIAN_POINT('Ctrl Pts',(-6.11301843917963,0.053208314667885,10.8623234890965));
#7571=CARTESIAN_POINT('Ctrl Pts',(-6.11317236687149,0.0355238075657486,
10.8631293369179));
#7572=CARTESIAN_POINT('Ctrl Pts',(-6.11324955711771,0.0178382994096718,
10.8639351847392));
#7573=CARTESIAN_POINT('Ctrl Pts',(-6.11324999809966,0.000152428621332483,
10.8647410325606));
#7574=CARTESIAN_POINT('Origin',(0.,0.,-3.86474103256053));
#7575=CARTESIAN_POINT('',(3.72292453512037,-4.84888218750454,7.98461472294509));
#7576=CARTESIAN_POINT('',(3.72292453512038,-4.84888218750453,8.13013011411225));
#7577=CARTESIAN_POINT('',(3.72292453512038,-4.84888218750453,-3.86474103256053));
#7578=CARTESIAN_POINT('',(-6.11324999816031,-0.000149976428034001,9.26025896747021));
#7579=CARTESIAN_POINT('Ctrl Pts',(3.72292453512038,-4.84888218750453,8.13013011411225));
#7580=CARTESIAN_POINT('Ctrl Pts',(3.8573997599122,-4.74563341915264,8.13785312315989));
#7581=CARTESIAN_POINT('Ctrl Pts',(3.9875736773476,-4.63678976520587,8.14557613220753));
#7582=CARTESIAN_POINT('Ctrl Pts',(4.11299006133295,-4.52273571169888,8.15329914125517));
#7583=CARTESIAN_POINT('Ctrl Pts',(4.23843542662074,-4.40865530250443,8.16102393494095));
#7584=CARTESIAN_POINT('Ctrl Pts',(4.35912082733167,-4.28936230135537,8.16874872862672));
#7585=CARTESIAN_POINT('Ctrl Pts',(4.4746252444227,-4.16527964060939,8.17647352231249));
#7586=CARTESIAN_POINT('Ctrl Pts',(4.54064502664269,-4.09435672314841,8.18088884433803));
#7587=CARTESIAN_POINT('Ctrl Pts',(4.60497284510067,-4.02186970029884,8.18530416636357));
#7588=CARTESIAN_POINT('Ctrl Pts',(4.66753571967432,-3.94790271765457,8.1897194883891));
#7589=CARTESIAN_POINT('Ctrl Pts',(4.77699168229202,-3.81849486447602,8.19744425049228));
#7590=CARTESIAN_POINT('Ctrl Pts',(4.88108194442947,-3.6845092756081,8.20516901259547));
#7591=CARTESIAN_POINT('Ctrl Pts',(4.97943563993126,-3.54641315560982,8.21289377469864));
#7592=CARTESIAN_POINT('Ctrl Pts',(5.07777014969844,-3.4083439738521,8.22061702994196));
#7593=CARTESIAN_POINT('Ctrl Pts',(5.17037014194221,-3.26616611890436,8.22834028518528));
#7594=CARTESIAN_POINT('Ctrl Pts',(5.25690691641525,-3.12037741862191,8.2360635404286));
#7595=CARTESIAN_POINT('Ctrl Pts',(5.34344703511902,-2.97458308430636,8.24378709413865));
#7596=CARTESIAN_POINT('Ctrl Pts',(5.42392330200462,-2.82517789592657,8.2515106478487));
#7597=CARTESIAN_POINT('Ctrl Pts',(5.49805159489902,-2.67268670485868,8.25923420155874));
#7598=CARTESIAN_POINT('Ctrl Pts',(5.57217490900077,-2.52020575579142,8.26695723651986));
#7599=CARTESIAN_POINT('Ctrl Pts',(5.63995096375848,-2.36463950388084,8.27468027148098));
#7600=CARTESIAN_POINT('Ctrl Pts',(5.70114257959357,-2.20653548569816,8.28240330644209));
#7601=CARTESIAN_POINT('Ctrl Pts',(5.7623504574944,-2.04838945035507,8.29012839384946));
#7602=CARTESIAN_POINT('Ctrl Pts',(5.81697028332761,-1.88770459605305,8.29785348125682));
#7603=CARTESIAN_POINT('Ctrl Pts',(5.86481348823859,-1.72504733577798,8.30557856866419));
#7604=CARTESIAN_POINT('Ctrl Pts',(5.91247117325567,-1.56302080577533,8.31327370077489));
#7605=CARTESIAN_POINT('Ctrl Pts',(5.953404641684,-1.39903744786339,8.3209688328856));
#7606=CARTESIAN_POINT('Ctrl Pts',(5.98747708276542,-1.23367084178031,8.32866396499631));
#7607=CARTESIAN_POINT('Ctrl Pts',(6.02168071927778,-1.06766749402391,8.33638872709951));
#7608=CARTESIAN_POINT('Ctrl Pts',(6.04898247149159,-0.900211425091387,8.34411348920271));
#7609=CARTESIAN_POINT('Ctrl Pts',(6.0692801964792,-0.731890332717556,8.35183825130591));
#7610=CARTESIAN_POINT('Ctrl Pts',(6.08957396201447,-0.56360207453292,8.35956150654923));
#7611=CARTESIAN_POINT('Ctrl Pts',(6.10286638859551,-0.394449444057672,8.36728476179255));
#7612=CARTESIAN_POINT('Ctrl Pts',(6.10910701135986,-0.225026856738937,8.37500801703588));
#7613=CARTESIAN_POINT('Ctrl Pts',(6.1153478752943,-0.0555977220509368,8.38273157074592));
#7614=CARTESIAN_POINT('Ctrl Pts',(6.11453637446197,0.11410107379936,8.39045512445596));
#7615=CARTESIAN_POINT('Ctrl Pts',(6.10667411801386,0.283472712760192,8.39817867816601));
#7616=CARTESIAN_POINT('Ctrl Pts',(6.09881238963058,0.452832975953017,8.40590171312713));
#7617=CARTESIAN_POINT('Ctrl Pts',(6.08390086800804,0.621865809612514,8.41362474808825));
#7618=CARTESIAN_POINT('Ctrl Pts',(6.06199323707562,0.789976933935036,8.42134778304937));
#7619=CARTESIAN_POINT('Ctrl Pts',(6.0400797840493,0.958132734870672,8.42907287045674));
#7620=CARTESIAN_POINT('Ctrl Pts',(6.01116654528001,1.12536602222688,8.4367979578641));
#7621=CARTESIAN_POINT('Ctrl Pts',(5.97535892207165,1.29108919711951,8.44452304527146));
#7622=CARTESIAN_POINT('Ctrl Pts',(5.93969014881027,1.45616975315099,8.45221817738213));
#7623=CARTESIAN_POINT('Ctrl Pts',(5.89718046172444,1.61975158898021,8.4599133094928));
#7624=CARTESIAN_POINT('Ctrl Pts',(5.84798414103763,1.78126557499785,8.46760844160348));
#7625=CARTESIAN_POINT('Ctrl Pts',(5.79859839064467,1.94340146823296,8.47533320370668));
#7626=CARTESIAN_POINT('Ctrl Pts',(5.74245689117747,2.10351097055519,8.48305796580988));
#7627=CARTESIAN_POINT('Ctrl Pts',(5.67975112004893,2.26102914107779,8.49078272791308));
#7628=CARTESIAN_POINT('Ctrl Pts',(5.61705758085826,2.41851658472404,8.49850598315641));
#7629=CARTESIAN_POINT('Ctrl Pts',(5.5478024421776,2.57341341092616,8.50622923839974));
#7630=CARTESIAN_POINT('Ctrl Pts',(5.472225775228,2.72517350409664,8.51395249364307));
#7631=CARTESIAN_POINT('Ctrl Pts',(5.3966461876034,2.87693946206544,8.5216760473531));
#7632=CARTESIAN_POINT('Ctrl Pts',(5.31474472058753,3.02556815898231,8.52939960106314));
#7633=CARTESIAN_POINT('Ctrl Pts',(5.2268083224284,3.17053628320087,8.53712315477317));
#7634=CARTESIAN_POINT('Ctrl Pts',(5.13887783047677,3.31549467070244,8.54484618973429));
#7635=CARTESIAN_POINT('Ctrl Pts',(5.04491338291061,3.45679270651908,8.55256922469541));
#7636=CARTESIAN_POINT('Ctrl Pts',(4.94524644182811,3.59393422200329,8.56029225965653));
#7637=CARTESIAN_POINT('Ctrl Pts',(4.84555301361461,3.73111218372783,8.5680173470639));
#7638=CARTESIAN_POINT('Ctrl Pts',(4.74015424828601,3.86413115998052,8.57574243447126));
#7639=CARTESIAN_POINT('Ctrl Pts',(4.6294238259699,3.99252559190824,8.58346752187862));
#7640=CARTESIAN_POINT('Ctrl Pts',(4.51912277907408,4.12042215331384,8.5911626539893));
#7641=CARTESIAN_POINT('Ctrl Pts',(4.40353157874229,4.24372975614234,8.59885778609998));
#7642=CARTESIAN_POINT('Ctrl Pts',(4.28305799071617,4.36202244499755,8.60655291821066));
#7643=CARTESIAN_POINT('Ctrl Pts',(4.16212052091903,4.48077061810374,8.61427768031386));
#7644=CARTESIAN_POINT('Ctrl Pts',(4.03622013617656,4.59450721651413,8.62200244241706));
#7645=CARTESIAN_POINT('Ctrl Pts',(3.90579526204611,4.70282775928251,8.62972720452026));
#7646=CARTESIAN_POINT('Ctrl Pts',(3.77539582973515,4.81112717209608,8.63745045976363));
#7647=CARTESIAN_POINT('Ctrl Pts',(3.640473912771,4.9140124350067,8.645173715007));
#7648=CARTESIAN_POINT('Ctrl Pts',(3.50150160162873,5.01111884675383,8.65289697025037));
#7649=CARTESIAN_POINT('Ctrl Pts',(3.3625239198749,5.10822901119683,8.66062052396042));
#7650=CARTESIAN_POINT('Ctrl Pts',(3.21949578823365,5.19955969282079,8.66834407767047));
#7651=CARTESIAN_POINT('Ctrl Pts',(3.07291955104879,5.28478864244182,8.67606763138052));
#7652=CARTESIAN_POINT('Ctrl Pts',(2.92635315858919,5.37001186769984,8.68379066634166));
#7653=CARTESIAN_POINT('Ctrl Pts',(2.77623941148398,5.44913402175403,8.69151370130279));
#7654=CARTESIAN_POINT('Ctrl Pts',(2.62310675684637,5.52187798712421,8.69923673626392));
#7655=CARTESIAN_POINT('Ctrl Pts',(2.46993340622074,5.59464128467113,8.70696182367127));
#7656=CARTESIAN_POINT('Ctrl Pts',(2.31373983041921,5.66102286836999,8.71468691107863));
#7657=CARTESIAN_POINT('Ctrl Pts',(2.1550769046879,5.72079269834005,8.72241199848598));
#7658=CARTESIAN_POINT('Ctrl Pts',(1.99702922054153,5.78033076096589,8.73010713059661));
#7659=CARTESIAN_POINT('Ctrl Pts',(1.83653160655494,5.83330817515008,8.73780226270723));
#7660=CARTESIAN_POINT('Ctrl Pts',(1.67414592198967,5.87954598539593,8.74549739481786));
#7661=CARTESIAN_POINT('Ctrl Pts',(1.51113497374385,5.92596183364735,8.75322215692104));
#7662=CARTESIAN_POINT('Ctrl Pts',(1.34616364423006,5.96560248367512,8.76094691902423));
#7663=CARTESIAN_POINT('Ctrl Pts',(1.17981044188946,5.99832250581015,8.76867168112741));
#7664=CARTESIAN_POINT('Ctrl Pts',(1.01348968986373,6.03103614529066,8.77639493637074));
#7665=CARTESIAN_POINT('Ctrl Pts',(0.845787913659838,6.05683178948147,8.78411819161407));
#7666=CARTESIAN_POINT('Ctrl Pts',(0.677294151997093,6.07561504657517,8.7918414468574));
#7667=CARTESIAN_POINT('Ctrl Pts',(0.508793878860008,6.0943990295515,8.79956500056744));
#7668=CARTESIAN_POINT('Ctrl Pts',(0.339501873546732,6.10617004410448,8.80728855427748));
#7669=CARTESIAN_POINT('Ctrl Pts',(0.170013431173421,6.11088545103904,8.81501210798751));
#7670=CARTESIAN_POINT('Ctrl Pts',(0.000536372413207947,6.11560054126547,
8.82273514294863));
#7671=CARTESIAN_POINT('Ctrl Pts',(-0.169136780169513,6.11326096338999,8.83045817790974));
#7672=CARTESIAN_POINT('Ctrl Pts',(-0.338409402262352,6.10387619787299,8.83818121287085));
#7673=CARTESIAN_POINT('Ctrl Pts',(-0.507727009643669,6.09448893829417,8.8459063002782));
#7674=CARTESIAN_POINT('Ctrl Pts',(-0.676643557050688,6.07805276513605,8.85363138768555));
#7675=CARTESIAN_POINT('Ctrl Pts',(-0.84456524874239,6.05462922920279,8.86135647509289));
#7676=CARTESIAN_POINT('Ctrl Pts',(-1.01183579646384,6.03129652188154,8.86905160720361));
#7677=CARTESIAN_POINT('Ctrl Pts',(-1.17811888544632,6.00103061981052,8.87674673931433));
#7678=CARTESIAN_POINT('Ctrl Pts',(-1.34283551486153,5.9639431873993,8.88444187142505));
#7679=CARTESIAN_POINT('Ctrl Pts',(-1.5081863832247,5.92671295037753,8.89216663352827));
#7680=CARTESIAN_POINT('Ctrl Pts',(-1.67201726057745,5.88259533119599,8.89989139563148));
#7681=CARTESIAN_POINT('Ctrl Pts',(-1.83375056574864,5.83173939962311,8.9076161577347));
#7682=CARTESIAN_POINT('Ctrl Pts',(-1.99545232180208,5.78089338845452,8.91533941297804));
#7683=CARTESIAN_POINT('Ctrl Pts',(-2.15505701996771,5.72331178267044,8.92306266822139));
#7684=CARTESIAN_POINT('Ctrl Pts',(-2.31200225016791,5.65919350771102,8.93078592346472));
#7685=CARTESIAN_POINT('Ctrl Pts',(-2.46895354554717,5.59507275488834,8.93850947717477));
#7686=CARTESIAN_POINT('Ctrl Pts',(-2.62324487242339,5.52441494359042,8.9462330308848));
#7687=CARTESIAN_POINT('Ctrl Pts',(-2.77433308677689,5.44746743782054,8.95395658459485));
#7688=CARTESIAN_POINT('Ctrl Pts',(-2.92541115335974,5.3705251001946,8.96167961955595));
#7689=CARTESIAN_POINT('Ctrl Pts',(-3.07328625550624,5.28729405732557,8.96940265451705));
#7690=CARTESIAN_POINT('Ctrl Pts',(-3.21743901756219,5.19806807677318,8.97712568947815));
#7691=CARTESIAN_POINT('Ctrl Pts',(-3.3616300891425,5.10881838384215,8.9848507768855));
#7692=CARTESIAN_POINT('Ctrl Pts',(-3.50209657308055,5.01357073470532,8.99257586429285));
#7693=CARTESIAN_POINT('Ctrl Pts',(-3.63834648953989,4.91266326797927,9.0003009517002));
#7694=CARTESIAN_POINT('Ctrl Pts',(-3.77406807454422,4.81214708654792,9.00799608381087));
#7695=CARTESIAN_POINT('Ctrl Pts',(-3.90560550311546,4.70601511495476,9.01569121592155));
#7696=CARTESIAN_POINT('Ctrl Pts',(-4.03250376303064,4.59464241956257,9.02338634803222));
#7697=CARTESIAN_POINT('Ctrl Pts',(-4.15989064282114,4.4828408852519,9.03111111013541));
#7698=CARTESIAN_POINT('Ctrl Pts',(-4.28264765377203,4.36571856902371,9.03883587223861));
#7699=CARTESIAN_POINT('Ctrl Pts',(-4.40033892611598,4.24368270465741,9.04656063434181));
#7700=CARTESIAN_POINT('Ctrl Pts',(-4.51800724056737,4.12167064567792,9.05428388958511));
#7701=CARTESIAN_POINT('Ctrl Pts',(-4.63061156829005,3.99474717905708,9.0620071448284));
#7702=CARTESIAN_POINT('Ctrl Pts',(-4.73775321406145,3.86335605984621,9.06973040007171));
#7703=CARTESIAN_POINT('Ctrl Pts',(-4.84489900034333,3.73195986299908,9.07745395378176));
#7704=CARTESIAN_POINT('Ctrl Pts',(-4.94658147888625,3.59609591117928,9.08517750749182));
#7705=CARTESIAN_POINT('Ctrl Pts',(-5.04244204692123,3.45624127715945,9.09290106120187));
#7706=CARTESIAN_POINT('Ctrl Pts',(-5.13829617652533,3.31639603641169,9.100624096163));
#7707=CARTESIAN_POINT('Ctrl Pts',(-5.22832899893599,3.17256091128272,9.10834713112413));
#7708=CARTESIAN_POINT('Ctrl Pts',(-5.31222498382503,3.02524235123819,9.11607016608525));
#7709=CARTESIAN_POINT('Ctrl Pts',(-5.39614326461181,2.87788464033853,9.12379525349261));
#7710=CARTESIAN_POINT('Ctrl Pts',(-5.47392129009374,2.72704191917447,9.13152034089997));
#7711=CARTESIAN_POINT('Ctrl Pts',(-5.5452888153366,2.5732464936346,9.13924542830732));
#7712=CARTESIAN_POINT('Ctrl Pts',(-5.61637960126538,2.42004743514583,9.14694056041802));
#7713=CARTESIAN_POINT('Ctrl Pts',(-5.68110941194921,2.26391882752246,9.15463569252872));
#7714=CARTESIAN_POINT('Ctrl Pts',(-5.73925813199411,2.10540771748361,9.16233082463941));
#7715=CARTESIAN_POINT('Ctrl Pts',(-5.79753362347359,1.9465510335301,9.17004273309422));
#7716=CARTESIAN_POINT('Ctrl Pts',(-5.84922072930545,1.78524288839063,9.17775464154903));
#7717=CARTESIAN_POINT('Ctrl Pts',(-5.89413163322722,1.62204742615319,9.18546655000383));
#7718=CARTESIAN_POINT('Ctrl Pts',(-5.93903523272857,1.4588785064291,9.19317720417479));
#7719=CARTESIAN_POINT('Ctrl Pts',(-5.97716474304143,1.2938231890582,9.20088785834574));
#7720=CARTESIAN_POINT('Ctrl Pts',(-6.00838243299909,1.12746002205309,9.20859851251669));
#7721=CARTESIAN_POINT('Ctrl Pts',(-6.03959582536704,0.961119757467542,9.21630810519886));
#7722=CARTESIAN_POINT('Ctrl Pts',(-6.06389923863602,0.793472316223263,9.22401769788102));
#7723=CARTESIAN_POINT('Ctrl Pts',(-6.0812061301577,0.625106043029861,9.23172729056319));
#7724=CARTESIAN_POINT('Ctrl Pts',(-6.09851354978445,0.456734632282888,9.23943711849701));
#7725=CARTESIAN_POINT('Ctrl Pts',(-6.10882398799324,0.287644663002158,9.24714694643083));
#7726=CARTESIAN_POINT('Ctrl Pts',(-6.11210274251537,0.118429841830782,9.25485677436465));
#7727=CARTESIAN_POINT('Ctrl Pts',(-6.11286853846333,0.0789075099477037,
9.25665750538959));
#7728=CARTESIAN_POINT('Ctrl Pts',(-6.1132509679055,0.0393783782833313,9.25845823641453));
#7729=CARTESIAN_POINT('Ctrl Pts',(-6.11324999816033,-0.000149975753035227,
9.26025896743946));
#7730=CARTESIAN_POINT('Ctrl Pts',(-6.11324999816031,-0.000149976428034141,
9.26025896747021));
#7731=CARTESIAN_POINT('Ctrl Pts',(-6.11324566360336,-0.176832609976691,
9.26830782018757));
#7732=CARTESIAN_POINT('Ctrl Pts',(-6.10557737691335,-0.35347768337121,9.27635667290493));
#7733=CARTESIAN_POINT('Ctrl Pts',(-6.0902808612631,-0.529437997722481,9.28440552562229));
#7734=CARTESIAN_POINT('Ctrl Pts',(-6.07959408821543,-0.652371088359816,
9.29002878416372));
#7735=CARTESIAN_POINT('Ctrl Pts',(-6.06518507130406,-0.774969979963666,
9.29565204270516));
#7736=CARTESIAN_POINT('Ctrl Pts',(-6.04708101675142,-0.897015462154686,
9.30127530124659));
#7737=CARTESIAN_POINT('Ctrl Pts',(-6.02221118131847,-1.06467133441257,9.30900006334979));
#7738=CARTESIAN_POINT('Ctrl Pts',(-5.99036023379552,-1.23132198049045,9.316724825453));
#7739=CARTESIAN_POINT('Ctrl Pts',(-5.95163401593469,-1.39638035752052,9.3244495875562));
#7740=CARTESIAN_POINT('Ctrl Pts',(-5.91291535234972,-1.56140653681524,9.33217284279952));
#7741=CARTESIAN_POINT('Ctrl Pts',(-5.86732416685052,-1.72484075846385,9.33989609804284));
#7742=CARTESIAN_POINT('Ctrl Pts',(-5.81501714435499,-1.88610741299576,9.34761935328616));
#7743=CARTESIAN_POINT('Ctrl Pts',(-5.76270810044427,-2.04738029970932,9.35534290699621));
#7744=CARTESIAN_POINT('Ctrl Pts',(-5.70368279420213,-2.20648514900584,9.36306646070626));
#7745=CARTESIAN_POINT('Ctrl Pts',(-5.63814764407514,-2.36286197356298,9.3707900144163));
#7746=CARTESIAN_POINT('Ctrl Pts',(-5.57261689558631,-2.51922829514276,9.37851304937742));
#7747=CARTESIAN_POINT('Ctrl Pts',(-5.50057730069756,-2.67286666632751,9.38623608433854));
#7748=CARTESIAN_POINT('Ctrl Pts',(-5.42228331574657,-2.82323736272322,9.39395911929966));
#7749=CARTESIAN_POINT('Ctrl Pts',(-5.34396852366531,-2.97364802109903,9.40168420670701));
#7750=CARTESIAN_POINT('Ctrl Pts',(-5.25939616468751,-3.12078898709069,9.40940929411436));
#7751=CARTESIAN_POINT('Ctrl Pts',(-5.16886697504909,-3.26414456737855,9.41713438152172));
#7752=CARTESIAN_POINT('Ctrl Pts',(-5.07868882722921,-3.40694426283186,9.42482951363241));
#7753=CARTESIAN_POINT('Ctrl Pts',(-4.98260015775692,-3.54598763055786,9.4325246457431));
#7754=CARTESIAN_POINT('Ctrl Pts',(-4.880941269523,-3.68079310556396,9.44021977785379));
#7755=CARTESIAN_POINT('Ctrl Pts',(-4.77889094524181,-3.81611764706001,9.44794453995699));
#7756=CARTESIAN_POINT('Ctrl Pts',(-4.6711912537948,-3.94721950501217,9.4556693020602));
#7757=CARTESIAN_POINT('Ctrl Pts',(-4.55821599606418,-4.07363381954301,9.4633940641634));
#7758=CARTESIAN_POINT('Ctrl Pts',(-4.44526277627839,-4.20002347458872,9.47111731940674));
#7759=CARTESIAN_POINT('Ctrl Pts',(-4.32703625468782,-4.3217271745893,9.47884057465008));
#7760=CARTESIAN_POINT('Ctrl Pts',(-4.20394940881419,-4.43831442448941,9.48656382989342));
#7761=CARTESIAN_POINT('Ctrl Pts',(-4.08085780622533,-4.55490617992661,9.49428738360347));
#7762=CARTESIAN_POINT('Ctrl Pts',(-3.95290573086101,-4.6663808687876,9.50201093731352));
#7763=CARTESIAN_POINT('Ctrl Pts',(-3.82054235846018,-4.77234550820784,9.50973449102357));
#7764=CARTESIAN_POINT('Ctrl Pts',(-3.68818787618433,-4.87830303056184,9.51745752598469));
#7765=CARTESIAN_POINT('Ctrl Pts',(-3.55142293722101,-4.97875104598478,9.52518056094581));
#7766=CARTESIAN_POINT('Ctrl Pts',(-3.41072920625785,-5.07333734775047,9.53290359590693));
#7767=CARTESIAN_POINT('Ctrl Pts',(-3.2699980850303,-5.16794878643452,9.54062868331429));
#7768=CARTESIAN_POINT('Ctrl Pts',(-3.12533634741829,-5.25669521986794,9.54835377072166));
#7769=CARTESIAN_POINT('Ctrl Pts',(-2.97725480052742,-5.33926768529509,9.55607885812901));
#7770=CARTESIAN_POINT('Ctrl Pts',(-2.82974746418462,-5.42151996240964,9.56377399023967));
#7771=CARTESIAN_POINT('Ctrl Pts',(-2.67884708152624,-5.49764594366959,9.57146912235032));
#7772=CARTESIAN_POINT('Ctrl Pts',(-2.52508287618065,-5.5673855651391,9.57916425446097));
#7773=CARTESIAN_POINT('Ctrl Pts',(-2.37072660403329,-5.63739371799112,9.58688901656417));
#7774=CARTESIAN_POINT('Ctrl Pts',(-2.21342973040418,-5.70099099971579,9.59461377866736));
#7775=CARTESIAN_POINT('Ctrl Pts',(-2.05374290216678,-5.75794804199374,9.60233854077056));
#7776=CARTESIAN_POINT('Ctrl Pts',(-1.89408722384319,-5.81489397373129,9.61006179601388));
#7777=CARTESIAN_POINT('Ctrl Pts',(-1.73204281948366,-5.86520214420964,9.61778505125721));
#7778=CARTESIAN_POINT('Ctrl Pts',(-1.56817829685562,-5.90869210500691,9.62550830650053));
#7779=CARTESIAN_POINT('Ctrl Pts',(-1.40430744165072,-5.95218374648231,9.63323186021058));
#7780=CARTESIAN_POINT('Ctrl Pts',(-1.23861663272228,-5.98885656589006,9.64095541392063));
#7781=CARTESIAN_POINT('Ctrl Pts',(-1.07168831750803,-6.01858037352803,9.64867896763067));
#7782=CARTESIAN_POINT('Ctrl Pts',(-0.904771213957228,-6.04830218478014,
9.65640200259179));
#7783=CARTESIAN_POINT('Ctrl Pts',(-0.736617082500552,-6.07107586270196,
9.66412503755291));
#7784=CARTESIAN_POINT('Ctrl Pts',(-0.567817391472592,-6.08682256784615,
9.67184807251403));
#7785=CARTESIAN_POINT('Ctrl Pts',(-0.39897284084057,-6.10257345777856,9.67957315992139));
#7786=CARTESIAN_POINT('Ctrl Pts',(-0.22948270339204,-6.11129361166031,9.68729824732874));
#7787=CARTESIAN_POINT('Ctrl Pts',(-0.0599433489993579,-6.11295610628857,
9.69502333473609));
#7788=CARTESIAN_POINT('Ctrl Pts',(0.108938588669152,-6.11461215432054,9.70271846684678));
#7789=CARTESIAN_POINT('Ctrl Pts',(0.277869049776686,-6.10926520944416,9.71041359895747));
#7790=CARTESIAN_POINT('Ctrl Pts',(0.446258887046951,-6.09694009878985,9.71810873106816));
#7791=CARTESIAN_POINT('Ctrl Pts',(0.615297106898085,-6.08456753047905,9.72583349317136));
#7792=CARTESIAN_POINT('Ctrl Pts',(0.783850397435319,-6.06515853912477,9.73355825527457));
#7793=CARTESIAN_POINT('Ctrl Pts',(0.951325484752262,-6.03877515598659,9.74128301737777));
#7794=CARTESIAN_POINT('Ctrl Pts',(1.1187679029092,-6.01239691942262,9.7490062726211));
#7795=CARTESIAN_POINT('Ctrl Pts',(1.28513222464177,-5.97904705502086,9.75672952786443));
#7796=CARTESIAN_POINT('Ctrl Pts',(1.44983280882339,-5.93883914489686,9.76445278310776));
#7797=CARTESIAN_POINT('Ctrl Pts',(1.6145397578916,-5.89862968093024,9.77217633681781));
#7798=CARTESIAN_POINT('Ctrl Pts',(1.77758253193398,-5.85156171221188,9.77989989052787));
#7799=CARTESIAN_POINT('Ctrl Pts',(1.93838738208954,-5.7977995756542,9.78762344423792));
#7800=CARTESIAN_POINT('Ctrl Pts',(2.09918143186151,-5.74404105000564,9.79534647919905));
#7801=CARTESIAN_POINT('Ctrl Pts',(2.25773755793989,-5.68358935676934,9.80306951416018));
#7802=CARTESIAN_POINT('Ctrl Pts',(2.41349865744236,-5.61665824071787,9.81079254912131));
#7803=CARTESIAN_POINT('Ctrl Pts',(2.56930115145921,-5.54970933729166,9.81851763652867));
#7804=CARTESIAN_POINT('Ctrl Pts',(2.72230684236503,-5.47627769338708,9.82624272393604));
#7805=CARTESIAN_POINT('Ctrl Pts',(2.87197916135893,-5.39662498782527,9.8339678113434));
#7806=CARTESIAN_POINT('Ctrl Pts',(3.02107110132431,-5.3172811487271,9.84166294345405));
#7807=CARTESIAN_POINT('Ctrl Pts',(3.16685521437114,-5.23176458370965,9.8493580755647));
#7808=CARTESIAN_POINT('Ctrl Pts',(3.30882603292164,-5.14037895941146,9.85705320767535));
#7809=CARTESIAN_POINT('Ctrl Pts',(3.45078320703718,-5.04900211794075,9.86474760022748));
#7810=CARTESIAN_POINT('Ctrl Pts',(3.58897790024294,-4.95172510966648,9.8724419927796));
#7811=CARTESIAN_POINT('Ctrl Pts',(3.72292453512037,-4.84888218750454,9.88013638533173));
#7812=CARTESIAN_POINT('',(-6.113249999346,-8.94212127014783E-5,9.1147410326001));
#7813=CARTESIAN_POINT('Ctrl Pts',(-6.113249999346,-8.94212126777935E-5,
9.1147410326001));
#7814=CARTESIAN_POINT('Ctrl Pts',(-6.11324745823273,-0.173811743037197,
9.12265381564133));
#7815=CARTESIAN_POINT('Ctrl Pts',(-6.10583548873119,-0.347505304511466,
9.13056659868255));
#7816=CARTESIAN_POINT('Ctrl Pts',(-6.09104741134544,-0.520544902234175,
9.13847938172378));
#7817=CARTESIAN_POINT('Ctrl Pts',(-6.07625447837759,-0.69364131653641,9.14639476288285));
#7818=CARTESIAN_POINT('Ctrl Pts',(-6.0540806237368,-0.866083056933325,9.15431014404192));
#7819=CARTESIAN_POINT('Ctrl Pts',(-6.02461106481588,-1.03724976750927,9.16222552520099));
#7820=CARTESIAN_POINT('Ctrl Pts',(-6.01454643743982,-1.09570768897857,9.16492883549211));
#7821=CARTESIAN_POINT('Ctrl Pts',(-6.00363128079267,-1.15401695675892,9.16763214578322));
#7822=CARTESIAN_POINT('Ctrl Pts',(-5.99187036227722,-1.2121530943589,9.17033545607434));
#7823=CARTESIAN_POINT('Ctrl Pts',(-5.95826330727307,-1.3782782461899,9.17806021817753));
#7824=CARTESIAN_POINT('Ctrl Pts',(-5.91773729124733,-1.54303431655236,9.18578498028072));
#7825=CARTESIAN_POINT('Ctrl Pts',(-5.87042872341687,-1.70584060386138,9.19350974238391));
#7826=CARTESIAN_POINT('Ctrl Pts',(-5.82312938401064,-1.86861513274787,9.20123299762724));
#7827=CARTESIAN_POINT('Ctrl Pts',(-5.76905022116773,-2.02944033334585,9.20895625287057));
#7828=CARTESIAN_POINT('Ctrl Pts',(-5.70837781947927,-2.18774958177967,9.2166795081139));
#7829=CARTESIAN_POINT('Ctrl Pts',(-5.64770307309394,-2.34606494810545,9.22440306182395));
#7830=CARTESIAN_POINT('Ctrl Pts',(-5.58043468771526,-2.50186387035847,9.23212661553399));
#7831=CARTESIAN_POINT('Ctrl Pts',(-5.50680809604756,-2.65459792733382,9.23985016924404));
#7832=CARTESIAN_POINT('Ctrl Pts',(-5.43318644947603,-2.80732172599649,9.24757320420515));
#7833=CARTESIAN_POINT('Ctrl Pts',(-5.35320758884491,-2.95698078580961,9.25529623916626));
#7834=CARTESIAN_POINT('Ctrl Pts',(-5.26715385886396,-3.10304943395275,9.26301927412738));
#7835=CARTESIAN_POINT('Ctrl Pts',(-5.18107725955049,-3.24915690077911,9.27074436153473));
#7836=CARTESIAN_POINT('Ctrl Pts',(-5.08892272395834,-3.3916717749005,9.27846944894209));
#7837=CARTESIAN_POINT('Ctrl Pts',(-4.99101755607863,-3.53009480289339,9.28619453634944));
#7838=CARTESIAN_POINT('Ctrl Pts',(-4.89349203158589,-3.66798107283438,9.29388966846014));
#7839=CARTESIAN_POINT('Ctrl Pts',(-4.79026060016387,-3.80180693758459,9.30158480057083));
#7840=CARTESIAN_POINT('Ctrl Pts',(-4.68168829277586,-3.93110929532434,9.30927993268153));
#7841=CARTESIAN_POINT('Ctrl Pts',(-4.57269792932238,-4.06090952988217,9.31700469478473));
#7842=CARTESIAN_POINT('Ctrl Pts',(-4.45828685419007,-4.18619730495752,9.32472945688792));
#7843=CARTESIAN_POINT('Ctrl Pts',(-4.33885267649468,-4.30652795348816,9.33245421899112));
#7844=CARTESIAN_POINT('Ctrl Pts',(-4.21944179667792,-4.42683512926671,9.34017747423445));
#7845=CARTESIAN_POINT('Ctrl Pts',(-4.09500999257646,-4.5421868831726,9.34790072947777));
#7846=CARTESIAN_POINT('Ctrl Pts',(-3.96599219842421,-4.65217491551407,9.35562398472109));
#7847=CARTESIAN_POINT('Ctrl Pts',(-3.83696941835378,-4.7621671983648,9.36334753843114));
#7848=CARTESIAN_POINT('Ctrl Pts',(-3.70336053219576,-4.86679513625091,9.3710710921412));
#7849=CARTESIAN_POINT('Ctrl Pts',(-3.56563466029741,-4.96568978408698,9.37879464585125));
#7850=CARTESIAN_POINT('Ctrl Pts',(-3.42791803869402,-5.06457778970942,9.38651768081236));
#7851=CARTESIAN_POINT('Ctrl Pts',(-3.28608524216595,-5.15773309101325,9.39424071577347));
#7852=CARTESIAN_POINT('Ctrl Pts',(-3.14063570222464,-5.24482916293867,9.40196375073458));
#7853=CARTESIAN_POINT('Ctrl Pts',(-2.99514750813191,-5.33194838120579,9.40968883814194));
#7854=CARTESIAN_POINT('Ctrl Pts',(-2.84604092094657,-5.41300498756226,9.4174139255493));
#7855=CARTESIAN_POINT('Ctrl Pts',(-2.69384221228653,-5.48771716634551,9.42513901295666));
#7856=CARTESIAN_POINT('Ctrl Pts',(-2.5422336791458,-5.56213963637039,9.43283414506734));
#7857=CARTESIAN_POINT('Ctrl Pts',(-2.38755725677093,-5.6302666858497,9.44052927717802));
#7858=CARTESIAN_POINT('Ctrl Pts',(-2.23035504983439,-5.69186629447479,9.4482244092887));
#7859=CARTESIAN_POINT('Ctrl Pts',(-2.07254753812235,-5.75370309148291,9.4559491713919));
#7860=CARTESIAN_POINT('Ctrl Pts',(-1.91213885056458,-5.80898395301959,9.4636739334951));
#7861=CARTESIAN_POINT('Ctrl Pts',(-1.7496908798326,-5.85750863315886,9.47139869559829));
#7862=CARTESIAN_POINT('Ctrl Pts',(-1.58727459762713,-5.90602384764827,9.47912195084161));
#7863=CARTESIAN_POINT('Ctrl Pts',(-1.42282012948558,-5.94778541980937,9.48684520608493));
#7864=CARTESIAN_POINT('Ctrl Pts',(-1.25690474502644,-5.98264289628171,9.49456846132825));
#7865=CARTESIAN_POINT('Ctrl Pts',(-1.09098294873446,-6.01750171982813,9.5022920150383));
#7866=CARTESIAN_POINT('Ctrl Pts',(-0.923600432482852,-6.04545584474639,
9.51001556874834));
#7867=CARTESIAN_POINT('Ctrl Pts',(-0.755345657214048,-6.06640573161966,
9.51773912245839));
#7868=CARTESIAN_POINT('Ctrl Pts',(-0.587102182699702,-6.08735421140344,
9.52546215741951));
#7869=CARTESIAN_POINT('Ctrl Pts',(-0.417986880935509,-6.10129935540618,
9.53318519238063));
#7870=CARTESIAN_POINT('Ctrl Pts',(-0.248594534907554,-6.10819337609036,
9.54090822734175));
#7871=CARTESIAN_POINT('Ctrl Pts',(-0.0791571717736587,-6.11508922890489,
9.54863331474911));
#7872=CARTESIAN_POINT('Ctrl Pts',(0.0905570659481728,-6.11493019885617,
9.55635840215646));
#7873=CARTESIAN_POINT('Ctrl Pts',(0.259951216556874,-6.10772059998741,9.56408348956382));
#7874=CARTESIAN_POINT('Ctrl Pts',(0.428688513492966,-6.10053895752375,9.57177862167451));
#7875=CARTESIAN_POINT('Ctrl Pts',(0.597107890748209,-6.08636137400293,9.5794737537852));
#7876=CARTESIAN_POINT('Ctrl Pts',(0.764622306756637,-6.06524346506471,9.58716888589589));
#7877=CARTESIAN_POINT('Ctrl Pts',(0.932781734549123,-6.04404424193011,9.59489364799909));
#7878=CARTESIAN_POINT('Ctrl Pts',(1.10008877149121,-6.01584360211571,9.60261841010229));
#7879=CARTESIAN_POINT('Ctrl Pts',(1.26595420145235,-5.98073453033364,9.61034317220549));
#7880=CARTESIAN_POINT('Ctrl Pts',(1.43178727624756,-5.94563230723513,9.61806642744883));
#7881=CARTESIAN_POINT('Ctrl Pts',(1.5961789953133,-5.9036244067426,9.62578968269216));
#7882=CARTESIAN_POINT('Ctrl Pts',(1.75855046184005,-5.85485489450099,9.6335129379355));
#7883=CARTESIAN_POINT('Ctrl Pts',(1.92092820324404,-5.80608349755198,9.64123649164555));
#7884=CARTESIAN_POINT('Ctrl Pts',(2.08128523121816,-5.75055005334046,9.64896004535559));
#7885=CARTESIAN_POINT('Ctrl Pts',(2.23905718027886,-5.68844869063101,9.65668359906564));
#7886=CARTESIAN_POINT('Ctrl Pts',(2.39681853265922,-5.62635149893101,9.66440663402676));
#7887=CARTESIAN_POINT('Ctrl Pts',(2.55199485864944,-5.55768738760475,9.67212966898789));
#7888=CARTESIAN_POINT('Ctrl Pts',(2.70404100082699,-5.4826989547436,9.67985270394901));
#7889=CARTESIAN_POINT('Ctrl Pts',(2.85612755024525,-5.40769059322387,9.68757779135637));
#7890=CARTESIAN_POINT('Ctrl Pts',(3.00508196817793,-5.32635468999279,9.69530287876373));
#7891=CARTESIAN_POINT('Ctrl Pts',(3.150382110936,-5.23898063726088,9.70302796617109));
#7892=CARTESIAN_POINT('Ctrl Pts',(3.29511882849818,-5.15194539178574,9.71072309828175));
#7893=CARTESIAN_POINT('Ctrl Pts',(3.43622930968405,-5.05891892991148,9.71841823039243));
#7894=CARTESIAN_POINT('Ctrl Pts',(3.57322466611832,-4.96023094703701,9.72611336250309));
#7895=CARTESIAN_POINT('Ctrl Pts',(3.62368399696851,-4.92388132389347,9.72894770103262));
#7896=CARTESIAN_POINT('Ctrl Pts',(3.67359190198392,-4.88675930292695,9.73178203956215));
#7897=CARTESIAN_POINT('Ctrl Pts',(3.72292453512039,-4.84888218750452,9.73461637809168));
#7898=CARTESIAN_POINT('Ctrl Pts',(3.72292453512037,-4.84888218750454,7.98461472294509));
#7899=CARTESIAN_POINT('Ctrl Pts',(3.8574022678144,-4.74563149360974,7.99233781167824));
#7900=CARTESIAN_POINT('Ctrl Pts',(3.98758355070785,-4.63678185091767,8.00006090041139));
#7901=CARTESIAN_POINT('Ctrl Pts',(4.11301107379905,-4.52271660280703,8.00778398914454));
#7902=CARTESIAN_POINT('Ctrl Pts',(4.23843847491679,-4.40865146562047,8.01550707036727));
#7903=CARTESIAN_POINT('Ctrl Pts',(4.35911189315032,-4.28937094866781,8.02323015159001));
#7904=CARTESIAN_POINT('Ctrl Pts',(4.47460933368528,-4.16529673293471,8.03095323281275));
#7905=CARTESIAN_POINT('Ctrl Pts',(4.59013082874591,-4.04119667640035,8.03867792251317));
#7906=CARTESIAN_POINT('Ctrl Pts',(4.70047397780303,-3.91230115962854,8.04640261221359));
#7907=CARTESIAN_POINT('Ctrl Pts',(4.80525518851297,-3.77906709860637,8.05412730191402));
#7908=CARTESIAN_POINT('Ctrl Pts',(4.82629068090824,-3.75231951611106,8.0556780823483));
#7909=CARTESIAN_POINT('Ctrl Pts',(4.84710214032259,-3.7253971827812,8.05722886278257));
#7910=CARTESIAN_POINT('Ctrl Pts',(4.86768666217403,-3.69830395200192,8.05877964321685));
#7911=CARTESIAN_POINT('Ctrl Pts',(4.97022247626845,-3.56334689570254,8.06650440532005));
#7912=CARTESIAN_POINT('Ctrl Pts',(5.0671604439934,-3.42409909101741,8.07422916742325));
#7913=CARTESIAN_POINT('Ctrl Pts',(5.15815464990081,-3.28104650534044,8.08195392952645));
#7914=CARTESIAN_POINT('Ctrl Pts',(5.24913110568005,-3.13802182475594,8.08967718476978));
#7915=CARTESIAN_POINT('Ctrl Pts',(5.33416594314995,-2.99119411137184,8.09740044001311));
#7916=CARTESIAN_POINT('Ctrl Pts',(5.41295695714888,-2.84107770793999,8.10512369525643));
#7917=CARTESIAN_POINT('Ctrl Pts',(5.49175101604207,-2.69095550323017,8.11284724896648));
#7918=CARTESIAN_POINT('Ctrl Pts',(5.56430061782847,-2.53754463292657,8.12057080267653));
#7919=CARTESIAN_POINT('Ctrl Pts',(5.63034948816571,-2.38138409409573,8.12829435638658));
#7920=CARTESIAN_POINT('Ctrl Pts',(5.69639392236101,-2.22523404371551,8.1360173913477));
#7921=CARTESIAN_POINT('Ctrl Pts',(5.7559383753895,-2.06633498630608,8.14374042630882));
#7922=CARTESIAN_POINT('Ctrl Pts',(5.80877463804117,-1.90524611715905,8.15146346126995));
#7923=CARTESIAN_POINT('Ctrl Pts',(5.86162494226961,-1.74411443760854,8.1591885486773));
#7924=CARTESIAN_POINT('Ctrl Pts',(5.90776339285081,-1.58079208410473,8.16691363608466));
#7925=CARTESIAN_POINT('Ctrl Pts',(5.94703131228762,-1.41585455932823,8.17463872349201));
#7926=CARTESIAN_POINT('Ctrl Pts',(5.98614696390985,-1.25155660692535,8.18233385560268));
#7927=CARTESIAN_POINT('Ctrl Pts',(6.01844523195451,-1.08565629833407,8.19002898771335));
#7928=CARTESIAN_POINT('Ctrl Pts',(6.04381950108335,-0.918733585336168,8.19772411982402));
#7929=CARTESIAN_POINT('Ctrl Pts',(6.06929147346066,-0.751168138897491,8.20544888192722));
#7930=CARTESIAN_POINT('Ctrl Pts',(6.08779501129324,-0.582513047708593,8.21317364403042));
#7931=CARTESIAN_POINT('Ctrl Pts',(6.09925885820982,-0.413360548491332,8.22089840613361));
#7932=CARTESIAN_POINT('Ctrl Pts',(6.11072046888784,-0.244241045644635,8.22862166137694));
#7933=CARTESIAN_POINT('Ctrl Pts',(6.11514510730666,-0.0746246443857959,
8.23634491662026));
#7934=CARTESIAN_POINT('Ctrl Pts',(6.11251347583972,0.0948924137001474,8.24406817186359));
#7935=CARTESIAN_POINT('Ctrl Pts',(6.10988174267286,0.264416022806168,8.25179172557364));
#7936=CARTESIAN_POINT('Ctrl Pts',(6.10019319490759,0.433839964115716,8.25951527928369));
#7937=CARTESIAN_POINT('Ctrl Pts',(6.08348066331392,0.602568321093682,8.26723883299373));
#7938=CARTESIAN_POINT('Ctrl Pts',(6.06676925420973,0.771285345509321,8.27496186795485));
#7939=CARTESIAN_POINT('Ctrl Pts',(6.04303483659968,0.939306563671693,8.28268490291598));
#7940=CARTESIAN_POINT('Ctrl Pts',(6.01236211192288,1.10604131822201,8.2904079378771));
#7941=CARTESIAN_POINT('Ctrl Pts',(5.98168123577213,1.27282038360621,8.29813302528446));
#7942=CARTESIAN_POINT('Ctrl Pts',(5.94405842323202,1.43831198989677,8.30585811269181));
#7943=CARTESIAN_POINT('Ctrl Pts',(5.89962967276359,1.60193485721093,8.31358320009917));
#7944=CARTESIAN_POINT('Ctrl Pts',(5.85537320208061,1.76492324995224,8.32127833220985));
#7945=CARTESIAN_POINT('Ctrl Pts',(5.80436359484624,1.92605707780743,8.32897346432053));
#7946=CARTESIAN_POINT('Ctrl Pts',(5.74678469524245,2.08477606208128,8.33666859643122));
#7947=CARTESIAN_POINT('Ctrl Pts',(5.68898408893631,2.24410619145943,8.34439335853442));
#7948=CARTESIAN_POINT('Ctrl Pts',(5.62454300042812,2.40105926345284,8.35211812063762));
#7949=CARTESIAN_POINT('Ctrl Pts',(5.55368220100643,2.55508112840364,8.35984288274082));
#7950=CARTESIAN_POINT('Ctrl Pts',(5.48283522431398,2.70907294849812,8.36756613798415));
#7951=CARTESIAN_POINT('Ctrl Pts',(5.40557116784684,2.86013441472761,8.37528939322748));
#7952=CARTESIAN_POINT('Ctrl Pts',(5.32215834526735,3.00773271924238,8.38301264847081));
#7953=CARTESIAN_POINT('Ctrl Pts',(5.2387422991829,3.15533672772269,8.39073620218086));
#7954=CARTESIAN_POINT('Ctrl Pts',(5.1491771639691,3.29947702882138,8.39845975589091));
#7955=CARTESIAN_POINT('Ctrl Pts',(5.05377687308074,3.43964603987303,8.40618330960096));
#7956=CARTESIAN_POINT('Ctrl Pts',(4.95838298970897,3.57980563653764,8.41390634456209));
#7957=CARTESIAN_POINT('Ctrl Pts',(4.85715491329265,3.7159942149028,8.42162937952321));
#7958=CARTESIAN_POINT('Ctrl Pts',(4.75044961013144,3.84773362696822,8.42935241448434));
#7959=CARTESIAN_POINT('Ctrl Pts',(4.64371594934927,3.97950804963014,8.4370775018917));
#7960=CARTESIAN_POINT('Ctrl Pts',(4.53150235108678,4.10683069545986,8.44480258929906));
#7961=CARTESIAN_POINT('Ctrl Pts',(4.41420634043892,4.22925619305911,8.45252767670642));
#7962=CARTESIAN_POINT('Ctrl Pts',(4.29736516435994,4.35120696566036,8.46022280881708));
#7963=CARTESIAN_POINT('Ctrl Pts',(4.17548116086376,4.46829829839282,8.46791794092775));
#7964=CARTESIAN_POINT('Ctrl Pts',(4.04898382203956,4.58012615234143,8.47561307303841));
#7965=CARTESIAN_POINT('Ctrl Pts',(3.92199940708056,4.69238459778999,8.48333783514161));
#7966=CARTESIAN_POINT('Ctrl Pts',(3.79032106512151,4.79937868620239,8.49106259724481));
#7967=CARTESIAN_POINT('Ctrl Pts',(3.65440778259716,4.900727427739,8.49878735934801));
#7968=CARTESIAN_POINT('Ctrl Pts',(3.51852101251008,5.00205639930094,8.50651061459134));
#7969=CARTESIAN_POINT('Ctrl Pts',(3.37840120414425,5.09774203199839,8.51423386983468));
#7970=CARTESIAN_POINT('Ctrl Pts',(3.23453888158875,5.18744482245263,8.52195712507801));
#7971=CARTESIAN_POINT('Ctrl Pts',(3.09067099944551,5.27715107948885,8.52968067878806));
#7972=CARTESIAN_POINT('Ctrl Pts',(2.94306058052596,5.36087386057674,8.53740423249811));
#7973=CARTESIAN_POINT('Ctrl Pts',(2.79222614038394,5.43831763907337,8.54512778620816));
#7974=CARTESIAN_POINT('Ctrl Pts',(2.64140183096753,5.51575621609434,8.55285082116929));
#7975=CARTESIAN_POINT('Ctrl Pts',(2.48735421562718,5.58691648970304,8.56057385613042));
#7976=CARTESIAN_POINT('Ctrl Pts',(2.33062551577657,5.65154936877589,8.56829689109155));
#7977=CARTESIAN_POINT('Ctrl Pts',(2.17385516426556,5.71619942445221,8.57602197849891));
#7978=CARTESIAN_POINT('Ctrl Pts',(2.01440259683183,5.77431849632089,8.58374706590627));
#7979=CARTESIAN_POINT('Ctrl Pts',(1.85282996934096,5.82570567976206,8.59147215331363));
#7980=CARTESIAN_POINT('Ctrl Pts',(1.69188386628157,5.87689360094954,8.59916728542429));
#7981=CARTESIAN_POINT('Ctrl Pts',(1.52883442297593,5.92140168501278,8.60686241753494));
#7982=CARTESIAN_POINT('Ctrl Pts',(1.36425209167301,5.95908061640937,8.61455754964559));
#7983=CARTESIAN_POINT('Ctrl Pts',(1.19903603853412,5.99690462997482,8.62228231174879));
#7984=CARTESIAN_POINT('Ctrl Pts',(1.03221674792847,6.02786016224444,8.63000707385199));
#7985=CARTESIAN_POINT('Ctrl Pts',(0.864379544508043,6.05183224862818,8.63773183595519));
#7986=CARTESIAN_POINT('Ctrl Pts',(0.696575080885137,6.07579965880643,8.64545509119851));
#7987=CARTESIAN_POINT('Ctrl Pts',(0.527753414203596,6.09278629649545,8.65317834644184));
#7988=CARTESIAN_POINT('Ctrl Pts',(0.358507714816743,6.10272871598573,8.66090160168516));
#7989=CARTESIAN_POINT('Ctrl Pts',(0.189255474896465,6.11267151970278,8.6686251553952));
#7990=CARTESIAN_POINT('Ctrl Pts',(0.0195794856200138,6.11556953794196,8.67634870910525));
#7991=CARTESIAN_POINT('Ctrl Pts',(-0.149923542379877,6.11141133404881,8.6840722628153));
#7992=CARTESIAN_POINT('Ctrl Pts',(-0.319415185787106,6.10725340943951,8.69179529777642));
#7993=CARTESIAN_POINT('Ctrl Pts',(-0.488733574303142,6.09604021888496,8.69951833273755));
#7994=CARTESIAN_POINT('Ctrl Pts',(-0.657283396671435,6.07781244354908,8.70724136769867));
#7995=CARTESIAN_POINT('Ctrl Pts',(-0.825878012239498,6.05957982406463,8.71496645510603));
#7996=CARTESIAN_POINT('Ctrl Pts',(-0.993703337970038,6.03432892666479,8.72269154251339));
#7997=CARTESIAN_POINT('Ctrl Pts',(-1.16016961147651,6.00215228356516,8.73041662992074));
#7998=CARTESIAN_POINT('Ctrl Pts',(-1.32599038463506,5.97010041069001,8.73811176203142));
#7999=CARTESIAN_POINT('Ctrl Pts',(-1.49046232633288,5.93117649896973,8.74580689414211));
#8000=CARTESIAN_POINT('Ctrl Pts',(-1.65301307063605,5.88552235156799,8.75350202625279));
#8001=CARTESIAN_POINT('Ctrl Pts',(-1.81618971417897,5.83969241354607,8.76122678835599));
#8002=CARTESIAN_POINT('Ctrl Pts',(-1.97748812006645,5.78706404710313,8.76895155045919));
#8003=CARTESIAN_POINT('Ctrl Pts',(-2.1363392970195,5.7278163352634,8.7766763125624));
#8004=CARTESIAN_POINT('Ctrl Pts',(-2.29515948706802,5.66858018080225,8.78439956780572));
#8005=CARTESIAN_POINT('Ctrl Pts',(-2.45153310395785,5.60272736809181,8.79212282304904));
#8006=CARTESIAN_POINT('Ctrl Pts',(-2.60490891503397,5.53048597384322,8.79984607829236));
#8007=CARTESIAN_POINT('Ctrl Pts',(-2.75829065334869,5.45824178781163,8.80756963200241));
#8008=CARTESIAN_POINT('Ctrl Pts',(-2.90867406563048,5.37960865766176,8.81529318571245));
#8009=CARTESIAN_POINT('Ctrl Pts',(-3.05552969306556,5.29486202438691,8.8230167394225));
#8010=CARTESIAN_POINT('Ctrl Pts',(-3.20237545701001,5.21012108308068,8.83073977438362));
#8011=CARTESIAN_POINT('Ctrl Pts',(-3.34569363574495,5.11926761877613,8.83846280934474));
#8012=CARTESIAN_POINT('Ctrl Pts',(-3.48498093397388,5.02262216898091,8.84618584430586));
#8013=CARTESIAN_POINT('Ctrl Pts',(-3.62430524869861,4.92595103503552,8.85391093171321));
#8014=CARTESIAN_POINT('Ctrl Pts',(-3.7595962805231,4.82348501879639,8.86163601912057));
#8015=CARTESIAN_POINT('Ctrl Pts',(-3.89038041381802,4.71558753479151,8.86936110652793));
#8016=CARTESIAN_POINT('Ctrl Pts',(-4.02065741013091,4.60810844102275,8.8770562386386));
#8017=CARTESIAN_POINT('Ctrl Pts',(-4.14646217796333,4.49524015096725,8.88475137074928));
#8018=CARTESIAN_POINT('Ctrl Pts',(-4.26735995062769,4.37738102228705,8.89244650285996));
#8019=CARTESIAN_POINT('Ctrl Pts',(-4.38872323837968,4.25906807877299,8.90017126496315));
#8020=CARTESIAN_POINT('Ctrl Pts',(-4.50518462963113,4.13568386161381,8.90789602706634));
#8021=CARTESIAN_POINT('Ctrl Pts',(-4.61633015684259,4.00765785035669,8.91562078916953));
#8022=CARTESIAN_POINT('Ctrl Pts',(-4.72745400303229,3.87965681297668,8.92334404441284));
#8023=CARTESIAN_POINT('Ctrl Pts',(-4.83326384664574,3.7470160274108,8.93106729965615));
#8024=CARTESIAN_POINT('Ctrl Pts',(-4.93338475446752,3.61019949959659,8.93879055489947));
#8025=CARTESIAN_POINT('Ctrl Pts',(-5.03350953148165,3.4733776844805,8.94651410860951));
#8026=CARTESIAN_POINT('Ctrl Pts',(-5.1279447424171,3.33238005761311,8.95423766231956));
#8027=CARTESIAN_POINT('Ctrl Pts',(-5.21635723469462,3.18770179950212,8.96196121602961));
#8028=CARTESIAN_POINT('Ctrl Pts',(-5.3047637887878,3.04303325863974,8.96968425099072));
#8029=CARTESIAN_POINT('Ctrl Pts',(-5.38714826845094,2.89468485169631,8.97740728595184));
#8030=CARTESIAN_POINT('Ctrl Pts',(-5.46322207146371,2.74317884221421,8.98513032091295));
#8031=CARTESIAN_POINT('Ctrl Pts',(-5.53931609157915,2.59163256903522,8.9928554083203));
#8032=CARTESIAN_POINT('Ctrl Pts',(-5.60909593952382,2.43692729893481,9.00058049572766));
#8033=CARTESIAN_POINT('Ctrl Pts',(-5.67231958918843,2.27960874726546,9.00830558313501));
#8034=CARTESIAN_POINT('Ctrl Pts',(-5.73529807875576,2.12290022414772,9.01600071524572));
#8035=CARTESIAN_POINT('Ctrl Pts',(-5.79177103862998,1.96359895198479,9.02369584735643));
#8036=CARTESIAN_POINT('Ctrl Pts',(-5.84154727478895,1.80226274413744,9.03139097946714));
#8037=CARTESIAN_POINT('Ctrl Pts',(-5.89171153494281,1.63966886144922,9.03914609795154));
#8038=CARTESIAN_POINT('Ctrl Pts',(-5.93509151719397,1.47495225274229,9.04690121643594));
#8039=CARTESIAN_POINT('Ctrl Pts',(-5.97152821508267,1.30869260675361,9.05465633492034));
#8040=CARTESIAN_POINT('Ctrl Pts',(-6.00795675422069,1.14247018891895,9.06240971691153));
#8041=CARTESIAN_POINT('Ctrl Pts',(-6.03744504534487,0.974705727749124,9.07016309890272));
#8042=CARTESIAN_POINT('Ctrl Pts',(-6.05988488740563,0.805990517247494,9.07791648089391));
#8043=CARTESIAN_POINT('Ctrl Pts',(-6.08232272788607,0.637290355739623,9.08566917130195));
#8044=CARTESIAN_POINT('Ctrl Pts',(-6.09771333128856,0.467639922840535,9.09342186171));
#8045=CARTESIAN_POINT('Ctrl Pts',(-6.10600010853084,0.297637761585123,9.10117455211803));
#8046=CARTESIAN_POINT('Ctrl Pts',(-6.11083380261946,0.198475153747465,9.10569671226554));
#8047=CARTESIAN_POINT('Ctrl Pts',(-6.11325145157963,0.0991929884357902,
9.11021887241305));
#8048=CARTESIAN_POINT('Ctrl Pts',(-6.11324999934601,-8.94203443601632E-5,
9.11474103256055));
#8049=CARTESIAN_POINT('Origin',(0.,0.,-3.86474103256053));
#8050=CARTESIAN_POINT('',(3.72292453512036,-4.84888218750454,6.23460979329304));
#8051=CARTESIAN_POINT('',(3.72323907905152,-4.84929205898336,6.38013065756227));
#8052=CARTESIAN_POINT('',(3.72292453512038,-4.84888218750453,-3.86474103256053));
#8053=CARTESIAN_POINT('',(-6.11324999906832,0.000106729296146127,7.51025896743946));
#8054=CARTESIAN_POINT('Ctrl Pts',(3.72323907905155,-4.84929205898333,6.38013065756227));
#8055=CARTESIAN_POINT('Ctrl Pts',(3.74244957685544,-4.83454974172044,6.38123420254007));
#8056=CARTESIAN_POINT('Ctrl Pts',(4.56407058896953,-4.19609180936438,6.4286525730536));
#8057=CARTESIAN_POINT('Ctrl Pts',(5.85647901784331,-2.51246545019524,6.52238576910286));
#8058=CARTESIAN_POINT('Ctrl Pts',(6.34476406083597,0.595649340793697,6.66133024571005));
#8059=CARTESIAN_POINT('Ctrl Pts',(5.28652688781551,3.55857592152639,6.80027472231724));
#8060=CARTESIAN_POINT('Ctrl Pts',(2.93971047068678,5.65410748689819,6.93921919892443));
#8061=CARTESIAN_POINT('Ctrl Pts',(-0.123653876037357,6.37146284959777,7.07816367553161));
#8062=CARTESIAN_POINT('Ctrl Pts',(-3.15687786378923,5.53578822553583,7.2171081521388));
#8063=CARTESIAN_POINT('Ctrl Pts',(-5.42061984988151,3.35077745723799,7.35605262874599));
#8064=CARTESIAN_POINT('Ctrl Pts',(-6.0834461464926,1.23970149668133,7.45376956717954));
#8065=CARTESIAN_POINT('Ctrl Pts',(-6.11370812977969,0.111745833966236,7.50517168007736));
#8066=CARTESIAN_POINT('Ctrl Pts',(-6.11361710986571,0.000106735705416132,
7.51025896743946));
#8067=CARTESIAN_POINT('Ctrl Pts',(-6.11324999906832,0.000106729296146127,
7.51025896743946));
#8068=CARTESIAN_POINT('Ctrl Pts',(-6.11325294774147,-0.168787630489055,
7.51795578481954));
#8069=CARTESIAN_POINT('Ctrl Pts',(-6.10625233739568,-0.33771293236707,7.52565260219963));
#8070=CARTESIAN_POINT('Ctrl Pts',(-6.09226654106778,-0.506077024854876,
7.53334941957971));
#8071=CARTESIAN_POINT('Ctrl Pts',(-6.07828327346374,-0.674410676008743,
7.54104484532465));
#8072=CARTESIAN_POINT('Ctrl Pts',(-6.05731736650498,-0.842183000067764,
7.54874027106959));
#8073=CARTESIAN_POINT('Ctrl Pts',(-6.02943916153457,-1.00880570966528,7.55643569681453));
#8074=CARTESIAN_POINT('Ctrl Pts',(-6.0015598834746,-1.1754348329143,7.56413141877227));
#8075=CARTESIAN_POINT('Ctrl Pts',(-5.96676782543536,-1.34091393569506,7.57182714073001));
#8076=CARTESIAN_POINT('Ctrl Pts',(-5.92518479316057,-1.50466299529121,7.57952286268775));
#8077=CARTESIAN_POINT('Ctrl Pts',(-5.88360268844497,-1.66840840226907,7.58721841298322));
#8078=CARTESIAN_POINT('Ctrl Pts',(-5.83522999381734,-1.8304235322667,7.5949139632787));
#8079=CARTESIAN_POINT('Ctrl Pts',(-5.78023897185452,-1.9901414499362,7.60260951357417));
#8080=CARTESIAN_POINT('Ctrl Pts',(-5.72523548542042,-2.14989556986797,7.61030680817193));
#8081=CARTESIAN_POINT('Ctrl Pts',(-5.66361078029505,-2.30735113356998,7.6180041027697));
#8082=CARTESIAN_POINT('Ctrl Pts',(-5.59558629701935,-2.46195847956648,7.62570139736746));
#8083=CARTESIAN_POINT('Ctrl Pts',(-5.57131221422705,-2.51712907897855,7.6284481255651));
#8084=CARTESIAN_POINT('Ctrl Pts',(-5.5462236479206,-2.57193717972177,7.63119485376273));
#8085=CARTESIAN_POINT('Ctrl Pts',(-5.52033212740917,-2.62635846098626,7.63394158196037));
#8086=CARTESIAN_POINT('Ctrl Pts',(-5.4475160997392,-2.77941017228462,7.64166634406357));
#8087=CARTESIAN_POINT('Ctrl Pts',(-5.36831819637481,-2.92945887370836,7.64939110616676));
#8088=CARTESIAN_POINT('Ctrl Pts',(-5.28301132117769,-3.07597414534133,7.65711586826996));
#8089=CARTESIAN_POINT('Ctrl Pts',(-5.197721086688,-3.22246083642012,7.6648391235133));
#8090=CARTESIAN_POINT('Ctrl Pts',(-5.10632441754276,-3.36541519931389,7.67256237875664));
#8091=CARTESIAN_POINT('Ctrl Pts',(-5.00913949382559,-3.50433261747465,7.68028563399997));
#8092=CARTESIAN_POINT('Ctrl Pts',(-4.91195081437798,-3.64325540412627,7.68800918771002));
#8093=CARTESIAN_POINT('Ctrl Pts',(-4.80897361116746,-3.77814067191202,7.69573274142008));
#8094=CARTESIAN_POINT('Ctrl Pts',(-4.70056905431399,-3.90851328872317,7.70345629513013));
#8095=CARTESIAN_POINT('Ctrl Pts',(-4.59217177840257,-4.03887714911768,7.71117933009126));
#8096=CARTESIAN_POINT('Ctrl Pts',(-4.47834808097592,-4.1647287213615,7.71890236505238));
#8097=CARTESIAN_POINT('Ctrl Pts',(-4.35949914342364,-4.28562629973596,7.72662540001351));
#8098=CARTESIAN_POINT('Ctrl Pts',(-4.24061862100162,-4.40655600741964,7.73435048742087));
#8099=CARTESIAN_POINT('Ctrl Pts',(-4.11671041060107,-4.52252886274096,7.74207557482822));
#8100=CARTESIAN_POINT('Ctrl Pts',(-3.98821292170116,-4.63313967560615,7.74980066223558));
#8101=CARTESIAN_POINT('Ctrl Pts',(-3.86021370294402,-4.74332157685611,7.75749579434623));
#8102=CARTESIAN_POINT('Ctrl Pts',(-3.72766099141761,-4.84818276689439,7.76519092645689));
#8103=CARTESIAN_POINT('Ctrl Pts',(-3.59102105187657,-4.9473622636188,7.77288605856754));
#8104=CARTESIAN_POINT('Ctrl Pts',(-3.4538549822663,-5.0469236495306,7.78061082067074));
#8105=CARTESIAN_POINT('Ctrl Pts',(-3.31252154875908,-5.14079473810075,7.78833558277394));
#8106=CARTESIAN_POINT('Ctrl Pts',(-3.16751416376062,-5.22864031894295,7.79606034487714));
#8107=CARTESIAN_POINT('Ctrl Pts',(-3.02253506517465,-5.31646876385559,7.80378360012048));
#8108=CARTESIAN_POINT('Ctrl Pts',(-2.87388371601856,-5.39827388224882,7.81150685536382));
#8109=CARTESIAN_POINT('Ctrl Pts',(-2.72208094184447,-5.47376478381627,7.81923011060717));
#8110=CARTESIAN_POINT('Ctrl Pts',(-2.5702723012226,-5.5492586027443,7.82695366431721));
#8111=CARTESIAN_POINT('Ctrl Pts',(-2.41531227388109,-5.61843757189667,7.83467721802726));
#8112=CARTESIAN_POINT('Ctrl Pts',(-2.2577453298272,-5.6810572597135,7.84240077173731));
#8113=CARTESIAN_POINT('Ctrl Pts',(-2.10018896868471,-5.74367274170778,7.85012380669842));
#8114=CARTESIAN_POINT('Ctrl Pts',(-1.94002633576995,-5.79972970692885,7.85784684165953));
#8115=CARTESIAN_POINT('Ctrl Pts',(-1.77782104386801,-5.8490322189641,7.86556987662064));
#8116=CARTESIAN_POINT('Ctrl Pts',(-1.61557264486594,-5.89834783345918,7.87329496402799));
#8117=CARTESIAN_POINT('Ctrl Pts',(-1.45128080493979,-5.94090531352668,7.88102005143534));
#8118=CARTESIAN_POINT('Ctrl Pts',(-1.28552435768903,-5.97655859908428,7.88874513884269));
#8119=CARTESIAN_POINT('Ctrl Pts',(-1.12041065831811,-6.01207363316459,7.89644027095337));
#8120=CARTESIAN_POINT('Ctrl Pts',(-0.953844001930205,-6.04073788771953,
7.90413540306405));
#8121=CARTESIAN_POINT('Ctrl Pts',(-0.786406532173293,-6.06245744963667,
7.91183053517473));
#8122=CARTESIAN_POINT('Ctrl Pts',(-0.618324346912324,-6.08426064240615,
7.91955529727793));
#8123=CARTESIAN_POINT('Ctrl Pts',(-0.449305095290647,-6.0990732477667,7.92728005938114));
#8124=CARTESIAN_POINT('Ctrl Pts',(-0.279942430074679,-6.10683697165266,
7.93500482148434));
#8125=CARTESIAN_POINT('Ctrl Pts',(-0.110612802225837,-6.11459918107854,
7.94272807672769));
#8126=CARTESIAN_POINT('Ctrl Pts',(0.0590597891480183,-6.11531523817638,
7.95045133197104));
#8127=CARTESIAN_POINT('Ctrl Pts',(0.228478823103353,-6.10897888275064,7.95817458721439));
#8128=CARTESIAN_POINT('Ctrl Pts',(0.397904404290227,-6.10264228245522,7.96589814092444));
#8129=CARTESIAN_POINT('Ctrl Pts',(0.567076091606076,-6.08925273214945,7.97362169463449));
#8130=CARTESIAN_POINT('Ctrl Pts',(0.735398828517154,-6.06885608047477,7.98134524834454));
#8131=CARTESIAN_POINT('Ctrl Pts',(0.903710260109033,-6.04846079873182,7.98906828330565));
#8132=CARTESIAN_POINT('Ctrl Pts',(1.07117254074636,-6.0210593955603,7.99679131826677));
#8133=CARTESIAN_POINT('Ctrl Pts',(1.23719700561922,-5.98674946292116,8.00451435322789));
#8134=CARTESIAN_POINT('Ctrl Pts',(1.40326559256198,-5.95243041219664,8.01223944063524));
#8135=CARTESIAN_POINT('Ctrl Pts',(1.56789528916575,-5.91119922530853,8.0199645280426));
#8136=CARTESIAN_POINT('Ctrl Pts',(1.73050792712124,-5.86320457400819,8.02768961544995));
#8137=CARTESIAN_POINT('Ctrl Pts',(1.89249000783377,-5.81539602986029,8.03538474756061));
#8138=CARTESIAN_POINT('Ctrl Pts',(2.05247035474955,-5.76087650024044,8.04307987967126));
#8139=CARTESIAN_POINT('Ctrl Pts',(2.20989284155477,-5.69984203213957,8.05077501178192));
#8140=CARTESIAN_POINT('Ctrl Pts',(2.36792369396233,-5.63857169385457,8.05849988204356));
#8141=CARTESIAN_POINT('Ctrl Pts',(2.5234328366786,-5.5707142337554,8.0662247523052));
#8142=CARTESIAN_POINT('Ctrl Pts',(2.67587105519959,-5.49650249326288,8.07394962256685));
#8143=CARTESIAN_POINT('Ctrl Pts',(2.82827703775813,-5.42230644625525,8.08167285925766));
#8144=CARTESIAN_POINT('Ctrl Pts',(2.97761310740808,-5.34175893929577,8.08939609594846));
#8145=CARTESIAN_POINT('Ctrl Pts',(3.12335245258178,-5.25513986678294,8.09711933263927));
#8146=CARTESIAN_POINT('Ctrl Pts',(3.2690827895958,-5.16852614820137,8.10484209195625));
#8147=CARTESIAN_POINT('Ctrl Pts',(3.4112165726881,-5.07584177357938,8.11256485127323));
#8148=CARTESIAN_POINT('Ctrl Pts',(3.54925335581439,-4.97741159426667,8.12028761059021));
#8149=CARTESIAN_POINT('Ctrl Pts',(3.60789506958217,-4.93559582407384,8.12356844509756));
#8150=CARTESIAN_POINT('Ctrl Pts',(3.6657977138052,-4.89274360472679,8.1268492796049));
#8151=CARTESIAN_POINT('Ctrl Pts',(3.72292453512038,-4.84888218750453,8.13013011411225));
#8152=CARTESIAN_POINT('',(-6.11324999999769,5.31886132084791E-6,7.36474103251824));
#8153=CARTESIAN_POINT('Ctrl Pts',(-6.11324999999769,5.31793291456405E-6,
7.36474103256055));
#8154=CARTESIAN_POINT('Ctrl Pts',(-6.11325014740321,-0.169445255362402,
7.37246397694535));
#8155=CARTESIAN_POINT('Ctrl Pts',(-6.10620055882416,-0.338926118695248,
7.38018692133014));
#8156=CARTESIAN_POINT('Ctrl Pts',(-6.09211972579428,-0.507841322745799,
7.38790986571494));
#8157=CARTESIAN_POINT('Ctrl Pts',(-6.07804165032709,-0.676723446774617,
7.39563129765348));
#8158=CARTESIAN_POINT('Ctrl Pts',(-6.05693510430396,-0.845039816620301,
7.40335272959201));
#8159=CARTESIAN_POINT('Ctrl Pts',(-6.0288705499934,-1.01219832736588,7.41107416153055));
#8160=CARTESIAN_POINT('Ctrl Pts',(-6.00080494970368,-1.17936306818789,7.4187958812505));
#8161=CARTESIAN_POINT('Ctrl Pts',(-5.96578087081875,-1.3453695500608,7.42651760097044));
#8162=CARTESIAN_POINT('Ctrl Pts',(-5.92392026267643,-1.5096338244593,7.43423932069038));
#8163=CARTESIAN_POINT('Ctrl Pts',(-5.88206240640404,-1.67388730030668,7.44196053279304));
#8164=CARTESIAN_POINT('Ctrl Pts',(-5.83336899865677,-1.83639849045815,7.44968174489571));
#8165=CARTESIAN_POINT('Ctrl Pts',(-5.77801247941001,-1.99659644151795,7.45740295699837));
#8166=CARTESIAN_POINT('Ctrl Pts',(-5.72264136364105,-2.15683663390691,7.4651262050463));
#8167=CARTESIAN_POINT('Ctrl Pts',(-5.66060372734563,-2.3147620676604,7.47284945309423));
#8168=CARTESIAN_POINT('Ctrl Pts',(-5.5921213109299,-2.46981878006134,7.48057270114217));
#8169=CARTESIAN_POINT('Ctrl Pts',(-5.52582819395051,-2.61991851823695,7.48804904635748));
#8170=CARTESIAN_POINT('Ctrl Pts',(-5.45349612724275,-2.76732987301179,7.49552539157279));
#8171=CARTESIAN_POINT('Ctrl Pts',(-5.37536853871852,-2.91156978886907,7.5030017367881));
#8172=CARTESIAN_POINT('Ctrl Pts',(-5.29464500099184,-3.06060237146041,7.51072649889129));
#8173=CARTESIAN_POINT('Ctrl Pts',(-5.20770543635674,-3.20630217515723,7.51845126099449));
#8174=CARTESIAN_POINT('Ctrl Pts',(-5.11485012499966,-3.34815378399662,7.52617602309768));
#8175=CARTESIAN_POINT('Ctrl Pts',(-5.02201292681427,-3.4899777220167,7.533899278341));
#8176=CARTESIAN_POINT('Ctrl Pts',(-4.92326245797659,-3.62795469801437,7.54162253358432));
#8177=CARTESIAN_POINT('Ctrl Pts',(-4.8189428629313,-3.76159743278086,7.54934578882765));
#8178=CARTESIAN_POINT('Ctrl Pts',(-4.71461923643464,-3.89524533219723,7.5570693425377));
#8179=CARTESIAN_POINT('Ctrl Pts',(-4.60472624494501,-4.02455840295248,7.56479289624775));
#8180=CARTESIAN_POINT('Ctrl Pts',(-4.48964942152743,-4.14908105901516,7.5725164499578));
#8181=CARTESIAN_POINT('Ctrl Pts',(-4.37458032719155,-4.27359535157116,7.58023948491894));
#8182=CARTESIAN_POINT('Ctrl Pts',(-4.254328312797,-4.39331964052788,7.58796251988007));
#8183=CARTESIAN_POINT('Ctrl Pts',(-4.12931711911013,-4.50783381374291,7.59568555484121));
#8184=CARTESIAN_POINT('Ctrl Pts',(-4.00427270289438,-4.62237841983613,7.60341064224856));
#8185=CARTESIAN_POINT('Ctrl Pts',(-3.87446681243393,-4.73170992754462,7.61113572965592));
#8186=CARTESIAN_POINT('Ctrl Pts',(-3.74035845520799,-4.83544663801123,7.61886081706327));
#8187=CARTESIAN_POINT('Ctrl Pts',(-3.60677012518912,-4.93878109232519,7.62655594917394));
#8188=CARTESIAN_POINT('Ctrl Pts',(-3.46891290279384,-5.03656389624701,7.63425108128461));
#8189=CARTESIAN_POINT('Ctrl Pts',(-3.3272712997932,-5.12845895567786,7.64194621339527));
#8190=CARTESIAN_POINT('Ctrl Pts',(-3.18508430789232,-5.22070785567773,7.64967097549847));
#8191=CARTESIAN_POINT('Ctrl Pts',(-3.03903335938653,-5.30705622646052,7.65739573760167));
#8192=CARTESIAN_POINT('Ctrl Pts',(-2.88962872821693,-5.38719513063741,7.66512049970487));
#8193=CARTESIAN_POINT('Ctrl Pts',(-2.74025324122563,-5.46731840221647,7.6728437549482));
#8194=CARTESIAN_POINT('Ctrl Pts',(-2.58752565604764,-5.54123447439842,7.68056701019152));
#8195=CARTESIAN_POINT('Ctrl Pts',(-2.43198130352822,-5.60868010335669,7.68829026543485));
#8196=CARTESIAN_POINT('Ctrl Pts',(-2.27643093996662,-5.67612833876459,7.69601381914489));
#8197=CARTESIAN_POINT('Ctrl Pts',(-2.11806388042359,-5.73710550086938,7.70373737285494));
#8198=CARTESIAN_POINT('Ctrl Pts',(-1.95743663722948,-5.79139597797731,7.71146092656498));
#8199=CARTESIAN_POINT('Ctrl Pts',(-1.79682018249013,-5.84568280869036,7.7191839615261));
#8200=CARTESIAN_POINT('Ctrl Pts',(-1.63394414815684,-5.89328375166325,7.72690699648723));
#8201=CARTESIAN_POINT('Ctrl Pts',(-1.46938162599392,-5.93403262543201,7.73463003144835));
#8202=CARTESIAN_POINT('Ctrl Pts',(-1.30477537028179,-5.97479232847618,7.74235511885571));
#8203=CARTESIAN_POINT('Ctrl Pts',(-1.13848203846609,-6.00869624520714,7.75008020626306));
#8204=CARTESIAN_POINT('Ctrl Pts',(-0.971087312893186,-6.0356287984963,7.75780529367042));
#8205=CARTESIAN_POINT('Ctrl Pts',(-0.804341687893734,-6.06245691638151,
7.76550042578111));
#8206=CARTESIAN_POINT('Ctrl Pts',(-0.636503508969812,-6.08236762216965,
7.77319555789179));
#8207=CARTESIAN_POINT('Ctrl Pts',(-0.46815903580214,-6.09529758746009,7.78089069000247));
#8208=CARTESIAN_POINT('Ctrl Pts',(-0.29916635472732,-6.10827733939089,7.78861545210568));
#8209=CARTESIAN_POINT('Ctrl Pts',(-0.129603618233078,-6.1142270527368,7.79634021420888));
#8210=CARTESIAN_POINT('Ctrl Pts',(0.0399332841301361,-6.11311957148873,
7.80406497631209));
#8211=CARTESIAN_POINT('Ctrl Pts',(0.209437115137693,-6.11201230627567,7.81178823155542));
#8212=CARTESIAN_POINT('Ctrl Pts',(0.378914805342489,-6.10385059542405,7.81951148679875));
#8213=CARTESIAN_POINT('Ctrl Pts',(0.54777032320894,-6.08865939559043,7.82723474204209));
#8214=CARTESIAN_POINT('Ctrl Pts',(0.716632366530116,-6.07346760868989,7.83495829575214));
#8215=CARTESIAN_POINT('Ctrl Pts',(0.884871873401426,-6.05124581365886,7.84268184946219));
#8216=CARTESIAN_POINT('Ctrl Pts',(1.05189700087771,-6.02207092801509,7.85040540317224));
#8217=CARTESIAN_POINT('Ctrl Pts',(1.21891091018829,-5.99289800188906,7.85812843813337));
#8218=CARTESIAN_POINT('Ctrl Pts',(1.3847102910964,-5.95677297424082,7.86585147309449));
#8219=CARTESIAN_POINT('Ctrl Pts',(1.54871239069064,-5.91382410064937,7.87357450805561));
#8220=CARTESIAN_POINT('Ctrl Pts',(1.71275807489821,-5.87086381311838,7.88129959546298));
#8221=CARTESIAN_POINT('Ctrl Pts',(1.87500521599692,-5.82107613410619,7.88902468287035));
#8222=CARTESIAN_POINT('Ctrl Pts',(2.03488421555061,-5.76463977988243,7.89674977027771));
#8223=CARTESIAN_POINT('Ctrl Pts',(2.19414325799339,-5.70842226690244,7.90444490238836));
#8224=CARTESIAN_POINT('Ctrl Pts',(2.35105220830446,-5.64560768402968,7.91214003449901));
#8225=CARTESIAN_POINT('Ctrl Pts',(2.50506595839486,-5.57642090471937,7.91983516660965));
#8226=CARTESIAN_POINT('Ctrl Pts',(2.65967203777948,-5.50696803646484,7.92755989381924));
#8227=CARTESIAN_POINT('Ctrl Pts',(2.8114153475298,-5.43106923489391,7.93528462102883));
#8228=CARTESIAN_POINT('Ctrl Pts',(2.9597596364623,-5.34898574094833,7.94300934823842));
#8229=CARTESIAN_POINT('Ctrl Pts',(3.10808411080891,-5.2669132110274,7.95073304364374));
#8230=CARTESIAN_POINT('Ctrl Pts',(3.25301019191251,-5.17865778836112,7.95845673904906));
#8231=CARTESIAN_POINT('Ctrl Pts',(3.39402634211527,-5.084526600533,7.96618043445437));
#8232=CARTESIAN_POINT('Ctrl Pts',(3.50621497110141,-5.00963837750259,7.97232519728461));
#8233=CARTESIAN_POINT('Ctrl Pts',(3.61592928983639,-4.93103209513385,7.97846996011485));
#8234=CARTESIAN_POINT('Ctrl Pts',(3.72292453512037,-4.84888218750454,7.98461472294509));
#8235=CARTESIAN_POINT('Ctrl Pts',(3.72292453512037,-4.84888218750454,6.23460979329304));
#8236=CARTESIAN_POINT('Ctrl Pts',(3.82674007619718,-4.76917362580806,6.24057367796984));
#8237=CARTESIAN_POINT('Ctrl Pts',(3.92798420304844,-4.68613792056754,6.24653756264663));
#8238=CARTESIAN_POINT('Ctrl Pts',(4.02644658881525,-4.59995145951759,6.25250144732343));
#8239=CARTESIAN_POINT('Ctrl Pts',(4.15398066222203,-4.4883178609143,6.26022620942661));
#8240=CARTESIAN_POINT('Ctrl Pts',(4.27689188120749,-4.37135738492506,6.26795097152978));
#8241=CARTESIAN_POINT('Ctrl Pts',(4.3947438398315,-4.24947669069534,6.27567573363296));
#8242=CARTESIAN_POINT('Ctrl Pts',(4.51257280921926,-4.12761977158237,6.28339898887632));
#8243=CARTESIAN_POINT('Ctrl Pts',(4.62534426730198,-4.00084477703188,6.29112224411968));
#8244=CARTESIAN_POINT('Ctrl Pts',(4.73265893453336,-3.86959493640893,6.29884549936304));
#8245=CARTESIAN_POINT('Ctrl Pts',(4.83997774896067,-3.73834002361067,6.30656905307308));
#8246=CARTESIAN_POINT('Ctrl Pts',(4.94183914688451,-3.60261016153296,6.31429260678313));
#8247=CARTESIAN_POINT('Ctrl Pts',(5.03788389727962,-3.46288195005702,6.32201616049317));
#8248=CARTESIAN_POINT('Ctrl Pts',(5.13392219687341,-3.3231631233619,6.32973919545429));
#8249=CARTESIAN_POINT('Ctrl Pts',(5.22414445120127,-3.17944674588159,6.33746223041541));
#8250=CARTESIAN_POINT('Ctrl Pts',(5.30823446293605,-3.03223885091495,6.34518526537653));
#8251=CARTESIAN_POINT('Ctrl Pts',(5.39234682213254,-2.88499183450299,6.35291035278389));
#8252=CARTESIAN_POINT('Ctrl Pts',(5.47032352303129,-2.73425172075412,6.36063544019125));
#8253=CARTESIAN_POINT('Ctrl Pts',(5.54189361959266,-2.58055045903353,6.36836052759861));
#8254=CARTESIAN_POINT('Ctrl Pts',(5.61318619133598,-2.42744519922915,6.37605565970927));
#8255=CARTESIAN_POINT('Ctrl Pts',(5.67812165318492,-2.27140201192588,6.38375079181993));
#8256=CARTESIAN_POINT('Ctrl Pts',(5.73647916917479,-2.11296765335481,6.39144592393059));
#8257=CARTESIAN_POINT('Ctrl Pts',(5.79506138991806,-1.95392324562609,6.39917068603379));
#8258=CARTESIAN_POINT('Ctrl Pts',(5.84703562758219,-1.79241287656113,6.40689544813698));
#8259=CARTESIAN_POINT('Ctrl Pts',(5.89221322034706,-1.62900243353636,6.41462021024018));
#8260=CARTESIAN_POINT('Ctrl Pts',(5.93738200037424,-1.46562386678653,6.4223434654835));
#8261=CARTESIAN_POINT('Ctrl Pts',(5.97575669657398,-1.30034627092843,6.43006672072682));
#8262=CARTESIAN_POINT('Ctrl Pts',(6.00719874504435,-1.13374988425033,6.43778997597013));
#8263=CARTESIAN_POINT('Ctrl Pts',(6.03864200859886,-0.967147059422086,6.44551352968017));
#8264=CARTESIAN_POINT('Ctrl Pts',(6.06315202564524,-0.799225652475361,6.4532370833902));
#8265=CARTESIAN_POINT('Ctrl Pts',(6.08064136536425,-0.630576044836139,6.46096063710024));
#8266=CARTESIAN_POINT('Ctrl Pts',(6.09812953041987,-0.461937764469577,6.46868367206137));
#8267=CARTESIAN_POINT('Ctrl Pts',(6.10859792909061,-0.292571696553318,6.47640670702251));
#8268=CARTESIAN_POINT('Ctrl Pts',(6.11201100137875,-0.123073480186015,6.48412974198364));
#8269=CARTESIAN_POINT('Ctrl Pts',(6.11542498071282,0.0464697814227938,6.491854829391));
#8270=CARTESIAN_POINT('Ctrl Pts',(6.11177987839815,0.216144944617681,6.49957991679836));
#8271=CARTESIAN_POINT('Ctrl Pts',(6.10109226977798,0.385355262265019,6.50730500420572));
#8272=CARTESIAN_POINT('Ctrl Pts',(6.09044610411762,0.553909439082053,6.51500013631641));
#8273=CARTESIAN_POINT('Ctrl Pts',(6.07281200386748,0.722002059437204,6.52269526842709));
#8274=CARTESIAN_POINT('Ctrl Pts',(6.04825763137341,0.889047348026707,6.53039040053778));
#8275=CARTESIAN_POINT('Ctrl Pts',(6.02360871263081,1.05673584203206,6.53811516264098));
#8276=CARTESIAN_POINT('Ctrl Pts',(5.99197736342121,1.22342830869872,6.54583992474417));
#8277=CARTESIAN_POINT('Ctrl Pts',(5.95346865194615,1.38853756621652,6.55356468684737));
#8278=CARTESIAN_POINT('Ctrl Pts',(5.91496745231817,1.55361461607414,6.5612879420907));
#8279=CARTESIAN_POINT('Ctrl Pts',(5.86959163925624,1.71710876456313,6.56901119733403));
#8280=CARTESIAN_POINT('Ctrl Pts',(5.81749713914765,1.87844419627224,6.57673445257736));
#8281=CARTESIAN_POINT('Ctrl Pts',(5.76540062583691,2.03978586282069,6.58445800628741));
#8282=CARTESIAN_POINT('Ctrl Pts',(5.70658499952515,2.19896834284973,6.59218155999745));
#8283=CARTESIAN_POINT('Ctrl Pts',(5.64125594066812,2.35543137755629,6.59990511370749));
#8284=CARTESIAN_POINT('Ctrl Pts',(5.57593126960733,2.51188390349494,6.6076281486686));
#8285=CARTESIAN_POINT('Ctrl Pts',(5.50409416358331,2.66561705714119,6.6153511836297));
#8286=CARTESIAN_POINT('Ctrl Pts',(5.42599836759865,2.81609077931035,6.6230742185908));
#8287=CARTESIAN_POINT('Ctrl Pts',(5.34788181715341,2.96660449083996,6.63079930599817));
#8288=CARTESIAN_POINT('Ctrl Pts',(5.26350339725766,3.11385675748476,6.63852439340554));
#8289=CARTESIAN_POINT('Ctrl Pts',(5.17316316443419,3.25733149013748,6.64624948081291));
#8290=CARTESIAN_POINT('Ctrl Pts',(5.08317324071836,3.40024987592243,6.6539446129236));
#8291=CARTESIAN_POINT('Ctrl Pts',(4.98726785132823,3.53941972465211,6.66163974503429));
#8292=CARTESIAN_POINT('Ctrl Pts',(4.88578666437294,3.67435902338564,6.66933487714498));
#8293=CARTESIAN_POINT('Ctrl Pts',(4.7839147256064,3.80981790389558,6.67705963924818));
#8294=CARTESIAN_POINT('Ctrl Pts',(4.67638786097806,3.94106154785416,6.68478440135139));
#8295=CARTESIAN_POINT('Ctrl Pts',(4.56357925856923,4.06762460328589,6.6925091634546));
#8296=CARTESIAN_POINT('Ctrl Pts',(4.450792661597,4.19416297021663,6.70023241869788));
#8297=CARTESIAN_POINT('Ctrl Pts',(4.332726593414,4.31602233401184,6.70795567394115));
#8298=CARTESIAN_POINT('Ctrl Pts',(4.20979346398447,4.43277165587104,6.71567892918443));
#8299=CARTESIAN_POINT('Ctrl Pts',(4.08685558377908,4.54952548953158,6.72340248289448));
#8300=CARTESIAN_POINT('Ctrl Pts',(3.95905049302257,4.66116866497647,6.73112603660453));
#8301=CARTESIAN_POINT('Ctrl Pts',(3.82682684928917,4.76730760787045,6.73884959031458));
#8302=CARTESIAN_POINT('Ctrl Pts',(3.69461208629594,4.87343942199119,6.7465726252757));
#8303=CARTESIAN_POINT('Ctrl Pts',(3.55797961138892,4.97406754496306,6.75429566023682));
#8304=CARTESIAN_POINT('Ctrl Pts',(3.41741062478746,5.06883913574793,6.76201869519794));
#8305=CARTESIAN_POINT('Ctrl Pts',(3.27680428107322,5.16363591269292,6.76974378260531));
#8306=CARTESIAN_POINT('Ctrl Pts',(3.13225959694467,5.25257286826412,6.77746887001267));
#8307=CARTESIAN_POINT('Ctrl Pts',(2.98428697198997,5.33534036695982,6.78519395742003));
#8308=CARTESIAN_POINT('Ctrl Pts',(2.83688813521952,5.41778692106995,6.79288908953074));
#8309=CARTESIAN_POINT('Ctrl Pts',(2.6860881833734,5.49411165515322,6.80058422164145));
#8310=CARTESIAN_POINT('Ctrl Pts',(2.53241599697323,5.56405380822059,6.80827935375216));
#8311=CARTESIAN_POINT('Ctrl Pts',(2.37815209809004,5.63426527251486,6.81600411585536));
#8312=CARTESIAN_POINT('Ctrl Pts',(2.22093915363002,5.69806974563762,6.82372887795856));
#8313=CARTESIAN_POINT('Ctrl Pts',(2.0613275077843,5.75523713396344,6.83145364006176));
#8314=CARTESIAN_POINT('Ctrl Pts',(1.90174699718607,5.81239337071713,6.83917689530511));
#8315=CARTESIAN_POINT('Ctrl Pts',(1.73976901703855,5.8629149992405,6.84690015054846));
#8316=CARTESIAN_POINT('Ctrl Pts',(1.57596193686568,5.90662082209875,6.85462340579181));
#8317=CARTESIAN_POINT('Ctrl Pts',(1.41214852633633,5.95032833397704,6.86234695950187));
#8318=CARTESIAN_POINT('Ctrl Pts',(1.24650617951962,5.98721942758742,6.87007051321192));
#8319=CARTESIAN_POINT('Ctrl Pts',(1.07961717181621,6.01716314593676,6.87779406692198));
#8320=CARTESIAN_POINT('Ctrl Pts',(0.912739373136056,6.04710485313007,6.88551710188311));
#8321=CARTESIAN_POINT('Ctrl Pts',(0.744615393106126,6.07010006287075,6.89324013684424));
#8322=CARTESIAN_POINT('Ctrl Pts',(0.575836595672656,6.08606915649043,6.90096317180537));
#8323=CARTESIAN_POINT('Ctrl Pts',(0.407012944188079,6.10204249399946,6.90868825921272));
#8324=CARTESIAN_POINT('Ctrl Pts',(0.237534443096473,6.11098595215364,6.91641334662007));
#8325=CARTESIAN_POINT('Ctrl Pts',(0.0679974262798713,6.11287182202599,6.92413843402742));
#8326=CARTESIAN_POINT('Ctrl Pts',(-0.100882182876039,6.1147503791278,6.93183356613806));
#8327=CARTESIAN_POINT('Ctrl Pts',(-0.26981954222674,6.10962601333181,6.93952869824871));
#8328=CARTESIAN_POINT('Ctrl Pts',(-0.438225472296301,6.09752277551554,6.94722383035936));
#8329=CARTESIAN_POINT('Ctrl Pts',(-0.607279846912093,6.08537293436082,6.95494859246253));
#8330=CARTESIAN_POINT('Ctrl Pts',(-0.775858563478678,6.06618603735116,6.96267335456571));
#8331=CARTESIAN_POINT('Ctrl Pts',(-0.94336826687528,6.04002333402386,6.97039811666888));
#8332=CARTESIAN_POINT('Ctrl Pts',(-1.11084529436024,6.01386573422289,6.97812137191222));
#8333=CARTESIAN_POINT('Ctrl Pts',(-1.27725341182941,5.98073509218863,6.98584462715556));
#8334=CARTESIAN_POINT('Ctrl Pts',(-1.44200682901433,5.94074421832619,6.9935678823989));
#8335=CARTESIAN_POINT('Ctrl Pts',(-1.60676661312709,5.90075179900865,7.00129143610895));
#8336=CARTESIAN_POINT('Ctrl Pts',(-1.7698712600859,5.85389868825748,7.00901498981898));
#8337=CARTESIAN_POINT('Ctrl Pts',(-1.93074680500557,5.80034846689927,7.01673854352903));
#8338=CARTESIAN_POINT('Ctrl Pts',(-2.09161154479325,5.74680184221706,7.02446157849013));
#8339=CARTESIAN_POINT('Ctrl Pts',(-2.25024718141715,5.6865591071788,7.03218461345124));
#8340=CARTESIAN_POINT('Ctrl Pts',(-2.40609633085892,5.61983327236024,7.03990764841235));
#8341=CARTESIAN_POINT('Ctrl Pts',(-2.56198689821528,5.5530897047216,7.04763273581971));
#8342=CARTESIAN_POINT('Ctrl Pts',(-2.71508920622712,5.47985971730165,7.05535782322707));
#8343=CARTESIAN_POINT('Ctrl Pts',(-2.86486634178415,5.40040428173783,7.06308291063443));
#8344=CARTESIAN_POINT('Ctrl Pts',(-3.01406269187019,5.32125694769028,7.07077804274513));
#8345=CARTESIAN_POINT('Ctrl Pts',(-3.15995935078779,5.2359325348516,7.07847317485582));
#8346=CARTESIAN_POINT('Ctrl Pts',(-3.30205045130174,5.14473404361761,7.08616830696652));
#8347=CARTESIAN_POINT('Ctrl Pts',(-3.44468867149895,5.0531843939405,7.09389306906973));
#8348=CARTESIAN_POINT('Ctrl Pts',(-3.58354247061905,4.95568289053558,7.10161783117293));
#8349=CARTESIAN_POINT('Ctrl Pts',(-3.71812011161081,4.85256719666356,7.10934259327613));
#8350=CARTESIAN_POINT('Ctrl Pts',(-3.85267150070687,4.74947161744372,7.11706584851944));
#8351=CARTESIAN_POINT('Ctrl Pts',(-3.98294814467582,4.64076422561949,7.12478910376276));
#8352=CARTESIAN_POINT('Ctrl Pts',(-4.10848961758786,4.526824342149,7.13251235900607));
#8353=CARTESIAN_POINT('Ctrl Pts',(-4.23403594207518,4.41288005544898,7.14023591271613));
#8354=CARTESIAN_POINT('Ctrl Pts',(-4.35484649199016,4.29370308252234,7.14795946642618));
#8355=CARTESIAN_POINT('Ctrl Pts',(-4.47049551563522,4.16971166955048,7.15568302013624));
#8356=CARTESIAN_POINT('Ctrl Pts',(-4.58613677176657,4.04572858440508,7.16340605509734));
#8357=CARTESIAN_POINT('Ctrl Pts',(-4.69661697918975,3.91693193809907,7.17112909005845));
#8358=CARTESIAN_POINT('Ctrl Pts',(-4.80154859493683,3.78377544959531,7.17885212501956));
#8359=CARTESIAN_POINT('Ctrl Pts',(-4.90650809693604,3.65058357389785,7.1865772124269));
#8360=CARTESIAN_POINT('Ctrl Pts',(-5.0059158626915,3.51302978847744,7.19430229983425));
#8361=CARTESIAN_POINT('Ctrl Pts',(-5.09942527124864,3.37160013427611,7.20202738724159));
#8362=CARTESIAN_POINT('Ctrl Pts',(-5.19257208169858,3.23071889681388,7.2097225193523));
#8363=CARTESIAN_POINT('Ctrl Pts',(-5.27986605204589,3.08599207396941,7.21741765146301));
#8364=CARTESIAN_POINT('Ctrl Pts',(-5.36100793131647,2.93792775998013,7.22511278357372));
#8365=CARTESIAN_POINT('Ctrl Pts',(-5.44246224619427,2.78929332653756,7.23283754567692));
#8366=CARTESIAN_POINT('Ctrl Pts',(-5.51774582123992,2.63724299268517,7.24056230778012));
#8367=CARTESIAN_POINT('Ctrl Pts',(-5.58658839729109,2.48230853073357,7.24828706988332));
#8368=CARTESIAN_POINT('Ctrl Pts',(-5.65541754430528,2.32740429165766,7.25601032512664));
#8369=CARTESIAN_POINT('Ctrl Pts',(-5.71780807075731,2.16961733652475,7.26373358036996));
#8370=CARTESIAN_POINT('Ctrl Pts',(-5.77353714285875,2.00950103820087,7.27145683561328));
#8371=CARTESIAN_POINT('Ctrl Pts',(-5.82926836862119,1.84937855215102,7.27918038932332));
#8372=CARTESIAN_POINT('Ctrl Pts',(-5.87833751697747,1.68692684078353,7.28690394303336));
#8373=CARTESIAN_POINT('Ctrl Pts',(-5.92057082545285,1.52271686905236,7.29462749674341));
#8374=CARTESIAN_POINT('Ctrl Pts',(-5.96280129734756,1.3585179264081,7.30235053170453));
#8375=CARTESIAN_POINT('Ctrl Pts',(-5.99819676920487,1.19256126669211,7.31007356666565));
#8376=CARTESIAN_POINT('Ctrl Pts',(-6.02663400184908,1.02543072426009,7.31779660162678));
#8377=CARTESIAN_POINT('Ctrl Pts',(-6.05507879187085,0.85825576581093,7.32552168903414));
#8378=CARTESIAN_POINT('Ctrl Pts',(-6.07656159218805,0.689906613550995,7.33324677644151));
#8379=CARTESIAN_POINT('Ctrl Pts',(-6.09101056209332,0.520975906321606,7.34097186384887));
#8380=CARTESIAN_POINT('Ctrl Pts',(-6.10540350374189,0.352700255687394,7.34866699595955));
#8381=CARTESIAN_POINT('Ctrl Pts',(-6.11281707319215,0.183847866016913,7.35636212807023));
#8382=CARTESIAN_POINT('Ctrl Pts',(-6.11323157749471,0.0150080785417984,
7.3640572601809));
#8383=CARTESIAN_POINT('Ctrl Pts',(-6.11324385480432,0.0100071694253899,
7.36428518427924));
#8384=CARTESIAN_POINT('Ctrl Pts',(-6.11324999564585,0.0050062452407887,
7.36451310837758));
#8385=CARTESIAN_POINT('Ctrl Pts',(-6.11324999999769,5.31978972713177E-6,
7.36474103247592));
#8386=CARTESIAN_POINT('Origin',(0.,0.,-3.86474103256053));
#8387=CARTESIAN_POINT('',(3.72292453512037,-4.84888218750453,4.4846183003358));
#8388=CARTESIAN_POINT('',(3.72292453512038,-4.84888218750453,4.63013458917765));
#8389=CARTESIAN_POINT('',(3.72292453512038,-4.84888218750453,-3.86474103256053));
#8390=CARTESIAN_POINT('',(-6.11319920576163,-1.41071580853158E-5,5.76025896758647));
#8391=CARTESIAN_POINT('Ctrl Pts',(3.72292453512038,-4.84888218750453,4.63013458917765));
#8392=CARTESIAN_POINT('Ctrl Pts',(3.85740293170725,-4.74563098387927,4.63785792890056));
#8393=CARTESIAN_POINT('Ctrl Pts',(3.98758890164652,-4.6367776533406,4.64558126862347));
#8394=CARTESIAN_POINT('Ctrl Pts',(4.11302426972855,-4.52270460224011,4.65330460834637));
#8395=CARTESIAN_POINT('Ctrl Pts',(4.23845419774736,-4.40863649842539,4.66102761311227));
#8396=CARTESIAN_POINT('Ctrl Pts',(4.35913370250064,-4.28934934113618,4.66875061787816));
#8397=CARTESIAN_POINT('Ctrl Pts',(4.47463982938566,-4.16526397240024,4.67647362264406));
#8398=CARTESIAN_POINT('Ctrl Pts',(4.59017383948617,-4.04114864941713,4.68419849174574));
#8399=CARTESIAN_POINT('Ctrl Pts',(4.70053175983779,-3.91223303220383,4.69192336084742));
#8400=CARTESIAN_POINT('Ctrl Pts',(4.80532886836392,-3.77897340945505,4.6996482299491));
#8401=CARTESIAN_POINT('Ctrl Pts',(4.87975910829058,-3.68432818657416,4.70513467770254));
#8402=CARTESIAN_POINT('Ctrl Pts',(4.95138511255325,-3.5874924626389,4.71062112545598));
#8403=CARTESIAN_POINT('Ctrl Pts',(5.02008170643796,-3.48863945158953,4.71610757320942));
#8404=CARTESIAN_POINT('Ctrl Pts',(5.11680455315176,-3.34945722880027,4.72383233531262));
#8405=CARTESIAN_POINT('Ctrl Pts',(5.20775270115482,-3.20622540597074,4.73155709741581));
#8406=CARTESIAN_POINT('Ctrl Pts',(5.29260114598734,-3.05944417696965,4.73928185951901));
#8407=CARTESIAN_POINT('Ctrl Pts',(5.3774330395378,-2.91269158040286,4.74700511476234));
#8408=CARTESIAN_POINT('Ctrl Pts',(5.45616744560474,-2.76239123342247,4.75472837000567));
#8409=CARTESIAN_POINT('Ctrl Pts',(5.52852423355157,-2.60906982687951,4.76245162524899));
#8410=CARTESIAN_POINT('Ctrl Pts',(5.60088381774069,-2.45574249520064,4.77017517895904));
#8411=CARTESIAN_POINT('Ctrl Pts',(5.66686515178002,-2.29939415525088,4.77789873266908));
#8412=CARTESIAN_POINT('Ctrl Pts',(5.72623503965873,-2.14057418303701,4.78562228637913));
#8413=CARTESIAN_POINT('Ctrl Pts',(5.78560093998629,-1.98176487789336,4.79334532134025));
#8414=CARTESIAN_POINT('Ctrl Pts',(5.83835617180195,-1.82048456958474,4.80106835630137));
#8415=CARTESIAN_POINT('Ctrl Pts',(5.8843164172226,-1.65730077671634,4.80879139126249));
#8416=CARTESIAN_POINT('Ctrl Pts',(5.93028887687421,-1.49407361670494,4.81651647866985));
#8417=CARTESIAN_POINT('Ctrl Pts',(5.96946265360397,-1.32894226597837,4.82424156607721));
#8418=CARTESIAN_POINT('Ctrl Pts',(6.00170360798695,-1.16248843623341,4.83196665348456));
#8419=CARTESIAN_POINT('Ctrl Pts',(6.03381954276788,-0.996680058583567,4.83966178559525));
#8420=CARTESIAN_POINT('Ctrl Pts',(6.05905629822593,-0.82955975256591,4.84735691770593));
#8421=CARTESIAN_POINT('Ctrl Pts',(6.07733193889542,-0.661711468074713,4.85505204981662));
#8422=CARTESIAN_POINT('Ctrl Pts',(6.09567794964934,-0.493216886243646,4.86277681191982));
#8423=CARTESIAN_POINT('Ctrl Pts',(6.10701559962199,-0.32392902965204,4.87050157402302));
#8424=CARTESIAN_POINT('Ctrl Pts',(6.11129880128841,-0.154442623232287,4.87822633612622));
#8425=CARTESIAN_POINT('Ctrl Pts',(6.11558116743593,0.0150107216820271,4.88594959136955));
#8426=CARTESIAN_POINT('Ctrl Pts',(6.11281182309288,0.18466222250966,4.89367284661288));
#8427=CARTESIAN_POINT('Ctrl Pts',(6.10299676254115,0.353915355575724,4.90139610185621));
#8428=CARTESIAN_POINT('Ctrl Pts',(6.09318132268446,0.52317502946243,4.90911965556626));
#8429=CARTESIAN_POINT('Ctrl Pts',(6.07631963615679,0.692035988165516,4.91684320927631));
#8430=CARTESIAN_POINT('Ctrl Pts',(6.05246976500209,0.85990424248026,4.92456676298636));
#8431=CARTESIAN_POINT('Ctrl Pts',(6.02862149571299,1.0277612220011,4.93228979794748));
#8432=CARTESIAN_POINT('Ctrl Pts',(5.99778602564995,1.19462531675511,4.94001283290861));
#8433=CARTESIAN_POINT('Ctrl Pts',(5.96007301796655,1.35990999077407,4.94773586786973));
#8434=CARTESIAN_POINT('Ctrl Pts',(5.92234998780869,1.52523859025868,4.95546095527709));
#8435=CARTESIAN_POINT('Ctrl Pts',(5.87774583616835,1.68898662057517,4.96318604268445));
#8436=CARTESIAN_POINT('Ctrl Pts',(5.82642107960329,1.85057908927299,4.97091113009181));
#8437=CARTESIAN_POINT('Ctrl Pts',(5.77529534322139,2.011544956602,4.97860626220248));
#8438=CARTESIAN_POINT('Ctrl Pts',(5.71750115499425,2.17037166190213,4.98630139431314));
#8439=CARTESIAN_POINT('Ctrl Pts',(5.65324594395815,2.32650722320407,4.99399652642381));
#8440=CARTESIAN_POINT('Ctrl Pts',(5.588743319181,2.48324398217871,5.00172128852701));
#8441=CARTESIAN_POINT('Ctrl Pts',(5.51770694400194,2.63732433166466,5.00944605063021));
#8442=CARTESIAN_POINT('Ctrl Pts',(5.44038088156317,2.78820397855356,5.01717081273341));
#8443=CARTESIAN_POINT('Ctrl Pts',(5.36306990302458,2.93905419353479,5.02489406797675));
#8444=CARTESIAN_POINT('Ctrl Pts',(5.27947182983405,3.08670466986316,5.03261732322008));
#8445=CARTESIAN_POINT('Ctrl Pts',(5.18987732009901,3.2306344523672,5.04034057846341));
#8446=CARTESIAN_POINT('Ctrl Pts',(5.10027934796653,3.37456979706599,5.04806413217346));
#8447=CARTESIAN_POINT('Ctrl Pts',(5.0046846396936,3.51478388907138,5.05578768588351));
#8448=CARTESIAN_POINT('Ctrl Pts',(4.90342836288413,3.65078290953645,5.06351123959356));
#8449=CARTESIAN_POINT('Ctrl Pts',(4.80217888690586,3.78677279568995,5.07123427455468));
#8450=CARTESIAN_POINT('Ctrl Pts',(4.69526879263646,3.91854792261217,5.0789573095158));
#8451=CARTESIAN_POINT('Ctrl Pts',(4.58307499411493,4.04564570381768,5.08668034447692));
#8452=CARTESIAN_POINT('Ctrl Pts',(4.47085137936944,4.17277726207644,5.09440543188428));
#8453=CARTESIAN_POINT('Ctrl Pts',(4.3533414627329,4.29522875152499,5.10213051929164));
#8454=CARTESIAN_POINT('Ctrl Pts',(4.23096129118955,4.41257205209792,5.10985560669901));
#8455=CARTESIAN_POINT('Ctrl Pts',(4.10905566888494,4.52946033472753,5.11755073880967));
#8456=CARTESIAN_POINT('Ctrl Pts',(3.98231774261072,4.64127978094795,5.12524587092034));
#8457=CARTESIAN_POINT('Ctrl Pts',(3.851193745536,4.74764492109977,5.132941003031));
#8458=CARTESIAN_POINT('Ctrl Pts',(3.7195648574473,4.85441961865268,5.1406657651342));
#8459=CARTESIAN_POINT('Ctrl Pts',(3.58346941655499,4.95573571640908,5.14839052723739));
#8460=CARTESIAN_POINT('Ctrl Pts',(3.44338214681699,5.05123202332679,5.15611528934059));
#8461=CARTESIAN_POINT('Ctrl Pts',(3.30332220373084,5.14670970189706,5.16383854458392));
#8462=CARTESIAN_POINT('Ctrl Pts',(3.15927224725646,5.23636967647257,5.17156179982725));
#8463=CARTESIAN_POINT('Ctrl Pts',(3.01173675205558,5.31989354205681,5.17928505507058));
#8464=CARTESIAN_POINT('Ctrl Pts',(2.86419555531649,5.40342063543725,5.18700860878062));
#8465=CARTESIAN_POINT('Ctrl Pts',(2.71316882414718,5.48081098573346,5.19473216249067));
#8466=CARTESIAN_POINT('Ctrl Pts',(2.55918713534885,5.55179131170877,5.20245571620071));
#8467=CARTESIAN_POINT('Ctrl Pts',(2.4052157886596,5.62276687032323,5.21017875116184));
#8468=CARTESIAN_POINT('Ctrl Pts',(2.24829016935885,5.6873331334887,5.21790178612296));
#8469=CARTESIAN_POINT('Ctrl Pts',(2.08896257040708,5.74526421863592,5.22562482108408));
#8470=CARTESIAN_POINT('Ctrl Pts',(1.92959262912074,5.80321069934176,5.23334990849144));
#8471=CARTESIAN_POINT('Ctrl Pts',(1.7678197299364,5.85451836802344,5.2410749958988));
#8472=CARTESIAN_POINT('Ctrl Pts',(1.60421403973201,5.89901033032039,5.24880008330615));
#8473=CARTESIAN_POINT('Ctrl Pts',(1.44124275749345,5.94332976771762,5.25649521541683));
#8474=CARTESIAN_POINT('Ctrl Pts',(1.27645318257264,5.9808862119964,5.26419034752751));
#8475=CARTESIAN_POINT('Ctrl Pts',(1.1104215839229,6.01155466318474,5.27188547963819));
#8476=CARTESIAN_POINT('Ctrl Pts',(0.943750683055199,6.04234120279134,5.27961024174139));
#8477=CARTESIAN_POINT('Ctrl Pts',(0.775769139355649,6.06619747392887,5.28733500384459));
#8478=CARTESIAN_POINT('Ctrl Pts',(0.607066624682404,6.08303342713952,5.29505976594779));
#8479=CARTESIAN_POINT('Ctrl Pts',(0.438397018601847,6.09986609618141,5.30278302119112));
#8480=CARTESIAN_POINT('Ctrl Pts',(0.269007037341032,6.10968114837651,5.31050627643444));
#8481=CARTESIAN_POINT('Ctrl Pts',(0.0994920075322081,6.11244033941741,5.31822953167777));
#8482=CARTESIAN_POINT('Ctrl Pts',(-0.0700295732183527,6.11519963708779,
5.32595308538781));
#8483=CARTESIAN_POINT('Ctrl Pts',(-0.239675895375619,6.11090251884586,5.33367663909786));
#8484=CARTESIAN_POINT('Ctrl Pts',(-0.408850299863663,6.0995628527626,5.34140019280791));
#8485=CARTESIAN_POINT('Ctrl Pts',(-0.578013341830746,6.08822394830279,5.34912322776903));
#8486=CARTESIAN_POINT('Ctrl Pts',(-0.746704213310474,6.06984346377552,5.35684626273015));
#8487=CARTESIAN_POINT('Ctrl Pts',(-0.914329862609266,6.04448727890471,5.36456929769127));
#8488=CARTESIAN_POINT('Ctrl Pts',(-1.08200005950303,6.01912435546461,5.37229438509863));
#8489=CARTESIAN_POINT('Ctrl Pts',(-1.24860415462535,5.98678207254353,5.38001947250599));
#8490=CARTESIAN_POINT('Ctrl Pts',(-1.41355683812085,5.94757787909513,5.38774455991335));
#8491=CARTESIAN_POINT('Ctrl Pts',(-1.57786989046229,5.90852570635333,5.39543969202402));
#8492=CARTESIAN_POINT('Ctrl Pts',(-1.74054401937625,5.86266484840827,5.40313482413469));
#8493=CARTESIAN_POINT('Ctrl Pts',(-1.90101338440889,5.81016124344224,5.41082995624536));
#8494=CARTESIAN_POINT('Ctrl Pts',(-2.06210063436128,5.75745547412082,5.41855471834856));
#8495=CARTESIAN_POINT('Ctrl Pts',(-2.2210231508804,5.69803700527917,5.42627948045175));
#8496=CARTESIAN_POINT('Ctrl Pts',(-2.37722004541994,5.63210887840014,5.43400424255495));
#8497=CARTESIAN_POINT('Ctrl Pts',(-2.5333864708227,5.56619361204,5.44172749779827));
#8498=CARTESIAN_POINT('Ctrl Pts',(-2.68682804333982,5.49377134457642,5.44945075304159));
#8499=CARTESIAN_POINT('Ctrl Pts',(-2.83700369391927,5.4150933143565,5.45717400828491));
#8500=CARTESIAN_POINT('Ctrl Pts',(-2.98718514806639,5.33641224360856,5.46489756199496));
#8501=CARTESIAN_POINT('Ctrl Pts',(-3.13410014515453,5.25147506990209,5.47262111570501));
#8502=CARTESIAN_POINT('Ctrl Pts',(-3.27723137816399,5.16057943030406,5.48034466941505));
#8503=CARTESIAN_POINT('Ctrl Pts',(-3.42035299783036,5.06968989566964,5.48806770437618));
#8504=CARTESIAN_POINT('Ctrl Pts',(-3.55969109442315,4.97284286592676,5.49579073933731));
#8505=CARTESIAN_POINT('Ctrl Pts',(-3.69475641255519,4.87037992505537,5.50351377429844));
#8506=CARTESIAN_POINT('Ctrl Pts',(-3.82985762516441,4.76788975399828,5.5112388617058));
#8507=CARTESIAN_POINT('Ctrl Pts',(-3.96068353628313,4.65978087945045,5.51896394911315));
#8508=CARTESIAN_POINT('Ctrl Pts',(-4.0867763610621,4.54643646575689,5.52668903652051));
#8509=CARTESIAN_POINT('Ctrl Pts',(-4.21238024017934,4.43353156366484,5.53438416863119));
#8510=CARTESIAN_POINT('Ctrl Pts',(-4.3332874637223,4.31543188625376,5.54207930074187));
#8511=CARTESIAN_POINT('Ctrl Pts',(-4.44908054209656,4.19255386279506,5.54977443285255));
#8512=CARTESIAN_POINT('Ctrl Pts',(-4.56531948000866,4.06920269932213,5.55749919495576));
#8513=CARTESIAN_POINT('Ctrl Pts',(-4.67644595721203,3.94099261094878,5.56522395705897));
#8514=CARTESIAN_POINT('Ctrl Pts',(-4.7820645838156,3.80837023918585,5.57294871916217));
#8515=CARTESIAN_POINT('Ctrl Pts',(-4.887662607523,3.6757737379066,5.5806719744055));
#8516=CARTESIAN_POINT('Ctrl Pts',(-4.98775472714699,3.5387669184038,5.58839522964882));
#8517=CARTESIAN_POINT('Ctrl Pts',(-5.08198601560127,3.39782926288728,5.59611848489214));
#8518=CARTESIAN_POINT('Ctrl Pts',(-5.17622094564231,3.25688616080722,5.60384203860218));
#8519=CARTESIAN_POINT('Ctrl Pts',(-5.26459441184698,3.11201217999068,5.61156559231223));
#8520=CARTESIAN_POINT('Ctrl Pts',(-5.34679455169444,2.96371617812345,5.61928914602228));
#8521=CARTESIAN_POINT('Ctrl Pts',(-5.42898917060749,2.81543013648866,5.62701218098341));
#8522=CARTESIAN_POINT('Ctrl Pts',(-5.50501113924724,2.66372281096924,5.63473521594454));
#8523=CARTESIAN_POINT('Ctrl Pts',(-5.5745942534521,2.50912822946114,5.64245825090566));
#8524=CARTESIAN_POINT('Ctrl Pts',(-5.6441958598173,2.35449256344825,5.65018333831303));
#8525=CARTESIAN_POINT('Ctrl Pts',(-5.70735506026154,2.1969683964917,5.65790842572039));
#8526=CARTESIAN_POINT('Ctrl Pts',(-5.76385317898686,2.03711121286567,5.66563351312776));
#8527=CARTESIAN_POINT('Ctrl Pts',(-5.82013221696651,1.87787390175539,5.67332864523842));
#8528=CARTESIAN_POINT('Ctrl Pts',(-5.86980166664037,1.71632194021236,5.68102377734908));
#8529=CARTESIAN_POINT('Ctrl Pts',(-5.91269415143927,1.55302074488264,5.68871890945974));
#8530=CARTESIAN_POINT('Ctrl Pts',(-5.95622561344383,1.38728682172284,5.69652867736351));
#8531=CARTESIAN_POINT('Ctrl Pts',(-5.99279060141521,1.21969844586006,5.70433844526727));
#8532=CARTESIAN_POINT('Ctrl Pts',(-6.02225374567939,1.05084983948734,5.71214821317104));
#8533=CARTESIAN_POINT('Ctrl Pts',(-6.05250419851263,0.877489292587187,5.72016667221578));
#8534=CARTESIAN_POINT('Ctrl Pts',(-6.07526787912564,0.702800542431067,5.72818513126051));
#8535=CARTESIAN_POINT('Ctrl Pts',(-6.09045444039747,0.527437457849552,5.73620359030525));
#8536=CARTESIAN_POINT('Ctrl Pts',(-6.10564100166929,0.352074373268037,5.74422204934998));
#8537=CARTESIAN_POINT('Ctrl Pts',(-6.11325040615677,0.176037297326452,5.75224050839472));
#8538=CARTESIAN_POINT('Ctrl Pts',(-6.11324999998373,-1.4104047642468E-5,
5.76025896743945));
#8539=CARTESIAN_POINT('Ctrl Pts',(-6.11272873999193,-1.41359676000207E-5,
5.76025896894818));
#8540=CARTESIAN_POINT('Ctrl Pts',(-6.11276834790607,-0.493277251017307,
5.78272710798777));
#8541=CARTESIAN_POINT('Ctrl Pts',(-5.9321396680783,-2.00330256368141,5.85151007256308));
#8542=CARTESIAN_POINT('Ctrl Pts',(-4.70225644657925,-4.30111769607244,5.96660786267411));
#8543=CARTESIAN_POINT('Ctrl Pts',(-2.071393642429,-6.02662073661255,6.1055523392813));
#8544=CARTESIAN_POINT('Ctrl Pts',(1.03946149232852,-6.28111086285485,6.24339327091069));
#8545=CARTESIAN_POINT('Ctrl Pts',(2.93620164665179,-5.45327201018824,6.33491937700434));
#8546=CARTESIAN_POINT('Ctrl Pts',(3.72323907905155,-4.84929205898333,6.38013065756227));
#8547=CARTESIAN_POINT('',(-6.11324999945666,8.15052733732165E-5,5.61474103252431));
#8548=CARTESIAN_POINT('Ctrl Pts',(-6.11324999945667,8.15044776936738E-5,
5.61474103256055));
#8549=CARTESIAN_POINT('Ctrl Pts',(-6.11325227041943,-0.170252242020816,
5.62249939646803));
#8550=CARTESIAN_POINT('Ctrl Pts',(-6.10613117300444,-0.340583666322338,
5.63025776037552));
#8551=CARTESIAN_POINT('Ctrl Pts',(-6.09191333408529,-0.510311172221234,
5.638016124283));
#8552=CARTESIAN_POINT('Ctrl Pts',(-6.07769535203109,-0.680040386815467,
5.64577456629615));
#8553=CARTESIAN_POINT('Ctrl Pts',(-6.0563805151783,-0.849165361413687,5.6535330083093));
#8554=CARTESIAN_POINT('Ctrl Pts',(-6.02804736704293,-1.01708923069061,5.66129145032245));
#8555=CARTESIAN_POINT('Ctrl Pts',(-5.999707103126,-1.1850552735222,5.66905184084405));
#8556=CARTESIAN_POINT('Ctrl Pts',(-5.96434505832789,-1.35181930182925,5.67681223136565));
#8557=CARTESIAN_POINT('Ctrl Pts',(-5.9220911369778,-1.5167933701823,5.68457262188726));
#8558=CARTESIAN_POINT('Ctrl Pts',(-5.90003795229844,-1.60289670640407,5.68862292822306));
#8559=CARTESIAN_POINT('Ctrl Pts',(-5.87610825654539,-1.68851263893871,5.69267323455887));
#8560=CARTESIAN_POINT('Ctrl Pts',(-5.85032597278372,-1.77355901358603,5.69672354089467));
#8561=CARTESIAN_POINT('Ctrl Pts',(-5.80115388750823,-1.93575983431962,5.70444830299787));
#8562=CARTESIAN_POINT('Ctrl Pts',(-5.74522338914962,-2.09594316694078,5.71217306510106));
#8563=CARTESIAN_POINT('Ctrl Pts',(-5.68272521061636,-2.25354381877194,5.71989782720426));
#8564=CARTESIAN_POINT('Ctrl Pts',(-5.62023922352594,-2.41111372763774,5.72762108244762));
#8565=CARTESIAN_POINT('Ctrl Pts',(-5.55118822937105,-2.56610166654768,5.73534433769097));
#8566=CARTESIAN_POINT('Ctrl Pts',(-5.47581157962943,-2.71796120408226,5.74306759293432));
#8567=CARTESIAN_POINT('Ctrl Pts',(-5.40043201694254,-2.86982661025815,5.75079114664437));
#8568=CARTESIAN_POINT('Ctrl Pts',(-5.3187264468512,-3.01856308750147,5.75851470035443));
#8569=CARTESIAN_POINT('Ctrl Pts',(-5.23098112786476,-3.1636469465512,5.76623825406448));
#8570=CARTESIAN_POINT('Ctrl Pts',(-5.14324170225228,-3.30872106111031,5.7739612890256));
#8571=CARTESIAN_POINT('Ctrl Pts',(-5.04946350356382,-3.45014277720372,5.78168432398672));
#8572=CARTESIAN_POINT('Ctrl Pts',(-4.94997733988254,-3.5874154898965,5.78940735894785));
#8573=CARTESIAN_POINT('Ctrl Pts',(-4.85046473711304,-3.72472468369606,5.79713244635521));
#8574=CARTESIAN_POINT('Ctrl Pts',(-4.74524132250649,-3.8578824127043,5.80485753376257));
#8575=CARTESIAN_POINT('Ctrl Pts',(-4.63468016246876,-3.98642262612967,5.81258262116993));
#8576=CARTESIAN_POINT('Ctrl Pts',(-4.52454772150958,-4.11446440374052,5.82027775328057));
#8577=CARTESIAN_POINT('Ctrl Pts',(-4.40911908552082,-4.23792419680251,5.82797288539121));
#8578=CARTESIAN_POINT('Ctrl Pts',(-4.28880145867236,-4.35637551303717,5.83566801750185));
#8579=CARTESIAN_POINT('Ctrl Pts',(-4.16802055057835,-4.47528292431591,5.84339277960505));
#8580=CARTESIAN_POINT('Ctrl Pts',(-4.04227012884317,-4.58918530414057,5.85111754170825));
#8581=CARTESIAN_POINT('Ctrl Pts',(-3.91198808571947,-4.69767759426814,5.85884230381145));
#8582=CARTESIAN_POINT('Ctrl Pts',(-3.78173145655423,-4.80614872093766,5.86656555905478));
#8583=CARTESIAN_POINT('Ctrl Pts',(-3.64694521324448,-4.90921166100622,5.87428881429811));
#8584=CARTESIAN_POINT('Ctrl Pts',(-3.50810096534317,-5.00650109152673,5.88201206954143));
#8585=CARTESIAN_POINT('Ctrl Pts',(-3.3692513517786,-5.1037942818164,5.88973562325148));
#8586=CARTESIAN_POINT('Ctrl Pts',(-3.22634367708091,-5.19531333097637,5.89745917696152));
#8587=CARTESIAN_POINT('Ctrl Pts',(-3.07987986057829,-5.28073532823832,5.90518273067156));
#8588=CARTESIAN_POINT('Ctrl Pts',(-2.93342588125007,-5.36615158817138,5.9129057656327));
#8589=CARTESIAN_POINT('Ctrl Pts',(-2.7834165118849,-5.4454714560156,5.92062880059383));
#8590=CARTESIAN_POINT('Ctrl Pts',(-2.63037983402097,-5.51841711827548,5.92835183555497));
#8591=CARTESIAN_POINT('Ctrl Pts',(-2.47730248567556,-5.59138216631429,5.93607692296232));
#8592=CARTESIAN_POINT('Ctrl Pts',(-2.32119650654447,-5.65796948534384,5.94380201036967));
#8593=CARTESIAN_POINT('Ctrl Pts',(-2.16261246830647,-5.71794830987701,5.95152709777702));
#8594=CARTESIAN_POINT('Ctrl Pts',(-2.00464336575315,-5.77769455665558,5.95922222988769));
#8595=CARTESIAN_POINT('Ctrl Pts',(-1.8442156914994,-5.83088338859352,5.96691736199837));
#8596=CARTESIAN_POINT('Ctrl Pts',(-1.68189106853615,-5.87733511007143,5.97461249410904));
#8597=CARTESIAN_POINT('Ctrl Pts',(-1.51894141700973,-5.92396569321679,5.98233725621225));
#8598=CARTESIAN_POINT('Ctrl Pts',(-1.35402245925002,-5.96382366692076,5.99006201831545));
#8599=CARTESIAN_POINT('Ctrl Pts',(-1.18771251158513,-5.9967628394263,5.99778678041866));
#8600=CARTESIAN_POINT('Ctrl Pts',(-1.02143500579854,-6.0296955865277,6.00551003566196));
#8601=CARTESIAN_POINT('Ctrl Pts',(-0.853767362223276,-6.05571216391337,
6.01323329090526));
#8602=CARTESIAN_POINT('Ctrl Pts',(-0.685298494701385,-6.0747174037695,6.02095654614857));
#8603=CARTESIAN_POINT('Ctrl Pts',(-0.516823116666214,-6.09372337808694,
6.02868009985862));
#8604=CARTESIAN_POINT('Ctrl Pts',(-0.347546767200922,-6.10571743321528,
6.03640365356867));
#8605=CARTESIAN_POINT('Ctrl Pts',(-0.178064684725665,-6.11065614566501,
6.04412720727873));
#8606=CARTESIAN_POINT('Ctrl Pts',(-0.00859398543617382,-6.1155945264084,
6.05185024223987));
#8607=CARTESIAN_POINT('Ctrl Pts',(0.161082102388196,-6.11347850353662,6.059573277201));
#8608=CARTESIAN_POINT('Ctrl Pts',(0.330366942461903,-6.10431677141909,6.06729631216214));
#8609=CARTESIAN_POINT('Ctrl Pts',(0.499696771071035,-6.0951526045123,6.07502139956951));
#8610=CARTESIAN_POINT('Ctrl Pts',(0.66863482735465,-6.07893900172759,6.08274648697688));
#8611=CARTESIAN_POINT('Ctrl Pts',(0.836587234990848,-6.05573673145971,6.09047157438425));
#8612=CARTESIAN_POINT('Ctrl Pts',(1.00388837954898,-6.0326244318101,6.09816670649491));
#8613=CARTESIAN_POINT('Ctrl Pts',(1.17021120106051,-6.00257764240171,6.10586183860557));
#8614=CARTESIAN_POINT('Ctrl Pts',(1.33497655207619,-5.96570726468428,6.11355697071623));
#8615=CARTESIAN_POINT('Ctrl Pts',(1.50037510143476,-5.92869519296426,6.12128167545773));
#8616=CARTESIAN_POINT('Ctrl Pts',(1.66426275803222,-5.88479384477632,6.12900638019924));
#8617=CARTESIAN_POINT('Ctrl Pts',(1.82606175761478,-5.8341515252757,6.13673108494074));
#8618=CARTESIAN_POINT('Ctrl Pts',(1.98782868547295,-5.78351924407271,6.14445425849477));
#8619=CARTESIAN_POINT('Ctrl Pts',(2.14750748019648,-5.72614875246145,6.15217743204879));
#8620=CARTESIAN_POINT('Ctrl Pts',(2.30453548773657,-5.66223822779144,6.15990060560282));
#8621=CARTESIAN_POINT('Ctrl Pts',(2.46155959184305,-5.59832929182204,6.16762358717266));
#8622=CARTESIAN_POINT('Ctrl Pts',(2.61593274570186,-5.52788076395922,6.1753465687425));
#8623=CARTESIAN_POINT('Ctrl Pts',(2.76711159942012,-5.45113923495397,6.18306955031233));
#8624=CARTESIAN_POINT('Ctrl Pts',(2.91828130145515,-5.37440235153339,6.19079206436783));
#8625=CARTESIAN_POINT('Ctrl Pts',(3.06625680778526,-5.29137337273966,6.19851457842334));
#8626=CARTESIAN_POINT('Ctrl Pts',(3.21051845807112,-5.2023453165745,6.20623709247884));
#8627=CARTESIAN_POINT('Ctrl Pts',(3.35479862779034,-5.1133058315289,6.21396059790373));
#8628=CARTESIAN_POINT('Ctrl Pts',(3.49536371969221,-5.01826589756368,6.22168410332863));
#8629=CARTESIAN_POINT('Ctrl Pts',(3.63172160349,-4.91756278630421,6.22940760875352));
#8630=CARTESIAN_POINT('Ctrl Pts',(3.66233632378909,-4.89495318355452,6.2311416702667));
#8631=CARTESIAN_POINT('Ctrl Pts',(3.69273908654001,-4.8720582810407,6.23287573177987));
#8632=CARTESIAN_POINT('Ctrl Pts',(3.72292453512037,-4.84888218750454,6.23460979329304));
#8633=CARTESIAN_POINT('Ctrl Pts',(3.72292453512037,-4.84888218750453,4.4846183003358));
#8634=CARTESIAN_POINT('Ctrl Pts',(3.85738003164868,-4.74564856632129,4.49234091472402));
#8635=CARTESIAN_POINT('Ctrl Pts',(3.98754958283495,-4.63681087233664,4.50006352911223));
#8636=CARTESIAN_POINT('Ctrl Pts',(4.11297418411632,-4.52275015043863,4.50778614350044));
#8637=CARTESIAN_POINT('Ctrl Pts',(4.23840733119494,-4.40868165702058,4.5155092840685));
#8638=CARTESIAN_POINT('Ctrl Pts',(4.35909464600389,-4.28938963570915,4.52323242463655));
#8639=CARTESIAN_POINT('Ctrl Pts',(4.47461199751822,-4.1652938712852,4.53095556520461));
#8640=CARTESIAN_POINT('Ctrl Pts',(4.59012790250441,-4.04119966080974,4.53867860906217));
#8641=CARTESIAN_POINT('Ctrl Pts',(4.70047375972252,-3.91230206130686,4.54640165291973));
#8642=CARTESIAN_POINT('Ctrl Pts',(4.80526379357084,-3.77905615685943,4.55412469677729));
#8643=CARTESIAN_POINT('Ctrl Pts',(4.91007646117892,-3.6457814724252,4.56184940874691));
#8644=CARTESIAN_POINT('Ctrl Pts',(5.00933071284341,-3.50815685642527,4.56957412071653));
#8645=CARTESIAN_POINT('Ctrl Pts',(5.10268193066479,-3.36666937446596,4.57729883268615));
#8646=CARTESIAN_POINT('Ctrl Pts',(5.13437981000813,-3.31862658256237,4.57992179780316));
#8647=CARTESIAN_POINT('Ctrl Pts',(5.16539744813244,-3.27013866339535,4.58254476292016));
#8648=CARTESIAN_POINT('Ctrl Pts',(5.19572249657802,-3.22122543468368,4.58516772803716));
#8649=CARTESIAN_POINT('Ctrl Pts',(5.28503126530388,-3.0771735549815,4.59289249014036));
#8650=CARTESIAN_POINT('Ctrl Pts',(5.36836138009955,-2.92937973689538,4.60061725224357));
#8651=CARTESIAN_POINT('Ctrl Pts',(5.44541445031272,-2.77836049259728,4.60834201434678));
#8652=CARTESIAN_POINT('Ctrl Pts',(5.52245248987796,-2.627370707438,4.61606526959011));
#8653=CARTESIAN_POINT('Ctrl Pts',(5.59321578413792,-2.47315703363873,4.62378852483345));
#8654=CARTESIAN_POINT('Ctrl Pts',(5.65745214105643,-2.31626009639591,4.63151178007678));
#8655=CARTESIAN_POINT('Ctrl Pts',(5.72169098040162,-2.15935709584001,4.63923533378684));
#8656=CARTESIAN_POINT('Ctrl Pts',(5.77940225392466,-1.99977091612798,4.64695888749689));
#8657=CARTESIAN_POINT('Ctrl Pts',(5.83038182676192,-1.838062381059,4.65468244120695));
#8658=CARTESIAN_POINT('Ctrl Pts',(5.88135797557967,-1.67636470706926,4.66240547616808));
#8659=CARTESIAN_POINT('Ctrl Pts',(5.92560323320806,-1.51254526527581,4.67012851112921));
#8660=CARTESIAN_POINT('Ctrl Pts',(5.96296322514271,-1.34718044006572,4.67785154609034));
#8661=CARTESIAN_POINT('Ctrl Pts',(6.00033314573561,-1.18177166808926,4.68557663349771));
#8662=CARTESIAN_POINT('Ctrl Pts',(6.0308140722262,-1.0148170008996,4.69330172090507));
#8663=CARTESIAN_POINT('Ctrl Pts',(6.05430248239203,-0.846904371344088,4.70102680831244));
#8664=CARTESIAN_POINT('Ctrl Pts',(6.07769981238503,-0.679642850621103,4.70872194042308));
#8665=CARTESIAN_POINT('Ctrl Pts',(6.09415874759425,-0.511431097283521,4.71641707253371));
#8666=CARTESIAN_POINT('Ctrl Pts',(6.10362801536036,-0.342856548148325,4.72411220464435));
#8667=CARTESIAN_POINT('Ctrl Pts',(6.11313374440217,-0.173632905200967,4.73183696674755));
#8668=CARTESIAN_POINT('Ctrl Pts',(6.11559920859452,-0.00398373136690208,
4.73956172885075));
#8669=CARTESIAN_POINT('Ctrl Pts',(6.1110094978451,0.165494651717244,4.74728649095394));
#8670=CARTESIAN_POINT('Ctrl Pts',(6.10642068240492,0.334939974861039,4.75500974619727));
#8671=CARTESIAN_POINT('Ctrl Pts',(6.09477944669772,0.504214257114271,4.7627330014406));
#8672=CARTESIAN_POINT('Ctrl Pts',(6.07612298521814,0.672722105333136,4.77045625668393));
#8673=CARTESIAN_POINT('Ctrl Pts',(6.05746580275592,0.841236465570973,4.77817981039397));
#8674=CARTESIAN_POINT('Ctrl Pts',(6.03179288296159,1.0089840170759,4.78590336410402));
#8675=CARTESIAN_POINT('Ctrl Pts',(5.99919328418982,1.17537462174058,4.79362691781407));
#8676=CARTESIAN_POINT('Ctrl Pts',(5.96659587495507,1.34175405085698,4.80134995277519));
#8677=CARTESIAN_POINT('Ctrl Pts',(5.92707277868547,1.50677640447407,4.80907298773631));
#8678=CARTESIAN_POINT('Ctrl Pts',(5.88076419424647,1.6698616871372,4.81679602269744));
#8679=CARTESIAN_POINT('Ctrl Pts',(5.83444330300318,1.83299031076359,4.82452111010479));
#8680=CARTESIAN_POINT('Ctrl Pts',(5.78133340471915,1.99418052907824,4.83224619751215));
#8681=CARTESIAN_POINT('Ctrl Pts',(5.72162487809727,2.15286653484102,4.83997128491951));
#8682=CARTESIAN_POINT('Ctrl Pts',(5.6621478811054,2.31093720952329,4.84766641703019));
#8683=CARTESIAN_POINT('Ctrl Pts',(5.59612347945264,2.46652277728533,4.85536154914087));
#8684=CARTESIAN_POINT('Ctrl Pts',(5.52378769623179,2.61908286418325,4.86305668125155));
#8685=CARTESIAN_POINT('Ctrl Pts',(5.45117338514619,2.77223038144213,4.87078144335474));
#8686=CARTESIAN_POINT('Ctrl Pts',(5.37217324728784,2.92238329987741,4.87850620545794));
#8687=CARTESIAN_POINT('Ctrl Pts',(5.28705948742644,3.06901084046866,4.88623096756114));
#8688=CARTESIAN_POINT('Ctrl Pts',(5.20196233060183,3.2156097786053,4.89395422280446));
#8689=CARTESIAN_POINT('Ctrl Pts',(5.11075409040059,3.35868443715986,4.90167747804779));
#8690=CARTESIAN_POINT('Ctrl Pts',(5.01375228177231,3.49772978080397,4.90940073329111));
#8691=CARTESIAN_POINT('Ctrl Pts',(4.91674672448998,3.63678049788283,4.91712428700116));
#8692=CARTESIAN_POINT('Ctrl Pts',(4.81394732883338,3.77180132627353,4.92484784071121));
#8693=CARTESIAN_POINT('Ctrl Pts',(4.70571463859838,3.90231665841983,4.93257139442125));
#8694=CARTESIAN_POINT('Ctrl Pts',(4.59748921776214,4.032823224564,4.94029442938237));
#8695=CARTESIAN_POINT('Ctrl Pts',(4.48383143495245,4.15882465605924,4.9480174643435));
#8696=CARTESIAN_POINT('Ctrl Pts',(4.36514188924104,4.27987871899346,4.95574049930462));
#8697=CARTESIAN_POINT('Ctrl Pts',(4.24642080101916,4.40096495282382,4.96346558671198));
#8698=CARTESIAN_POINT('Ctrl Pts',(4.12266549827857,4.5171009628278,4.97119067411934));
#8699=CARTESIAN_POINT('Ctrl Pts',(3.99431385625943,4.62788098163662,4.97891576152669));
#8700=CARTESIAN_POINT('Ctrl Pts',(3.86645991883735,4.73823143270672,4.98661089363738));
#8701=CARTESIAN_POINT('Ctrl Pts',(3.73404548229173,4.8432671766407,4.99430602574806));
#8702=CARTESIAN_POINT('Ctrl Pts',(3.5975363353603,4.94262661732225,5.00200115785874));
#8703=CARTESIAN_POINT('Ctrl Pts',(3.46050156197515,5.04236864006238,5.00972591996194));
#8704=CARTESIAN_POINT('Ctrl Pts',(3.31929193105522,5.13642586111289,5.01745068206514));
#8705=CARTESIAN_POINT('Ctrl Pts',(3.17440041292128,5.22446242028261,5.02517544416834));
#8706=CARTESIAN_POINT('Ctrl Pts',(3.02953715859822,5.31248180626861,5.03289869941166));
#8707=CARTESIAN_POINT('Ctrl Pts',(2.88099372085466,5.39448270933945,5.04062195465499));
#8708=CARTESIAN_POINT('Ctrl Pts',(2.72929054152797,5.47017355322717,5.04834520989831));
#8709=CARTESIAN_POINT('Ctrl Pts',(2.57758149960195,5.5458673222025,5.05606876360836));
#8710=CARTESIAN_POINT('Ctrl Pts',(2.42271275355714,5.6152503989949,5.06379231731841));
#8711=CARTESIAN_POINT('Ctrl Pts',(2.26522845087726,5.67807763488984,5.07151587102845));
#8712=CARTESIAN_POINT('Ctrl Pts',(2.10775472555801,5.74090065102243,5.07923890598958));
#8713=CARTESIAN_POINT('Ctrl Pts',(1.9476660895506,5.79716858996948,5.0869619409507));
#8714=CARTESIAN_POINT('Ctrl Pts',(1.78552589699476,5.84668477290003,5.09468497591182));
#8715=CARTESIAN_POINT('Ctrl Pts',(1.62334261463946,5.8962141150748,5.10241006331918));
#8716=CARTESIAN_POINT('Ctrl Pts',(1.4591069889493,5.93898802102476,5.11013515072653));
#8717=CARTESIAN_POINT('Ctrl Pts',(1.29339766057976,5.97485966815178,5.11786023813389));
#8718=CARTESIAN_POINT('Ctrl Pts',(1.1283308973791,6.01059221706857,5.12555537024456));
#8719=CARTESIAN_POINT('Ctrl Pts',(0.961802152173548,6.03947590675075,5.13325050235524));
#8720=CARTESIAN_POINT('Ctrl Pts',(0.794393444370498,6.06141605716364,5.14094563446591));
#8721=CARTESIAN_POINT('Ctrl Pts',(0.62634013181097,6.0834406878016,5.1486703965691));
#8722=CARTESIAN_POINT('Ctrl Pts',(0.457340543251073,6.09847597173067,5.1563951586723));
#8723=CARTESIAN_POINT('Ctrl Pts',(0.287988254136562,6.1064628327682,5.16411992077549));
#8724=CARTESIAN_POINT('Ctrl Pts',(0.118669000365456,6.11444813581853,5.17184317601882));
#8725=CARTESIAN_POINT('Ctrl Pts',(-0.0510025002955841,6.11538774452854,
5.17956643126214));
#8726=CARTESIAN_POINT('Ctrl Pts',(-0.220429735668919,6.10927461276156,5.18728968650546));
#8727=CARTESIAN_POINT('Ctrl Pts',(-0.389863518591201,6.1031612447514,5.19501324021551));
#8728=CARTESIAN_POINT('Ctrl Pts',(-0.559052700481732,6.08999459833462,5.20273679392555));
#8729=CARTESIAN_POINT('Ctrl Pts',(-0.727402164915347,6.06981973809573,5.2104603476356));
#8730=CARTESIAN_POINT('Ctrl Pts',(-0.895740322234849,6.04964623289201,5.21818338259672));
#8731=CARTESIAN_POINT('Ctrl Pts',(-1.0632385602567,6.02246549354144,5.22590641755784));
#8732=CARTESIAN_POINT('Ctrl Pts',(-1.22930808609958,5.98837433632452,5.23362945251897));
#8733=CARTESIAN_POINT('Ctrl Pts',(-1.39542174598742,5.95427411916324,5.24135453992632));
#8734=CARTESIAN_POINT('Ctrl Pts',(-1.5601056238747,5.913259876027,5.24907962733367));
#8735=CARTESIAN_POINT('Ctrl Pts',(-1.7227813560714,5.86547951677208,5.25680471474103));
#8736=CARTESIAN_POINT('Ctrl Pts',(-1.88482628636772,5.8178844337167,5.26449984685172));
#8737=CARTESIAN_POINT('Ctrl Pts',(-2.04487832666801,5.76357573362856,5.27219497896241));
#8738=CARTESIAN_POINT('Ctrl Pts',(-2.20238109283932,5.70274873060386,5.27989011107311));
#8739=CARTESIAN_POINT('Ctrl Pts',(-2.36049032108483,5.64168751410266,5.28761487317631));
#8740=CARTESIAN_POINT('Ctrl Pts',(-2.51608659111276,5.57403604368506,5.2953396352795));
#8741=CARTESIAN_POINT('Ctrl Pts',(-2.6686204050553,5.50002642686583,5.3030643973827));
#8742=CARTESIAN_POINT('Ctrl Pts',(-2.82112446441408,5.42603124701166,5.31078765262604));
#8743=CARTESIAN_POINT('Ctrl Pts',(-2.97056697473137,5.34568053381436,5.31851090786939));
#8744=CARTESIAN_POINT('Ctrl Pts',(-3.11642075201407,5.25925348874877,5.32623416311273));
#8745=CARTESIAN_POINT('Ctrl Pts',(-3.26228016584448,5.17282310369314,5.33395771682278));
#8746=CARTESIAN_POINT('Ctrl Pts',(-3.40455029445344,5.08031607502897,5.34168127053282));
#8747=CARTESIAN_POINT('Ctrl Pts',(-3.5427301107876,4.98205669624693,5.34940482424287));
#8748=CARTESIAN_POINT('Ctrl Pts',(-3.6809006463382,4.88380391701069,5.357127859204));
#8749=CARTESIAN_POINT('Ctrl Pts',(-3.81498116107768,4.77979974450149,5.36485089416514));
#8750=CARTESIAN_POINT('Ctrl Pts',(-3.9445009403465,4.67041089135695,5.37257392912627));
#8751=CARTESIAN_POINT('Ctrl Pts',(-4.07405514033001,4.56099296742085,5.38029901653363));
#8752=CARTESIAN_POINT('Ctrl Pts',(-4.19904593917991,4.44618770630897,5.38802410394099));
#8753=CARTESIAN_POINT('Ctrl Pts',(-4.31903622504276,4.32640169763146,5.39574919134835));
#8754=CARTESIAN_POINT('Ctrl Pts',(-4.43856122884126,4.20708017889992,5.403444323459));
#8755=CARTESIAN_POINT('Ctrl Pts',(-4.55312423317451,4.08281671465023,5.41113945556965));
#8756=CARTESIAN_POINT('Ctrl Pts',(-4.66233010658665,3.95404900573017,5.41883458768029));
#8757=CARTESIAN_POINT('Ctrl Pts',(-4.77195647560163,3.82478547864853,5.42655934978349));
#8758=CARTESIAN_POINT('Ctrl Pts',(-4.87622318019224,3.69093715026868,5.43428411188669));
#8759=CARTESIAN_POINT('Ctrl Pts',(-4.97475873895932,3.55297073610914,5.44200887398989));
#8760=CARTESIAN_POINT('Ctrl Pts',(-5.07327507651592,3.41503123488863,5.44973212923323));
#8761=CARTESIAN_POINT('Ctrl Pts',(-5.16606231491152,3.27297550852698,5.45745538447657));
#8762=CARTESIAN_POINT('Ctrl Pts',(-5.25279109827068,3.12730095136819,5.46517863971991));
#8763=CARTESIAN_POINT('Ctrl Pts',(-5.33952323328064,2.98162076458762,5.47290219342995));
#8764=CARTESIAN_POINT('Ctrl Pts',(-5.42019627921881,2.83232173744498,5.48062574714));
#8765=CARTESIAN_POINT('Ctrl Pts',(-5.49452542264047,2.67992834651555,5.48834930085005));
#8766=CARTESIAN_POINT('Ctrl Pts',(-5.56884957377953,2.52754519101786,5.49607233581118));
#8767=CARTESIAN_POINT('Ctrl Pts',(-5.63683053612654,2.37206837251912,5.50379537077231));
#8768=CARTESIAN_POINT('Ctrl Pts',(-5.69823040890161,2.21404511461916,5.51151840573344));
#8769=CARTESIAN_POINT('Ctrl Pts',(-5.75964659908791,2.05597986102173,5.5192434931408));
#8770=CARTESIAN_POINT('Ctrl Pts',(-5.8144780879474,1.89536711057669,5.52696858054816));
#8771=CARTESIAN_POINT('Ctrl Pts',(-5.86253556051135,1.73277302732927,5.53469366795552));
#8772=CARTESIAN_POINT('Ctrl Pts',(-5.91040668232307,1.57080942937591,5.54238880006617));
#8773=CARTESIAN_POINT('Ctrl Pts',(-5.95155617160243,1.40688014571579,5.55008393217683));
#8774=CARTESIAN_POINT('Ctrl Pts',(-5.98584646198968,1.24155857533411,5.55777906428748));
#8775=CARTESIAN_POINT('Ctrl Pts',(-6.02107100601623,1.07173274800266,5.56568385356634));
#8776=CARTESIAN_POINT('Ctrl Pts',(-6.04906762166612,0.900389754905527,5.5735886428452));
#8777=CARTESIAN_POINT('Ctrl Pts',(-6.06973067897709,0.728144935561822,5.58149343212406));
#8778=CARTESIAN_POINT('Ctrl Pts',(-6.0903879230381,0.555948574787141,5.58939599750569));
#8779=CARTESIAN_POINT('Ctrl Pts',(-6.10371569436386,0.382851176372991,5.59729856288731));
#8780=CARTESIAN_POINT('Ctrl Pts',(-6.1096600488996,0.20947469866338,5.60520112826894));
#8781=CARTESIAN_POINT('Ctrl Pts',(-6.11205203894302,0.139708535499509,5.60838109635406));
#8782=CARTESIAN_POINT('Ctrl Pts',(-6.11324906863418,0.0698972401555901,
5.61156106443918));
#8783=CARTESIAN_POINT('Ctrl Pts',(-6.11324999945666,8.15052733772887E-5,
5.61474103252431));
#8784=CARTESIAN_POINT('Origin',(0.,0.,-3.86474103256053));
#8785=CARTESIAN_POINT('',(3.72292453512037,-4.84888218750454,2.73461001778677));
#8786=CARTESIAN_POINT('',(3.72292453512038,-4.84888218750453,2.88012709193022));
#8787=CARTESIAN_POINT('',(3.72292453512038,-4.84888218750453,-3.86474103256053));
#8788=CARTESIAN_POINT('',(-6.11324999945432,-8.16805581249634E-5,4.01025896739721));
#8789=CARTESIAN_POINT('Ctrl Pts',(3.72292453512039,-4.84888218750453,2.88012709193022));
#8790=CARTESIAN_POINT('Ctrl Pts',(3.85740722513931,-4.74562768742394,2.88785179219662));
#8791=CARTESIAN_POINT('Ctrl Pts',(3.98757783499191,-4.63678558761364,2.89557649246302));
#8792=CARTESIAN_POINT('Ctrl Pts',(4.1129822323414,-4.52274283139601,2.90330119272942));
#8793=CARTESIAN_POINT('Ctrl Pts',(4.1483088696491,-4.49061678819799,2.90547725425828));
#8794=CARTESIAN_POINT('Ctrl Pts',(4.18325748915386,-4.45807828123202,2.90765331578713));
#8795=CARTESIAN_POINT('Ctrl Pts',(4.21781844241679,-4.42513651194049,2.90982937731599));
#8796=CARTESIAN_POINT('Ctrl Pts',(4.34050575545397,-4.30819711127285,2.91755413941812));
#8797=CARTESIAN_POINT('Ctrl Pts',(4.45834856405392,-4.18613158317652,2.92527890152026));
#8798=CARTESIAN_POINT('Ctrl Pts',(4.57092809274141,-4.05936472043192,2.93300366362239));
#8799=CARTESIAN_POINT('Ctrl Pts',(4.68348566067742,-3.93262258594478,2.94072691886459));
#8800=CARTESIAN_POINT('Ctrl Pts',(4.79078178701837,-3.80118118354429,2.9484501741068));
#8801=CARTESIAN_POINT('Ctrl Pts',(4.89243633951613,-3.66550026957877,2.956173429349));
#8802=CARTESIAN_POINT('Ctrl Pts',(4.9940948204743,-3.52981411219733,2.96389698305794));
#8803=CARTESIAN_POINT('Ctrl Pts',(5.09011109812451,-3.38988836665788,2.97162053676688));
#8804=CARTESIAN_POINT('Ctrl Pts',(5.18014646731156,-3.24621443218091,2.97934409047582));
#8805=CARTESIAN_POINT('Ctrl Pts',(5.27017578931429,-3.1025501474979,2.98706712543581));
#8806=CARTESIAN_POINT('Ctrl Pts',(5.3542248384284,-2.9551384462428,2.9947901603958));
#8807=CARTESIAN_POINT('Ctrl Pts',(5.4319991521926,-2.80449831040757,3.0025131953558));
#8808=CARTESIAN_POINT('Ctrl Pts',(5.50979413498119,-2.6538181409868,3.01023828276203));
#8809=CARTESIAN_POINT('Ctrl Pts',(5.58131090281586,-2.4999081033464,3.01796337016827));
#8810=CARTESIAN_POINT('Ctrl Pts',(5.64630130242559,-2.34331115405682,3.0256884575745));
#8811=CARTESIAN_POINT('Ctrl Pts',(5.71103969113038,-2.18732143505259,3.03338358969073));
#8812=CARTESIAN_POINT('Ctrl Pts',(5.76930214586503,-2.02866590593596,3.04107872180696));
#8813=CARTESIAN_POINT('Ctrl Pts',(5.82089120605154,-1.86790019267943,3.04877385392319));
#8814=CARTESIAN_POINT('Ctrl Pts',(5.87267890912134,-1.7065154535151,3.05649861602735));
#8815=CARTESIAN_POINT('Ctrl Pts',(5.91776003709367,-1.54294708064208,3.06422337813152));
#8816=CARTESIAN_POINT('Ctrl Pts',(5.95597008558128,-1.37776845012541,3.07194814023568));
#8817=CARTESIAN_POINT('Ctrl Pts',(5.9941726804816,-1.21262204080153,3.07967139547997));
#8818=CARTESIAN_POINT('Ctrl Pts',(6.02550679895802,-1.04586630918302,3.08739465072427));
#8819=CARTESIAN_POINT('Ctrl Pts',(6.04985859784319,-0.878086845706551,3.09511790596856));
#8820=CARTESIAN_POINT('Ctrl Pts',(6.07421133780852,-0.710300898359008,3.10284145967961));
#8821=CARTESIAN_POINT('Ctrl Pts',(6.0915811687888,-0.541491453049558,3.11056501339066));
#8822=CARTESIAN_POINT('Ctrl Pts',(6.10190576470393,-0.372252066714117,3.1182885671017));
#8823=CARTESIAN_POINT('Ctrl Pts',(6.1122296671723,-0.203024047264704,3.1260116020638));
#8824=CARTESIAN_POINT('Ctrl Pts',(6.11550926221234,-0.0333664609460739,
3.13373463702589));
#8825=CARTESIAN_POINT('Ctrl Pts',(6.11173427081301,0.136124081152851,3.14145767198798));
#8826=CARTESIAN_POINT('Ctrl Pts',(6.10795827618541,0.30565966645452,3.14918275939633));
#8827=CARTESIAN_POINT('Ctrl Pts',(6.09712395369223,0.475027801708435,3.15690784680469));
#8828=CARTESIAN_POINT('Ctrl Pts',(6.07927315977078,0.643632978793483,3.16463293421304));
#8829=CARTESIAN_POINT('Ctrl Pts',(6.06149158525163,0.811584361451595,3.17232806631882));
#8830=CARTESIAN_POINT('Ctrl Pts',(6.03674792255507,0.978778385355505,3.1800231984246));
#8831=CARTESIAN_POINT('Ctrl Pts',(6.00513460410749,1.14463266992115,3.18771833053038));
#8832=CARTESIAN_POINT('Ctrl Pts',(5.9733995590264,1.31112557405299,3.195443092633));
#8833=CARTESIAN_POINT('Ctrl Pts',(5.93473058105001,1.4763273622822,3.20316785473561));
#8834=CARTESIAN_POINT('Ctrl Pts',(5.88925753445974,1.63965583440829,3.21089261683823));
#8835=CARTESIAN_POINT('Ctrl Pts',(5.84379335824084,1.80295244624988,3.21861587208099));
#8836=CARTESIAN_POINT('Ctrl Pts',(5.79152784672204,1.96437616601436,3.22633912732375));
#8837=CARTESIAN_POINT('Ctrl Pts',(5.73264119483716,2.12335830555183,3.2340623825665));
#8838=CARTESIAN_POINT('Ctrl Pts',(5.67375226726619,2.28234658898495,3.24178593627596));
#8839=CARTESIAN_POINT('Ctrl Pts',(5.60824179366985,2.43889280481764,3.24950948998542));
#8840=CARTESIAN_POINT('Ctrl Pts',(5.53633901888734,2.59244591659026,3.25723304369488));
#8841=CARTESIAN_POINT('Ctrl Pts',(5.46444107342178,2.74598871503844,3.26495607865539));
#8842=CARTESIAN_POINT('Ctrl Pts',(5.38615182035971,2.89653852467828,3.27267911361589));
#8843=CARTESIAN_POINT('Ctrl Pts',(5.30174766962646,3.04356652795867,3.2804021485764));
#8844=CARTESIAN_POINT('Ctrl Pts',(5.21732108794688,3.1906336048773,3.28812723598316));
#8845=CARTESIAN_POINT('Ctrl Pts',(5.12677651731211,3.33417672906057,3.29585232338992));
#8846=CARTESIAN_POINT('Ctrl Pts',(5.03043562145371,3.47369299462541,3.30357741079668));
#8847=CARTESIAN_POINT('Ctrl Pts',(4.9344683032164,3.61266826299348,3.31127254291031));
#8848=CARTESIAN_POINT('Ctrl Pts',(4.83274973616982,3.74764760826321,3.31896767502394));
#8849=CARTESIAN_POINT('Ctrl Pts',(4.72563971554549,3.87816384921513,3.32666280713756));
#8850=CARTESIAN_POINT('Ctrl Pts',(4.61811726940627,4.00918264097942,3.33438756924104));
#8851=CARTESIAN_POINT('Ctrl Pts',(4.50512366338708,4.13575027387649,3.34211233134452));
#8852=CARTESIAN_POINT('Ctrl Pts',(4.38705147630667,4.25741763358206,3.349837093448));
#8853=CARTESIAN_POINT('Ctrl Pts',(4.2690023214234,4.37906125978456,3.35756034869158));
#8854=CARTESIAN_POINT('Ctrl Pts',(4.14587678280687,4.49580629284127,3.36528360393516));
#8855=CARTESIAN_POINT('Ctrl Pts',(4.01810517137538,4.60723956336834,3.37300685917875));
#8856=CARTESIAN_POINT('Ctrl Pts',(3.89032862218446,4.71867714025639,3.38073041288907));
#8857=CARTESIAN_POINT('Ctrl Pts',(3.75790587713221,4.82480233256016,3.38845396659939));
#8858=CARTESIAN_POINT('Ctrl Pts',(3.62130187405447,4.92524093821506,3.39617752030971));
#8859=CARTESIAN_POINT('Ctrl Pts',(3.48470704592134,5.02567279795752,3.40390055527113));
#8860=CARTESIAN_POINT('Ctrl Pts',(3.34393177711988,5.12041864761897,3.41162359023254));
#8861=CARTESIAN_POINT('Ctrl Pts',(3.19947179220364,5.20914636129503,3.41934662519396));
#8862=CARTESIAN_POINT('Ctrl Pts',(3.05497341611712,5.29789765493177,3.42707171260159));
#8863=CARTESIAN_POINT('Ctrl Pts',(2.90678863626768,5.38062744883377,3.43479680000923));
#8864=CARTESIAN_POINT('Ctrl Pts',(2.75544051885762,5.45704802155319,3.44252188741687));
#8865=CARTESIAN_POINT('Ctrl Pts',(2.60467927869192,5.53317226091944,3.45021701952616));
#8866=CARTESIAN_POINT('Ctrl Pts',(2.45077948328852,5.60303601027428,3.45791215163546));
#8867=CARTESIAN_POINT('Ctrl Pts',(2.2942805913903,5.66640116215484,3.46560728374476));
#8868=CARTESIAN_POINT('Ctrl Pts',(2.13717910279434,5.73001030062734,3.47333204584786));
#8869=CARTESIAN_POINT('Ctrl Pts',(1.9774028104633,5.78709319740479,3.48105680795096));
#8870=CARTESIAN_POINT('Ctrl Pts',(1.81551131753373,5.83744329466308,3.48878157005407));
#8871=CARTESIAN_POINT('Ctrl Pts',(1.6536514045795,5.88778357018954,3.49650482529729));
#8872=CARTESIAN_POINT('Ctrl Pts',(1.48967741677477,5.93139357275478,3.50422808054051));
#8873=CARTESIAN_POINT('Ctrl Pts',(1.324164893687,5.9681163608652,3.51195133578372));
#8874=CARTESIAN_POINT('Ctrl Pts',(1.15864597433448,6.00484056813516,3.51967488949369));
#8875=CARTESIAN_POINT('Ctrl Pts',(0.991588709257809,6.03467695583886,3.52739844320366));
#8876=CARTESIAN_POINT('Ctrl Pts',(0.823580401719469,6.05751936723306,3.53512199691363));
#8877=CARTESIAN_POINT('Ctrl Pts',(0.655583378381846,6.08036024442719,3.54284503187467));
#8878=CARTESIAN_POINT('Ctrl Pts',(0.486635754478305,6.09620804265871,3.5505680668357));
#8879=CARTESIAN_POINT('Ctrl Pts',(0.317331737426225,6.10500828262518,3.55829110179674));
#8880=CARTESIAN_POINT('Ctrl Pts',(0.147982726742336,6.11381086131204,3.56601618920401));
#8881=CARTESIAN_POINT('Ctrl Pts',(-0.021722549741907,6.11556212051749,3.57374127661127));
#8882=CARTESIAN_POINT('Ctrl Pts',(-0.191187119584226,6.11025965469595,3.58146636401854));
#8883=CARTESIAN_POINT('Ctrl Pts',(-0.359994562703326,6.10497775005717,3.58916149612967));
#8884=CARTESIAN_POINT('Ctrl Pts',(-0.528562851593163,6.092696769089,3.5968566282408));
#8885=CARTESIAN_POINT('Ctrl Pts',(-0.696304355874567,6.07346571625214,3.60455176035192));
#8886=CARTESIAN_POINT('Ctrl Pts',(-0.864691746330856,6.0541606145315,3.61227652245514));
#8887=CARTESIAN_POINT('Ctrl Pts',(-1.03230560687944,6.02784494527547,3.62000128455836));
#8888=CARTESIAN_POINT('Ctrl Pts',(-1.19855571209354,5.99460505517319,3.62772604666157));
#8889=CARTESIAN_POINT('Ctrl Pts',(-1.36477338710263,5.96137164913568,3.63544930190488));
#8890=CARTESIAN_POINT('Ctrl Pts',(-1.52962752700772,5.92121677947923,3.64317255714818));
#8891=CARTESIAN_POINT('Ctrl Pts',(-1.6925376500896,5.87427798674264,3.65089581239149));
#8892=CARTESIAN_POINT('Ctrl Pts',(-1.85545406886596,5.82733738004696,3.65861936610155));
#8893=CARTESIAN_POINT('Ctrl Pts',(-2.01642601485949,5.77361240959754,3.6663429198116));
#8894=CARTESIAN_POINT('Ctrl Pts',(-2.17488697325315,5.71329083944392,3.67406647352166));
#8895=CARTESIAN_POINT('Ctrl Pts',(-2.3333372886891,5.65297332076093,3.68178950848277));
#8896=CARTESIAN_POINT('Ctrl Pts',(-2.48927665780199,5.58606020177335,3.68951254344388));
#8897=CARTESIAN_POINT('Ctrl Pts',(-2.64215722705511,5.51278792899023,3.69723557840499));
#8898=CARTESIAN_POINT('Ctrl Pts',(-2.79507842530368,5.43949618362894,3.70496066581236));
#8899=CARTESIAN_POINT('Ctrl Pts',(-2.94493891238881,5.35984204257687,3.71268575321972));
#8900=CARTESIAN_POINT('Ctrl Pts',(-3.09121332034152,5.27410900253713,3.72041084062709));
#8901=CARTESIAN_POINT('Ctrl Pts',(-3.23692052522489,5.18870840645757,3.72810597273777));
#8902=CARTESIAN_POINT('Ctrl Pts',(-3.37906915972562,5.09727615711957,3.73580110484845));
#8903=CARTESIAN_POINT('Ctrl Pts',(-3.51716665543486,5.00013642617851,3.74349623695913));
#8904=CARTESIAN_POINT('Ctrl Pts',(-3.65579589351149,4.90262266013831,3.75122099906233));
#8905=CARTESIAN_POINT('Ctrl Pts',(-3.79039181424287,4.7993228110639,3.75894576116554));
#8906=CARTESIAN_POINT('Ctrl Pts',(-3.92047743605519,4.69059508334306,3.76667052326874));
#8907=CARTESIAN_POINT('Ctrl Pts',(-4.05053768222588,4.58188856500582,3.77439377851214));
#8908=CARTESIAN_POINT('Ctrl Pts',(-4.17608914200571,4.46775648385058,3.78211703375554));
#8909=CARTESIAN_POINT('Ctrl Pts',(-4.29668788265976,4.34859733724621,3.78984028899894));
#8910=CARTESIAN_POINT('Ctrl Pts',(-4.41729128387497,4.22943358571406,3.797563842709));
#8911=CARTESIAN_POINT('Ctrl Pts',(-4.53294135474333,4.10524259991034,3.80528739641906));
#8912=CARTESIAN_POINT('Ctrl Pts',(-4.64323045562768,3.97646029760535,3.81301095012911));
#8913=CARTESIAN_POINT('Ctrl Pts',(-4.75351214899525,3.84768664490451,3.82073398509024));
#8914=CARTESIAN_POINT('Ctrl Pts',(-4.85843338676705,3.71432253355324,3.82845702005136));
#8915=CARTESIAN_POINT('Ctrl Pts',(-4.95762620737575,3.5768377025581,3.83618005501249));
#8916=CARTESIAN_POINT('Ctrl Pts',(-5.0568453891149,3.43931633408433,3.84390514241986));
#8917=CARTESIAN_POINT('Ctrl Pts',(-5.15033292430782,3.29767231359746,3.85163022982722));
#8918=CARTESIAN_POINT('Ctrl Pts',(-5.23776310674007,3.15240593835448,3.85935531723459));
#8919=CARTESIAN_POINT('Ctrl Pts',(-5.32485426426226,3.00770285737021,3.86705044934517));
#8920=CARTESIAN_POINT('Ctrl Pts',(-5.40593482891385,2.85940574834771,3.87474558145574));
#8921=CARTESIAN_POINT('Ctrl Pts',(-5.48072735671713,2.70803493401257,3.88244071356631));
#8922=CARTESIAN_POINT('Ctrl Pts',(-5.55558719194807,2.55652789777887,3.89014277069417));
#8923=CARTESIAN_POINT('Ctrl Pts',(-5.62417561300256,2.40188493173974,3.89784482782203));
#8924=CARTESIAN_POINT('Ctrl Pts',(-5.68624590948509,2.24464541060813,3.90554688494989));
#8925=CARTESIAN_POINT('Ctrl Pts',(-5.74830346396685,2.08743816813815,3.91324736097337));
#8926=CARTESIAN_POINT('Ctrl Pts',(-5.80384544591209,1.92763573217092,3.92094783699684));
#8927=CARTESIAN_POINT('Ctrl Pts',(-5.85267341985573,1.76579710131551,3.92864831302032));
#8928=CARTESIAN_POINT('Ctrl Pts',(-5.9015019239919,1.60395671315531,3.93634887265846));
#8929=CARTESIAN_POINT('Ctrl Pts',(-5.94361617794235,1.44008039172325,3.94404943229661));
#8930=CARTESIAN_POINT('Ctrl Pts',(-5.97886752376897,1.27474259979051,3.95174999193475));
#8931=CARTESIAN_POINT('Ctrl Pts',(-6.01411712626691,1.1094129845134,3.95945017074754));
#8932=CARTESIAN_POINT('Ctrl Pts',(-6.04250443368888,0.9426223571398,3.96715034956032));
#8933=CARTESIAN_POINT('Ctrl Pts',(-6.06393180476829,0.774955888821809,3.9748505283731));
#8934=CARTESIAN_POINT('Ctrl Pts',(-6.08536381698891,0.607253104160884,3.98255237503479));
#8935=CARTESIAN_POINT('Ctrl Pts',(-6.0998328402343,0.438674417704038,3.99025422169647));
#8936=CARTESIAN_POINT('Ctrl Pts',(-6.10729296440831,0.26981143302088,3.99795606835815));
#8937=CARTESIAN_POINT('Ctrl Pts',(-6.1112652219098,0.179897747673746,4.0020570347045));
#8938=CARTESIAN_POINT('Ctrl Pts',(-6.11325120176772,0.0899035318141606,
4.00615800105085));
#8939=CARTESIAN_POINT('Ctrl Pts',(-6.11324999945432,-8.1680558123466E-5,
4.0102589673972));
#8940=CARTESIAN_POINT('Ctrl Pts',(-6.11324999945431,-8.16814850665972E-5,
4.01025896743945));
#8941=CARTESIAN_POINT('Ctrl Pts',(-6.11324891212047,-0.081460510364748,
4.0139677083508));
#8942=CARTESIAN_POINT('Ctrl Pts',(-6.11162270832985,-0.162834847314414,
4.01767644926215));
#8943=CARTESIAN_POINT('Ctrl Pts',(-6.10837287883718,-0.244144087756446,
4.0213851901735));
#8944=CARTESIAN_POINT('Ctrl Pts',(-6.10160396175534,-0.413499282476559,
4.02910995227672));
#8945=CARTESIAN_POINT('Ctrl Pts',(-6.08778642357728,-0.582602790231776,
4.03683471437994));
#8946=CARTESIAN_POINT('Ctrl Pts',(-6.06696261821026,-0.750859608541673,
4.04455947648316));
#8947=CARTESIAN_POINT('Ctrl Pts',(-6.04614287491734,-0.919083605200879,
4.05228273172653));
#8948=CARTESIAN_POINT('Ctrl Pts',(-6.0183196304021,-1.08646092763768,4.0600059869699));
#8949=CARTESIAN_POINT('Ctrl Pts',(-5.98358701388492,-1.25240249511397,4.06772924221327));
#8950=CARTESIAN_POINT('Ctrl Pts',(-5.94885305511907,-1.4183504754342,4.07545279592333));
#8951=CARTESIAN_POINT('Ctrl Pts',(-5.90720925108868,-1.58286227875742,4.0831763496334));
#8952=CARTESIAN_POINT('Ctrl Pts',(-5.85880085173651,-1.74535902959579,4.09089990334346));
#8953=CARTESIAN_POINT('Ctrl Pts',(-5.81039570371216,-1.90784486641479,4.09862293830459));
#8954=CARTESIAN_POINT('Ctrl Pts',(-5.75522696007558,-2.06831561782367,4.10634597326573));
#8955=CARTESIAN_POINT('Ctrl Pts',(-5.69348980268939,-2.2262074092887,4.11406900822687));
#8956=CARTESIAN_POINT('Ctrl Pts',(-5.63173623825635,-2.38414116151334,4.12179409563424));
#8957=CARTESIAN_POINT('Ctrl Pts',(-5.56341088540832,-2.53949428808111,4.12951918304162));
#8958=CARTESIAN_POINT('Ctrl Pts',(-5.48875751365973,-2.69172185018138,4.13724427044899));
#8959=CARTESIAN_POINT('Ctrl Pts',(-5.41439362263685,-2.84335912487575,4.14493940255955));
#8960=CARTESIAN_POINT('Ctrl Pts',(-5.33375086774613,-2.9918947656903,4.15263453467011));
#8961=CARTESIAN_POINT('Ctrl Pts',(-5.24711601306163,-3.13681352776544,4.16032966678067));
#8962=CARTESIAN_POINT('Ctrl Pts',(-5.16014757214769,-3.28229029739528,4.16805442888386));
#8963=CARTESIAN_POINT('Ctrl Pts',(-5.06710996744875,-3.42417378765433,4.17577919098705));
#8964=CARTESIAN_POINT('Ctrl Pts',(-4.96832505762452,-3.56196177467984,4.18350395309024));
#8965=CARTESIAN_POINT('Ctrl Pts',(-4.86955941765144,-3.69972288357177,4.19122720833357));
#8966=CARTESIAN_POINT('Ctrl Pts',(-4.76504889413752,-3.83338982591715,4.19895046357689));
#8967=CARTESIAN_POINT('Ctrl Pts',(-4.65515797786181,-3.96249034871374,4.20667371882021));
#8968=CARTESIAN_POINT('Ctrl Pts',(-4.54526281483007,-4.09159586062538,4.21439727253025));
#8969=CARTESIAN_POINT('Ctrl Pts',(-4.42998704536689,-4.21613435596427,4.22212082624029));
#8970=CARTESIAN_POINT('Ctrl Pts',(-4.30973516820192,-4.33566700087352,4.22984437995033));
#8971=CARTESIAN_POINT('Ctrl Pts',(-4.18949136769876,-4.45519161742786,4.23756741491145));
#8972=CARTESIAN_POINT('Ctrl Pts',(-4.0642723531173,-4.56971083293029,4.24529044987257));
#8973=CARTESIAN_POINT('Ctrl Pts',(-3.93451929281437,-4.67882287514408,4.25301348483369));
#8974=CARTESIAN_POINT('Ctrl Pts',(-3.80473174980083,-4.78796391458512,4.26073857224104));
#8975=CARTESIAN_POINT('Ctrl Pts',(-3.67040799460991,-4.89169470349284,4.26846365964839));
#8976=CARTESIAN_POINT('Ctrl Pts',(-3.53202280228015,-4.9896533433369,4.27618874705574));
#8977=CARTESIAN_POINT('Ctrl Pts',(-3.39417422128802,-5.08723213244784,4.28388387916645));
#8978=CARTESIAN_POINT('Ctrl Pts',(-3.25229591838128,-5.17908330377386,4.29157901127716));
#8979=CARTESIAN_POINT('Ctrl Pts',(-3.10688621678911,-5.26489160367294,4.29927414338787));
#8980=CARTESIAN_POINT('Ctrl Pts',(-2.96091661728943,-5.35103030716294,4.30699890549107));
#8981=CARTESIAN_POINT('Ctrl Pts',(-2.81133665657384,-5.43110999278065,4.31472366759427));
#8982=CARTESIAN_POINT('Ctrl Pts',(-2.6586692457176,-5.50484363123744,4.32244842969748));
#8983=CARTESIAN_POINT('Ctrl Pts',(-2.50603161550612,-5.57856288656373,4.33017168494081));
#8984=CARTESIAN_POINT('Ctrl Pts',(-2.35030802210038,-5.64593842706568,4.33789494018413));
#8985=CARTESIAN_POINT('Ctrl Pts',(-2.19204447401633,-5.70672993810242,4.34561819542746));
#8986=CARTESIAN_POINT('Ctrl Pts',(-2.03377480980615,-5.76752379843914,4.35334174913751));
#8987=CARTESIAN_POINT('Ctrl Pts',(-1.87296528892247,-5.82173300282247,4.36106530284756));
#8988=CARTESIAN_POINT('Ctrl Pts',(-1.71018106321062,-5.86916572380912,4.36878885655762));
#8989=CARTESIAN_POINT('Ctrl Pts',(-1.54740777082637,-5.91659525899888,4.37651189151874));
#8990=CARTESIAN_POINT('Ctrl Pts',(-1.3826603433326,-5.95724913293791,4.38423492647986));
#8991=CARTESIAN_POINT('Ctrl Pts',(-1.2165184017685,-5.99098560678113,4.39195796144099));
#8992=CARTESIAN_POINT('Ctrl Pts',(-1.05033230691417,-6.02473104630939,4.39968304884835));
#8993=CARTESIAN_POINT('Ctrl Pts',(-0.882751267811871,-6.05155534703707,
4.40740813625572));
#8994=CARTESIAN_POINT('Ctrl Pts',(-0.714365339658028,-6.07136786268097,
4.41513322366309));
#8995=CARTESIAN_POINT('Ctrl Pts',(-0.546632355629441,-6.09110355203755,
4.42282835577374));
#8996=CARTESIAN_POINT('Ctrl Pts',(-0.378101027449535,-6.10388173387967,
4.4305234878844));
#8997=CARTESIAN_POINT('Ctrl Pts',(-0.20935977231692,-6.10966398816133,4.43821861999506));
#8998=CARTESIAN_POINT('Ctrl Pts',(-0.0399687814736328,-6.1154685069277,
4.44594338209826));
#8999=CARTESIAN_POINT('Ctrl Pts',(0.129693750450044,-6.11422514153443,4.45366814420145));
#9000=CARTESIAN_POINT('Ctrl Pts',(0.299031318382102,-6.10593202002173,4.46139290630465));
#9001=CARTESIAN_POINT('Ctrl Pts',(0.468335853842491,-6.09764051623807,4.46911616154798));
#9002=CARTESIAN_POINT('Ctrl Pts',(0.637315235442858,-6.08230201581923,4.4768394167913));
#9003=CARTESIAN_POINT('Ctrl Pts',(0.805375025299262,-6.05996671864823,4.48456267203463));
#9004=CARTESIAN_POINT('Ctrl Pts',(0.973441309859275,-6.03763055832528,4.49228622574468));
#9005=CARTESIAN_POINT('Ctrl Pts',(1.14058761688449,-6.00829709800294,4.50000977945472));
#9006=CARTESIAN_POINT('Ctrl Pts',(1.30622589592708,-5.97206827416679,4.50773333316477));
#9007=CARTESIAN_POINT('Ctrl Pts',(1.47185304995097,-5.93584188362291,4.51545636812588));
#9008=CARTESIAN_POINT('Ctrl Pts',(1.63597206904608,-5.89272112408309,4.52317940308701));
#9009=CARTESIAN_POINT('Ctrl Pts',(1.79800616083802,-5.84285883862416,4.53090243804812));
#9010=CARTESIAN_POINT('Ctrl Pts',(1.96008331423251,-5.79298330194202,4.53862752545548));
#9011=CARTESIAN_POINT('Ctrl Pts',(2.12007412936835,-5.73636275047694,4.54635261286283));
#9012=CARTESIAN_POINT('Ctrl Pts',(2.27741709554115,-5.67319988502405,4.55407770027018));
#9013=CARTESIAN_POINT('Ctrl Pts',(2.4341499384906,-5.61028194396788,4.56177283238087));
#9014=CARTESIAN_POINT('Ctrl Pts',(2.5882551532058,-5.54087248274603,4.56946796449157));
#9015=CARTESIAN_POINT('Ctrl Pts',(2.73919765391028,-5.46521927970986,4.57716309660226));
#9016=CARTESIAN_POINT('Ctrl Pts',(2.89071986958217,-5.38927552037625,4.58488778290239));
#9017=CARTESIAN_POINT('Ctrl Pts',(3.0391086801984,-5.30701304086964,4.59261246920252));
#9018=CARTESIAN_POINT('Ctrl Pts',(3.18383939880802,-5.21871557426708,4.60033715550265));
#9019=CARTESIAN_POINT('Ctrl Pts',(3.3285436798381,-5.13043423673041,4.60806043075467));
#9020=CARTESIAN_POINT('Ctrl Pts',(3.46959093155419,-5.03612027631624,4.61578370600668));
#9021=CARTESIAN_POINT('Ctrl Pts',(3.60648317551241,-4.93610217350147,4.62350698125869));
#9022=CARTESIAN_POINT('Ctrl Pts',(3.64564048854767,-4.9074925163882,4.62571618389834));
#9023=CARTESIAN_POINT('Ctrl Pts',(3.68445801165065,-4.87841640971667,4.627925386538));
#9024=CARTESIAN_POINT('Ctrl Pts',(3.72292453512038,-4.84888218750453,4.63013458917765));
#9025=CARTESIAN_POINT('',(-6.11324999817629,-0.000149323895545952,3.86474103251618));
#9026=CARTESIAN_POINT('Ctrl Pts',(-6.11324999817626,-0.000149324869336022,
3.86474103256055));
#9027=CARTESIAN_POINT('Ctrl Pts',(-6.11324540503865,-0.188188990505417,
3.87330913670744));
#9028=CARTESIAN_POINT('Ctrl Pts',(-6.10455976566219,-0.376188117694265,
3.88187724085434));
#9029=CARTESIAN_POINT('Ctrl Pts',(-6.08723465950245,-0.563382430194741,
3.89044534500124));
#9030=CARTESIAN_POINT('Ctrl Pts',(-6.07161483028389,-0.732151565863044,
3.89817010710471));
#9031=CARTESIAN_POINT('Ctrl Pts',(-6.0489692004611,-0.900300595441643,3.90589486920817));
#9032=CARTESIAN_POINT('Ctrl Pts',(-6.01937119477572,-1.0672375471301,3.91361963131164));
#9033=CARTESIAN_POINT('Ctrl Pts',(-5.98977896273696,-1.23414193463244,3.92134288655525));
#9034=CARTESIAN_POINT('Ctrl Pts',(-5.95323711621792,-1.39983440415421,3.92906614179887));
#9035=CARTESIAN_POINT('Ctrl Pts',(-5.9098704745594,-1.56373160626468,3.93678939704248));
#9036=CARTESIAN_POINT('Ctrl Pts',(-5.86650215698853,-1.72763514221457,3.9445129507528));
#9037=CARTESIAN_POINT('Ctrl Pts',(-5.81630859374343,-1.88974296453487,3.95223650446312));
#9038=CARTESIAN_POINT('Ctrl Pts',(-5.7594651209688,-2.04948458956,3.95996005817344));
#9039=CARTESIAN_POINT('Ctrl Pts',(-5.70262546605979,-2.20921548561255,3.96768309313483));
#9040=CARTESIAN_POINT('Ctrl Pts',(-5.63913690168427,-2.3665802037917,3.97540612809623));
#9041=CARTESIAN_POINT('Ctrl Pts',(-5.56922384271879,-2.52102585313848,3.98312916305763));
#9042=CARTESIAN_POINT('Ctrl Pts',(-5.49929220390803,-2.67551254741034,3.99085425046526));
#9043=CARTESIAN_POINT('Ctrl Pts',(-5.42293278760885,-2.82707833286508,3.99857933787289));
#9044=CARTESIAN_POINT('Ctrl Pts',(-5.3404175391466,-2.97519177030244,4.00630442528053));
#9045=CARTESIAN_POINT('Ctrl Pts',(-5.25822225714617,-3.12273087349967,4.01399955738982));
#9046=CARTESIAN_POINT('Ctrl Pts',(-5.16991897872069,-3.2668440981476,4.02169468949912));
#9047=CARTESIAN_POINT('Ctrl Pts',(-5.07582103137174,-3.40703190768509,4.02938982160841));
#9048=CARTESIAN_POINT('Ctrl Pts',(-4.98136076125069,-3.54775950833596,4.03711458371152));
#9049=CARTESIAN_POINT('Ctrl Pts',(-4.88102762909894,-3.68458122915613,4.04483934581462));
#9050=CARTESIAN_POINT('Ctrl Pts',(-4.775169327721,-3.81701237279794,4.05256410791773));
#9051=CARTESIAN_POINT('Ctrl Pts',(-4.66933167599206,-3.94941768325901,4.06028736316097));
#9052=CARTESIAN_POINT('Ctrl Pts',(-4.55797120337342,-4.07743387808856,4.06801061840421));
#9053=CARTESIAN_POINT('Ctrl Pts',(-4.44147660841494,-4.20060842014617,4.07573387364745));
#9054=CARTESIAN_POINT('Ctrl Pts',(-4.32497751150002,-4.32378772230809,4.0834574273574));
#9055=CARTESIAN_POINT('Ctrl Pts',(-4.20334411010281,-4.44212476431314,4.09118098106735));
#9056=CARTESIAN_POINT('Ctrl Pts',(-4.07700330753907,-4.55520247550155,4.0989045347773));
#9057=CARTESIAN_POINT('Ctrl Pts',(-3.95067099059709,-4.66827259187763,4.10662756973833));
#9058=CARTESIAN_POINT('Ctrl Pts',(-3.81963214137809,-4.77608387295123,4.11435060469935));
#9059=CARTESIAN_POINT('Ctrl Pts',(-3.68434834364815,-4.87825817737819,4.12207363966038));
#9060=CARTESIAN_POINT('Ctrl Pts',(-3.54902859337836,-4.98045963528407,4.12979872706765));
#9061=CARTESIAN_POINT('Ctrl Pts',(-3.4094618921013,-5.07702093017004,4.13752381447492));
#9062=CARTESIAN_POINT('Ctrl Pts',(-3.26614129816218,-5.16760549799803,4.14524890188219));
#9063=CARTESIAN_POINT('Ctrl Pts',(-3.12337645338244,-5.25783880927565,4.15294403399333));
#9064=CARTESIAN_POINT('Ctrl Pts',(-2.97688705798117,-5.34214152303887,4.16063916610447));
#9065=CARTESIAN_POINT('Ctrl Pts',(-2.82718724591767,-5.420224888233,4.16833429821561));
#9066=CARTESIAN_POINT('Ctrl Pts',(-2.6769110169479,-5.49860891226682,4.17605906031882));
#9067=CARTESIAN_POINT('Ctrl Pts',(-2.52334636165946,-5.57075333230414,4.18378382242203));
#9068=CARTESIAN_POINT('Ctrl Pts',(-2.36703049156718,-5.63639886935721,4.19150858452525));
#9069=CARTESIAN_POINT('Ctrl Pts',(-2.21074511381998,-5.70203160101588,4.19923183976859));
#9070=CARTESIAN_POINT('Ctrl Pts',(-2.05170988415776,-5.76116785662558,4.20695509501193));
#9071=CARTESIAN_POINT('Ctrl Pts',(-1.89048263592708,-5.81359621626392,4.21467835025528));
#9072=CARTESIAN_POINT('Ctrl Pts',(-1.72924915703758,-5.86602660200657,4.22240190396534));
#9073=CARTESIAN_POINT('Ctrl Pts',(-1.56582379022629,-5.911748471275,4.23012545767541));
#9074=CARTESIAN_POINT('Ctrl Pts',(-1.40078094924048,-5.95059982646665,4.23784901138547));
#9075=CARTESIAN_POINT('Ctrl Pts',(-1.23574919328105,-5.98944857222493,4.24557204634661));
#9076=CARTESIAN_POINT('Ctrl Pts',(-1.06910048907319,-6.02142765473253,4.25329508130775));
#9077=CARTESIAN_POINT('Ctrl Pts',(-0.901421079249796,-6.04642585337686,
4.26101811626889));
#9078=CARTESIAN_POINT('Ctrl Pts',(-0.73369710754433,-6.07143069545334,4.26874320367626));
#9079=CARTESIAN_POINT('Ctrl Pts',(-0.564942196233197,-6.0894508975762,4.27646829108363));
#9080=CARTESIAN_POINT('Ctrl Pts',(-0.395750334799665,-6.10042680760994,
4.28419337849101));
#9081=CARTESIAN_POINT('Ctrl Pts',(-0.227214542631636,-6.11136015674758,
4.2918885106016));
#9082=CARTESIAN_POINT('Ctrl Pts',(-0.0582454966302977,-6.11530375944402,
4.2995836427122));
#9083=CARTESIAN_POINT('Ctrl Pts',(0.110567181803888,-6.11225003258276,4.3072787748228));
#9084=CARTESIAN_POINT('Ctrl Pts',(0.280029870964719,-6.10918454739129,4.31500353692601));
#9085=CARTESIAN_POINT('Ctrl Pts',(0.449395004085272,-6.09906662372046,4.32272829902921));
#9086=CARTESIAN_POINT('Ctrl Pts',(0.61806679505976,-6.08192559962259,4.33045306113242));
#9087=CARTESIAN_POINT('Ctrl Pts',(0.786705683434824,-6.06478791920327,4.33817631637576));
#9088=CARTESIAN_POINT('Ctrl Pts',(0.954651184423808,-6.04062990399549,4.3458995716191));
#9089=CARTESIAN_POINT('Ctrl Pts',(1.1213123005287,-6.00953278443366,4.35362282686244));
#9090=CARTESIAN_POINT('Ctrl Pts',(1.28797985728529,-5.97843446311752,4.3613463805725));
#9091=CARTESIAN_POINT('Ctrl Pts',(1.45336261756681,-5.94039655507275,4.36906993428256));
#9092=CARTESIAN_POINT('Ctrl Pts',(1.61687866927581,-5.8955516223116,4.37679348799262));
#9093=CARTESIAN_POINT('Ctrl Pts',(1.78038373850458,-5.85070970153968,4.38451652295376));
#9094=CARTESIAN_POINT('Ctrl Pts',(1.94202204439148,-5.79906175480238,4.39223955791489));
#9095=CARTESIAN_POINT('Ctrl Pts',(2.10122558078278,-5.74079059199724,4.39996259287603));
#9096=CARTESIAN_POINT('Ctrl Pts',(2.26047142653828,-5.68250394325564,4.4076876802834));
#9097=CARTESIAN_POINT('Ctrl Pts',(2.41728091124755,-5.61759066817747,4.41541276769077));
#9098=CARTESIAN_POINT('Ctrl Pts',(2.57110389791294,-5.54628256660593,4.42313785509814));
#9099=CARTESIAN_POINT('Ctrl Pts',(2.7243304106525,-5.47525097392432,4.43083298720876));
#9100=CARTESIAN_POINT('Ctrl Pts',(2.87459327577343,-5.39787422111947,4.43852811931937));
#9101=CARTESIAN_POINT('Ctrl Pts',(3.02137110334711,-5.31442774138091,4.44622325142999));
#9102=CARTESIAN_POINT('Ctrl Pts',(3.16871553818466,-5.23065913273266,4.45394808910188));
#9103=CARTESIAN_POINT('Ctrl Pts',(3.31260014595631,-5.14074414708694,4.46167292677376));
#9104=CARTESIAN_POINT('Ctrl Pts',(3.45251577270222,-5.04499359779003,4.46939776444565));
#9105=CARTESIAN_POINT('Ctrl Pts',(3.54440943264835,-4.98210663783149,4.47447127640903));
#9106=CARTESIAN_POINT('Ctrl Pts',(3.63459155151057,-4.91670339231516,4.47954478837242));
#9107=CARTESIAN_POINT('Ctrl Pts',(3.72292453512037,-4.84888218750453,4.4846183003358));
#9108=CARTESIAN_POINT('Ctrl Pts',(3.72292453512037,-4.84888218750454,2.73461001778677));
#9109=CARTESIAN_POINT('Ctrl Pts',(3.85742670434484,-4.74561273147958,2.74233503114518));
#9110=CARTESIAN_POINT('Ctrl Pts',(3.98762056731902,-4.63675019710229,2.75006004450358));
#9111=CARTESIAN_POINT('Ctrl Pts',(4.11305073883802,-4.52268053064154,2.75778505786199));
#9112=CARTESIAN_POINT('Ctrl Pts',(4.22727439585806,-4.41880237835639,2.76481988262257));
#9113=CARTESIAN_POINT('Ctrl Pts',(4.33754781035837,-4.31060659422731,2.77185470738315));
#9114=CARTESIAN_POINT('Ctrl Pts',(4.44355277819139,-4.19841211292169,2.77888953214373));
#9115=CARTESIAN_POINT('Ctrl Pts',(4.55995413570729,-4.07521420817501,2.78661429418798));
#9116=CARTESIAN_POINT('Ctrl Pts',(4.67124943892527,-3.94715064688156,2.79433905623222));
#9117=CARTESIAN_POINT('Ctrl Pts',(4.77704270982733,-3.81466754920865,2.80206381827647));
#9118=CARTESIAN_POINT('Ctrl Pts',(4.88281534375428,-3.68221029486554,2.80978707346002));
#9119=CARTESIAN_POINT('Ctrl Pts',(4.98308788929193,-3.54533547187285,2.81751032864357));
#9120=CARTESIAN_POINT('Ctrl Pts',(5.07750478792242,-3.40452209438049,2.82523358382712));
#9121=CARTESIAN_POINT('Ctrl Pts',(5.17192533530416,-3.26370327513993,2.8329571374767));
#9122=CARTESIAN_POINT('Ctrl Pts',(5.26048960316994,-3.11894585784414,2.84068069112628));
#9123=CARTESIAN_POINT('Ctrl Pts',(5.34288505882612,-2.97075828883344,2.84840424477586));
#9124=CARTESIAN_POINT('Ctrl Pts',(5.42527498042637,-2.82258067277815,2.85612727967622));
#9125=CARTESIAN_POINT('Ctrl Pts',(5.50149676492954,-2.67097364306444,2.86385031457659));
#9126=CARTESIAN_POINT('Ctrl Pts',(5.57128350479845,-2.5164708763784,2.87157334947695));
#9127=CARTESIAN_POINT('Ctrl Pts',(5.64108879094418,-2.3619270495843,2.87929843682372));
#9128=CARTESIAN_POINT('Ctrl Pts',(5.7044554826127,-2.20448623618459,2.88702352417049));
#9129=CARTESIAN_POINT('Ctrl Pts',(5.76116417231926,-2.04470363184618,2.89474861151725));
#9130=CARTESIAN_POINT('Ctrl Pts',(5.81765296740604,-1.88554060336482,2.90244374392848));
#9131=CARTESIAN_POINT('Ctrl Pts',(5.86753522907989,-1.72405421779254,2.9101388763397));
#9132=CARTESIAN_POINT('Ctrl Pts',(5.91064283593141,-1.56080967082881,2.91783400875093));
#9133=CARTESIAN_POINT('Ctrl Pts',(5.95391642647975,-1.39693655885368,2.92555877088689));
#9134=CARTESIAN_POINT('Ctrl Pts',(5.99037838488768,-1.23123367253846,2.93328353302285));
#9135=CARTESIAN_POINT('Ctrl Pts',(6.0198944294592,-1.06428220912787,2.94100829515882));
#9136=CARTESIAN_POINT('Ctrl Pts',(6.04940471637381,-0.897363312724832,2.94873155043535));
#9137=CARTESIAN_POINT('Ctrl Pts',(6.07197173788201,-0.729196637109618,2.95645480571189));
#9138=CARTESIAN_POINT('Ctrl Pts',(6.08751244314942,-0.560372926720169,2.96417806098842));
#9139=CARTESIAN_POINT('Ctrl Pts',(6.10305374899113,-0.391542692097803,2.97190161473202));
#9140=CARTESIAN_POINT('Ctrl Pts',(6.11156816224163,-0.22205568711227,2.97962516847561));
#9141=CARTESIAN_POINT('Ctrl Pts',(6.11302449538673,-0.0525079165631778,
2.9873487222192));
#9142=CARTESIAN_POINT('Ctrl Pts',(6.11448073071791,0.117028466390709,2.99507175721399));
#9143=CARTESIAN_POINT('Ctrl Pts',(6.1088798318847,0.286625289795099,3.00279479220878));
#9144=CARTESIAN_POINT('Ctrl Pts',(6.09624274694914,0.455686221834749,3.01051782720356));
#9145=CARTESIAN_POINT('Ctrl Pts',(6.08360230362713,0.624792082902369,3.01824291464448));
#9146=CARTESIAN_POINT('Ctrl Pts',(6.06392195913237,0.793361451592205,3.02596800208539));
#9147=CARTESIAN_POINT('Ctrl Pts',(6.03727466787266,0.960801825124741,3.03369308952631));
#9148=CARTESIAN_POINT('Ctrl Pts',(6.01073070655698,1.12759291673757,3.04138822147024));
#9149=CARTESIAN_POINT('Ctrl Pts',(5.97727381465468,1.29326345017323,3.04908335341418));
#9150=CARTESIAN_POINT('Ctrl Pts',(5.9370267664945,1.45723667824685,3.05677848535811));
#9151=CARTESIAN_POINT('Ctrl Pts',(5.89662474686772,1.62184128608116,3.0645032474473));
#9152=CARTESIAN_POINT('Ctrl Pts',(5.84936583776353,1.78479378253571,3.07222800953649));
#9153=CARTESIAN_POINT('Ctrl Pts',(5.79541018467373,1.9455195588531,3.07995277162568));
#9154=CARTESIAN_POINT('Ctrl Pts',(5.7414650566483,2.10621398258659,3.08767602685482));
#9155=CARTESIAN_POINT('Ctrl Pts',(5.6808258920245,2.26468225262756,3.09539928208395));
#9156=CARTESIAN_POINT('Ctrl Pts',(5.61370239110768,2.42036588692122,3.10312253731309));
#9157=CARTESIAN_POINT('Ctrl Pts',(5.54657629619104,2.57605553763705,3.11084609100882));
#9158=CARTESIAN_POINT('Ctrl Pts',(5.47296548537579,2.72896004467673,3.11856964470455));
#9159=CARTESIAN_POINT('Ctrl Pts',(5.39312771821359,2.87854111965354,3.12629319840029));
#9160=CARTESIAN_POINT('Ctrl Pts',(5.31329531331895,3.02811214808504,3.13401623334702));
#9161=CARTESIAN_POINT('Ctrl Pts',(5.22723693827673,3.1743599115294,3.14173926829376));
#9162=CARTESIAN_POINT('Ctrl Pts',(5.13525629070301,3.31677077762319,3.1494623032405));
#9163=CARTESIAN_POINT('Ctrl Pts',(5.04325119867929,3.45921949032262,3.15718739063356));
#9164=CARTESIAN_POINT('Ctrl Pts',(4.9453208593657,3.59782900050773,3.16491247802662));
#9165=CARTESIAN_POINT('Ctrl Pts',(4.84181280658558,3.73211391954799,3.17263756541967));
#9166=CARTESIAN_POINT('Ctrl Pts',(4.73870612215536,3.86587812821911,3.18033269760155));
#9167=CARTESIAN_POINT('Ctrl Pts',(4.63006512036532,3.9953509970781,3.18802782978343));
#9168=CARTESIAN_POINT('Ctrl Pts',(4.51627354531815,4.12008480815134,3.19572296196531));
#9169=CARTESIAN_POINT('Ctrl Pts',(4.40204381848931,4.24529890382852,3.20344772407255));
#9170=CARTESIAN_POINT('Ctrl Pts',(4.28258329639064,4.36578170088513,3.21117248617979));
#9171=CARTESIAN_POINT('Ctrl Pts',(4.15830751659645,4.48110523865681,3.21889724828703));
#9172=CARTESIAN_POINT('Ctrl Pts',(4.03405597912532,4.59640628040822,3.22662050353445));
#9173=CARTESIAN_POINT('Ctrl Pts',(3.90499129038211,4.70654985557746,3.23434375878188));
#9174=CARTESIAN_POINT('Ctrl Pts',(3.77156478783028,4.81114587325085,3.2420670140293));
#9175=CARTESIAN_POINT('Ctrl Pts',(3.63813312898482,4.91574593305808,3.24979056774346));
#9176=CARTESIAN_POINT('Ctrl Pts',(3.50033956599702,5.01479780772929,3.25751412145761));
#9177=CARTESIAN_POINT('Ctrl Pts',(3.35866797716767,5.10795213188695,3.26523767517177));
#9178=CARTESIAN_POINT('Ctrl Pts',(3.21700590364524,5.20110019937739,3.272960710137));
#9179=CARTESIAN_POINT('Ctrl Pts',(3.07146659035469,5.28835133489436,3.28068374510223));
#9180=CARTESIAN_POINT('Ctrl Pts',(2.92256245884773,5.36939980227157,3.28840678006746));
#9181=CARTESIAN_POINT('Ctrl Pts',(2.77361875511016,5.45046980880023,3.2961318674789));
#9182=CARTESIAN_POINT('Ctrl Pts',(2.62130872380104,5.52533369975343,3.30385695489035));
#9183=CARTESIAN_POINT('Ctrl Pts',(2.46616976756211,5.59373151304768,3.31158204230179));
#9184=CARTESIAN_POINT('Ctrl Pts',(2.31163238862835,5.66186410235693,3.31927717439202));
#9185=CARTESIAN_POINT('Ctrl Pts',(2.15428828368925,5.72358057502088,3.32697230648224));
#9186=CARTESIAN_POINT('Ctrl Pts',(1.99468862981037,5.77867137260852,3.33466743857247));
#9187=CARTESIAN_POINT('Ctrl Pts',(1.83447443939561,5.8339742966456,3.34239220067569));
#9188=CARTESIAN_POINT('Ctrl Pts',(1.67193054273701,5.88261997842296,3.35011696277891));
#9189=CARTESIAN_POINT('Ctrl Pts',(1.50762658312358,5.92443141983761,3.35784172488213));
#9190=CARTESIAN_POINT('Ctrl Pts',(1.34335467408245,5.96623470514556,3.36556498012546));
#9191=CARTESIAN_POINT('Ctrl Pts',(1.17732369411053,6.0012063320846,3.3732882353688));
#9192=CARTESIAN_POINT('Ctrl Pts',(1.01011660531776,6.02921968468237,3.38101149061213));
#9193=CARTESIAN_POINT('Ctrl Pts',(0.842903054773498,6.05723411986177,3.38873504432221));
#9194=CARTESIAN_POINT('Ctrl Pts',(0.674513616365418,6.07828968633435,3.39645859803229));
#9195=CARTESIAN_POINT('Ctrl Pts',(0.505540342874708,6.09231109877246,3.40418215174237));
#9196=CARTESIAN_POINT('Ctrl Pts',(0.336578418395957,6.10633156946887,3.41190518670353));
#9197=CARTESIAN_POINT('Ctrl Pts',(0.167033053178525,6.11331880536751,3.41962822166468));
#9198=CARTESIAN_POINT('Ctrl Pts',(-0.00249950891330681,6.11324948901607,
3.42735125662584));
#9199=CARTESIAN_POINT('Ctrl Pts',(-0.172077125374675,6.11318015424336,3.43507634403325));
#9200=CARTESIAN_POINT('Ctrl Pts',(-0.341641614760534,6.10605051781757,3.44280143144066));
#9201=CARTESIAN_POINT('Ctrl Pts',(-0.510596696319146,6.09188940938753,3.45052651884806));
#9202=CARTESIAN_POINT('Ctrl Pts',(-0.678896626763082,6.07778321298433,3.4582216509586));
#9203=CARTESIAN_POINT('Ctrl Pts',(-0.84659155873096,6.05670003721768,3.46591678306913));
#9204=CARTESIAN_POINT('Ctrl Pts',(-1.01309723036588,6.02871956258748,3.47361191517967));
#9205=CARTESIAN_POINT('Ctrl Pts',(-1.18024402960935,6.00063134955649,3.48133667728178));
#9206=CARTESIAN_POINT('Ctrl Pts',(-1.34625158532875,5.96558263870925,3.48906143938389));
#9207=CARTESIAN_POINT('Ctrl Pts',(-1.51053499781256,5.92369053740009,3.496786201486));
#9208=CARTESIAN_POINT('Ctrl Pts',(-1.67478636373223,5.88180660793185,3.50450945672822));
#9209=CARTESIAN_POINT('Ctrl Pts',(-1.83731395059546,5.83308202993113,3.51223271197044));
#9210=CARTESIAN_POINT('Ctrl Pts',(-1.99754526737113,5.77768452472988,3.51995596721266));
#9211=CARTESIAN_POINT('Ctrl Pts',(-2.15778277631777,5.72228487868108,3.52767952092162));
#9212=CARTESIAN_POINT('Ctrl Pts',(-2.31572353678688,5.66021188921617,3.53540307463057));
#9213=CARTESIAN_POINT('Ctrl Pts',(-2.47081163307323,5.59168270168918,3.54312662833952));
#9214=CARTESIAN_POINT('Ctrl Pts',(-2.62588931293904,5.5231581168935,3.55084966329954));
#9215=CARTESIAN_POINT('Ctrl Pts',(-2.77811442212812,5.44817832990716,3.55857269825957));
#9216=CARTESIAN_POINT('Ctrl Pts',(-2.92695222758717,5.36700812556889,3.5662957332196));
#9217=CARTESIAN_POINT('Ctrl Pts',(-3.07582958765062,5.28581634972659,3.57402082062585));
#9218=CARTESIAN_POINT('Ctrl Pts',(-3.22131756569114,5.19843101907086,3.5817459080321));
#9219=CARTESIAN_POINT('Ctrl Pts',(-3.3629063449619,5.10516272781926,3.58947099543836));
#9220=CARTESIAN_POINT('Ctrl Pts',(-3.50394609057995,5.01225609962381,3.59716612755453));
#9221=CARTESIAN_POINT('Ctrl Pts',(-3.64111658026085,4.91351225267007,3.60486125967069));
#9222=CARTESIAN_POINT('Ctrl Pts',(-3.77394287989615,4.80928068444556,3.61255639178686));
#9223=CARTESIAN_POINT('Ctrl Pts',(-3.9072806251576,4.70464777416891,3.62028115389102));
#9224=CARTESIAN_POINT('Ctrl Pts',(-4.03628786521529,4.59444771647263,3.62800591599518));
#9225=CARTESIAN_POINT('Ctrl Pts',(-4.16050701194673,4.47906317950998,3.63573067809934));
#9226=CARTESIAN_POINT('Ctrl Pts',(-4.28470192740124,4.36370115046775,3.64345393334361));
#9227=CARTESIAN_POINT('Ctrl Pts',(-4.40411038114396,4.24315687568503,3.65117718858788));
#9228=CARTESIAN_POINT('Ctrl Pts',(-4.51830989664579,4.11785153209446,3.65890044383215));
#9229=CARTESIAN_POINT('Ctrl Pts',(-4.63251382541117,3.99254134605335,3.66662399754319));
#9230=CARTESIAN_POINT('Ctrl Pts',(-4.74150819671914,3.86246995459035,3.67434755125424));
#9231=CARTESIAN_POINT('Ctrl Pts',(-4.84490873516459,3.72809400504143,3.68207110496528));
#9232=CARTESIAN_POINT('Ctrl Pts',(-4.94830232876042,3.59372708079137,3.68979413992739));
#9233=CARTESIAN_POINT('Ctrl Pts',(-5.04610264805784,3.45505642822008,3.6975171748895));
#9234=CARTESIAN_POINT('Ctrl Pts',(-5.13796681081408,3.31257039373852,3.70524020985161));
#9235=CARTESIAN_POINT('Ctrl Pts',(-5.22985538706272,3.17004649267641,3.71296529725996));
#9236=CARTESIAN_POINT('Ctrl Pts',(-5.31580448071359,3.02370544893328,3.7206903846683));
#9237=CARTESIAN_POINT('Ctrl Pts',(-5.39551500572968,2.87406391464175,3.72841547207665));
#9238=CARTESIAN_POINT('Ctrl Pts',(-5.47491644001749,2.72500264011901,3.73611060418245));
#9239=CARTESIAN_POINT('Ctrl Pts',(-5.54812748350642,2.57266671663333,3.74380573628825));
#9240=CARTESIAN_POINT('Ctrl Pts',(-5.61489829397816,2.41759026941729,3.75150086839405));
#9241=CARTESIAN_POINT('Ctrl Pts',(-5.68165926002252,2.26253668606663,3.75919486595964));
#9242=CARTESIAN_POINT('Ctrl Pts',(-5.74200723500789,2.10468435679823,3.76688886352523));
#9243=CARTESIAN_POINT('Ctrl Pts',(-5.79572429309673,1.94458362661738,3.77458286109083));
#9244=CARTESIAN_POINT('Ctrl Pts',(-5.84943543818212,1.78450051981731,3.78227601172556));
#9245=CARTESIAN_POINT('Ctrl Pts',(-5.89651701651356,1.62216980979388,3.78996916236029));
#9246=CARTESIAN_POINT('Ctrl Pts',(-5.93680028371151,1.4581590975689,3.79766231299503));
#9247=CARTESIAN_POINT('Ctrl Pts',(-5.97707810581009,1.29417055471316,3.80535442374466));
#9248=CARTESIAN_POINT('Ctrl Pts',(-6.01055937518844,1.12850277583631,3.81304653449429));
#9249=CARTESIAN_POINT('Ctrl Pts',(-6.03712593207551,0.961735952723713,3.82073864524391));
#9250=CARTESIAN_POINT('Ctrl Pts',(-6.06369690572731,0.794941404158186,3.82843203482857));
#9251=CARTESIAN_POINT('Ctrl Pts',(-6.08335081641304,0.627047763945297,3.83612542441322));
#9252=CARTESIAN_POINT('Ctrl Pts',(-6.09602096456547,0.458643611182269,3.84381881399787));
#9253=CARTESIAN_POINT('Ctrl Pts',(-6.10750647886695,0.305984914399864,3.85079288683731));
#9254=CARTESIAN_POINT('Ctrl Pts',(-6.11325373677083,0.152906976817679,3.85776695967675));
#9255=CARTESIAN_POINT('Ctrl Pts',(-6.11324999817629,-0.000149323895543098,
3.86474103251618));
#9256=CARTESIAN_POINT('Origin',(0.,0.,-3.86474103256053));
#9257=CARTESIAN_POINT('',(3.72318137141383,-4.84921626688776,0.984617815426764));
#9258=CARTESIAN_POINT('',(3.72292453512038,-4.84888218750453,1.13013653271955));
#9259=CARTESIAN_POINT('',(3.72292453512038,-4.84888218750453,-3.86474103256053));
#9260=CARTESIAN_POINT('',(-6.11286162838407,-0.000127878758945515,0.364741032560545));
#9261=CARTESIAN_POINT('Ctrl Pts',(-6.11286162838407,-0.000127878758945515,
0.364741032560545));
#9262=CARTESIAN_POINT('Ctrl Pts',(-6.11309733150939,-0.381299532825294,
0.382105164980884));
#9263=CARTESIAN_POINT('Ctrl Pts',(-5.98437783201522,-1.77899319463741,0.445784122936951));
#9264=CARTESIAN_POINT('Ctrl Pts',(-4.93150710543191,-4.0362823909247,0.555777906428748));
#9265=CARTESIAN_POINT('Ctrl Pts',(-2.39941005850561,-5.9036730620091,0.694722383035934));
#9266=CARTESIAN_POINT('Ctrl Pts',(0.717505479260219,-6.33215256902002,0.833666859643123));
#9267=CARTESIAN_POINT('Ctrl Pts',(2.76360922605899,-5.55669049096136,0.930298670440064));
#9268=CARTESIAN_POINT('Ctrl Pts',(3.65355952202664,-4.9027500092498,0.980615655701276));
#9269=CARTESIAN_POINT('Ctrl Pts',(3.72318137141383,-4.84921626688776,0.984617815426764));
#9270=CARTESIAN_POINT('',(-1.5788818818754,5.90584097022478,0.));
#9271=CARTESIAN_POINT('Ctrl Pts',(-1.5788818818754,5.90584097022478,0.));
#9272=CARTESIAN_POINT('Ctrl Pts',(-2.56095449565812,5.64329129027149,0.0463148255357291));
#9273=CARTESIAN_POINT('Ctrl Pts',(-4.39060121268314,4.61907415016922,0.138944476607187));
#9274=CARTESIAN_POINT('Ctrl Pts',(-5.8560845614411,2.28791808963582,0.260524820794035));
#9275=CARTESIAN_POINT('Ctrl Pts',(-6.11246864768786,0.635388098315462,0.335790339445155));
#9276=CARTESIAN_POINT('Ctrl Pts',(-6.11286162838407,-0.000127878758945515,
0.364741032560545));
#9277=CARTESIAN_POINT('',(1.57893355462654,5.90582715566367,0.));
#9278=CARTESIAN_POINT('Origin',(0.,0.,0.));
#9279=CARTESIAN_POINT('',(-6.11324999799714,-0.000156486230825092,0.510258967478569));
#9280=CARTESIAN_POINT('Ctrl Pts',(1.57893355462654,5.90582715566367,-4.44089209850063E-16));
#9281=CARTESIAN_POINT('Ctrl Pts',(1.41553753480309,5.94951137661894,0.00770829872622793));
#9282=CARTESIAN_POINT('Ctrl Pts',(1.25029716222687,5.98641851155851,0.0154165974524564));
#9283=CARTESIAN_POINT('Ctrl Pts',(1.08379079859978,6.01641280726069,0.0231248961786847));
#9284=CARTESIAN_POINT('Ctrl Pts',(0.917316661967493,6.04640129762312,0.0308317029781331));
#9285=CARTESIAN_POINT('Ctrl Pts',(0.749577337565903,6.06947956174143,0.0385385097775815));
#9286=CARTESIAN_POINT('Ctrl Pts',(0.581160905815119,6.08556304412765,0.0462453165770298));
#9287=CARTESIAN_POINT('Ctrl Pts',(0.412739059075133,6.10164704363611,0.053952371168663));
#9288=CARTESIAN_POINT('Ctrl Pts',(0.243640379249169,6.11073577750831,0.0616594257602958));
#9289=CARTESIAN_POINT('Ctrl Pts',(0.0744583243935386,6.11279653844527,0.0693664803519289));
#9290=CARTESIAN_POINT('Ctrl Pts',(-0.0947158388586656,6.11485720325674,
0.0770731754431501));
#9291=CARTESIAN_POINT('Ctrl Pts',(-0.263973049736742,6.10989054820349,0.0847798705343731));
#9292=CARTESIAN_POINT('Ctrl Pts',(-0.432719396652683,6.09791599534304,0.0924865656255944));
#9293=CARTESIAN_POINT('Ctrl Pts',(-0.601506554892215,6.0859385464356,0.100195124581918));
#9294=CARTESIAN_POINT('Ctrl Pts',(-0.769782283310316,6.06694983542276,0.107903683538241));
#9295=CARTESIAN_POINT('Ctrl Pts',(-0.936956493901048,6.04102127881012,0.115612242494564));
#9296=CARTESIAN_POINT('Ctrl Pts',(-1.04775886705582,6.02383593906779,0.12072144338713));
#9297=CARTESIAN_POINT('Ctrl Pts',(-1.15807744082288,6.00360300632556,0.125830644279697));
#9298=CARTESIAN_POINT('Ctrl Pts',(-1.2677424668155,5.98035572523345,0.130939845172263));
#9299=CARTESIAN_POINT('Ctrl Pts',(-1.433546794107,5.94520778478531,0.138664528673874));
#9300=CARTESIAN_POINT('Ctrl Pts',(-1.59791786096845,5.9031540298198,0.146389212175485));
#9301=CARTESIAN_POINT('Ctrl Pts',(-1.76027626943888,5.85433625765982,0.154113895677096));
#9302=CARTESIAN_POINT('Ctrl Pts',(-1.92260304000586,5.80552799835462,0.161837073911484));
#9303=CARTESIAN_POINT('Ctrl Pts',(-2.08291763142132,5.74995844307731,0.16956025214587));
#9304=CARTESIAN_POINT('Ctrl Pts',(-2.24065518922987,5.68781943151128,0.177283430380257));
#9305=CARTESIAN_POINT('Ctrl Pts',(-2.39839890908997,5.62567799247142,0.18500691032226));
#9306=CARTESIAN_POINT('Ctrl Pts',(-2.55356509756797,5.55696669608266,0.192730390264264));
#9307=CARTESIAN_POINT('Ctrl Pts',(-2.7056075559911,5.48192605891979,0.200453870206266));
#9308=CARTESIAN_POINT('Ctrl Pts',(-2.85763984024223,5.40689044322499,0.208176833318864));
#9309=CARTESIAN_POINT('Ctrl Pts',(-3.00654852851301,5.32552647462806,0.215899796431462));
#9310=CARTESIAN_POINT('Ctrl Pts',(-3.15181060588922,5.23812136811512,0.22362275954406));
#9311=CARTESIAN_POINT('Ctrl Pts',(-3.29711136203908,5.15069298834055,0.231347779041556));
#9312=CARTESIAN_POINT('Ctrl Pts',(-3.43876329415943,5.05722041799664,0.239072798539052));
#9313=CARTESIAN_POINT('Ctrl Pts',(-3.57627022355895,4.95803558383616,0.246797818036548));
#9314=CARTESIAN_POINT('Ctrl Pts',(-3.71325172206461,4.85922974712911,0.254493319284182));
#9315=CARTESIAN_POINT('Ctrl Pts',(-3.84611960496846,4.75475543331657,0.262188820531816));
#9316=CARTESIAN_POINT('Ctrl Pts',(-3.97441411774349,4.64498202183617,0.269884321779451));
#9317=CARTESIAN_POINT('Ctrl Pts',(-4.10319053334657,4.53479627691848,0.277608729047571));
#9318=CARTESIAN_POINT('Ctrl Pts',(-4.22740488074,4.419232384039,0.285333136315691));
#9319=CARTESIAN_POINT('Ctrl Pts',(-4.34661622458183,4.29869200556425,0.293057543583811));
#9320=CARTESIAN_POINT('Ctrl Pts',(-4.46580422246066,4.17817523332633,0.300780438129061));
#9321=CARTESIAN_POINT('Ctrl Pts',(-4.57999094901574,4.05268414536578,0.308503332674311));
#9322=CARTESIAN_POINT('Ctrl Pts',(-4.68877217920449,3.92265739187326,0.31622622721956));
#9323=CARTESIAN_POINT('Ctrl Pts',(-4.79755753321199,3.7926257091594,0.323949414534226));
#9324=CARTESIAN_POINT('Ctrl Pts',(-4.90093677434673,3.65805825740187,0.331672601848891));
#9325=CARTESIAN_POINT('Ctrl Pts',(-4.99854534658632,3.51942750751032,0.339395789163556));
#9326=CARTESIAN_POINT('Ctrl Pts',(-5.09614733242753,3.38080611209782,0.347118455335588));
#9327=CARTESIAN_POINT('Ctrl Pts',(-5.18797924609181,3.23812222643966,0.354841121507622));
#9328=CARTESIAN_POINT('Ctrl Pts',(-5.27371923011663,3.09187823893472,0.362563787679654));
#9329=CARTESIAN_POINT('Ctrl Pts',(-5.35948199583808,2.9455953934081,0.370288505816589));
#9330=CARTESIAN_POINT('Ctrl Pts',(-5.43914943511072,2.79575082835339,0.378013223953523));
#9331=CARTESIAN_POINT('Ctrl Pts',(-5.51244464647516,2.64287335717159,0.385737942090457));
#9332=CARTESIAN_POINT('Ctrl Pts',(-5.5854764025778,2.49054539493372,0.393434894189186));
#9333=CARTESIAN_POINT('Ctrl Pts',(-5.65218155735735,2.33520658914986,0.401131846287916));
#9334=CARTESIAN_POINT('Ctrl Pts',(-5.71233296231532,2.17740159138041,0.408828798386645));
#9335=CARTESIAN_POINT('Ctrl Pts',(-5.77255257252794,2.01941765963484,0.416534478005176));
#9336=CARTESIAN_POINT('Ctrl Pts',(-5.82622593648816,1.85890309650743,0.424240157623708));
#9337=CARTESIAN_POINT('Ctrl Pts',(-5.87315835556509,1.69641872571483,0.431945837242239));
#9338=CARTESIAN_POINT('Ctrl Pts',(-5.92008371072521,1.53395881085486,0.439650357059488));
#9339=CARTESIAN_POINT('Ctrl Pts',(-5.96027005446787,1.36952998661637,0.447354876876737));
#9340=CARTESIAN_POINT('Ctrl Pts',(-5.99357258088567,1.20370813744675,0.455059396693986));
#9341=CARTESIAN_POINT('Ctrl Pts',(-6.02687058901322,1.03790878600701,0.462762871207455));
#9342=CARTESIAN_POINT('Ctrl Pts',(-6.05328658190003,0.870717100760946,0.470466345720923));
#9343=CARTESIAN_POINT('Ctrl Pts',(-6.0727268179118,0.7027194016923,0.478169820234392));
#9344=CARTESIAN_POINT('Ctrl Pts',(-6.09216822287533,0.534711600832463,0.48587375796189));
#9345=CARTESIAN_POINT('Ctrl Pts',(-6.1046329952404,0.36589800713182,0.493577695689388));
#9346=CARTESIAN_POINT('Ctrl Pts',(-6.11007916304154,0.196870982792384,0.501281633416886));
#9347=CARTESIAN_POINT('Ctrl Pts',(-6.11219462092914,0.131215724836038,0.504274078091075));
#9348=CARTESIAN_POINT('Ctrl Pts',(-6.11325167937916,0.0655283026476351,
0.507266522765266));
#9349=CARTESIAN_POINT('Ctrl Pts',(-6.11324999799716,-0.000156485372245552,
0.510258967439455));
#9350=CARTESIAN_POINT('Ctrl Pts',(-6.11324999799714,-0.000156486230820938,
0.510258967478568));
#9351=CARTESIAN_POINT('Ctrl Pts',(-6.11324545367516,-0.177683775470678,
0.518346693833848));
#9352=CARTESIAN_POINT('Ctrl Pts',(-6.10550354738073,-0.355172525646239,
0.526434420189127));
#9353=CARTESIAN_POINT('Ctrl Pts',(-6.09006029727742,-0.531969113788794,
0.534522146544405));
#9354=CARTESIAN_POINT('Ctrl Pts',(-6.0816260978578,-0.628525063548642,0.538939189360876));
#9355=CARTESIAN_POINT('Ctrl Pts',(-6.07089572361351,-0.724874613800565,
0.543356232177347));
#9356=CARTESIAN_POINT('Ctrl Pts',(-6.05788157683862,-0.820911909707277,
0.547773274993818));
#9357=CARTESIAN_POINT('Ctrl Pts',(-6.03512235647263,-0.988862526732028,
0.555497826788483));
#9358=CARTESIAN_POINT('Ctrl Pts',(-6.00537031896867,-1.15589589163436,0.563222378583147));
#9359=CARTESIAN_POINT('Ctrl Pts',(-5.96872389633741,-1.32142370638293,0.570946930377813));
#9360=CARTESIAN_POINT('Ctrl Pts',(-5.93208463577432,-1.4869191708662,0.57866997250898));
#9361=CARTESIAN_POINT('Ctrl Pts',(-5.88855374713308,-1.65090936302899,0.586393014640148));
#9362=CARTESIAN_POINT('Ctrl Pts',(-5.83828064561057,-1.81281677661836,0.594116056771316));
#9363=CARTESIAN_POINT('Ctrl Pts',(-5.78800561639362,-1.97473039845849,0.601839395038287));
#9364=CARTESIAN_POINT('Ctrl Pts',(-5.73098794716263,-2.13456077803919,0.60956273330526));
#9365=CARTESIAN_POINT('Ctrl Pts',(-5.66742697942247,-2.29174540370746,0.617286071572231));
#9366=CARTESIAN_POINT('Ctrl Pts',(-5.60387028783684,-2.44891945455645,0.625008890240635));
#9367=CARTESIAN_POINT('Ctrl Pts',(-5.53377129750875,-2.60344781381839,0.632731708909037));
#9368=CARTESIAN_POINT('Ctrl Pts',(-5.45737763912667,-2.7547876263807,0.64045452757744));
#9369=CARTESIAN_POINT('Ctrl Pts',(-5.38096367159313,-2.90616767242888,0.648179399346812));
#9370=CARTESIAN_POINT('Ctrl Pts',(-5.29825183307229,-3.05435719378608,0.655904271116186));
#9371=CARTESIAN_POINT('Ctrl Pts',(-5.20953633294877,-3.19883678204854,0.663629142885557));
#9372=CARTESIAN_POINT('Ctrl Pts',(-5.12115007746558,-3.34278017167597,0.671325345790709));
#9373=CARTESIAN_POINT('Ctrl Pts',(-5.02680483702586,-3.48304086855312,0.679021548695858));
#9374=CARTESIAN_POINT('Ctrl Pts',(-4.92683498489223,-3.61913285113189,0.686717751601009));
#9375=CARTESIAN_POINT('Ctrl Pts',(-4.82649285791936,-3.75573162270607,0.69444261417343));
#9376=CARTESIAN_POINT('Ctrl Pts',(-4.72044858365999,-3.88817893987517,0.702167476745851));
#9377=CARTESIAN_POINT('Ctrl Pts',(-4.60907010354336,-4.01600527179967,0.709892339318273));
#9378=CARTESIAN_POINT('Ctrl Pts',(-4.49771333152076,-4.1438066898806,0.717615696285277));
#9379=CARTESIAN_POINT('Ctrl Pts',(-4.3810246361935,-4.26698868104521,0.72533905325228));
#9380=CARTESIAN_POINT('Ctrl Pts',(-4.25941156418452,-4.38511558449617,0.733062410219284));
#9381=CARTESIAN_POINT('Ctrl Pts',(-4.13779377703128,-4.50324706792674,0.740786066633885));
#9382=CARTESIAN_POINT('Ctrl Pts',(-4.01125145570191,-4.61632284780844,0.748509723048488));
#9383=CARTESIAN_POINT('Ctrl Pts',(-3.8802288134936,-4.72394431777451,0.756233379463089));
#9384=CARTESIAN_POINT('Ctrl Pts',(-3.74921496558499,-4.83155856413826,0.763956517462337));
#9385=CARTESIAN_POINT('Ctrl Pts',(-3.61372164350764,-4.93371903204126,0.771679655461583));
#9386=CARTESIAN_POINT('Ctrl Pts',(-3.47422605934365,-5.03006747977376,0.77940279346083));
#9387=CARTESIAN_POINT('Ctrl Pts',(-3.33469341163632,-5.12644152698949,0.78712798347385));
#9388=CARTESIAN_POINT('Ctrl Pts',(-3.19115663663698,-5.21700028625419,0.794853173486872));
#9389=CARTESIAN_POINT('Ctrl Pts',(-3.04412263002233,-5.30142839014976,0.802578363499892));
#9390=CARTESIAN_POINT('Ctrl Pts',(-2.8976704344348,-5.38552241349502,0.810272985069329));
#9391=CARTESIAN_POINT('Ctrl Pts',(-2.74774892083377,-5.46353408407591,0.817967606638764));
#9392=CARTESIAN_POINT('Ctrl Pts',(-2.59488388816268,-5.53519675977772,0.825662228208201));
#9393=CARTESIAN_POINT('Ctrl Pts',(-2.44142077045098,-5.60713981597963,0.833386955014744));
#9394=CARTESIAN_POINT('Ctrl Pts',(-2.28493669669956,-5.67270954479624,0.841111681821286));
#9395=CARTESIAN_POINT('Ctrl Pts',(-2.12597938050378,-5.73166967263229,0.848836408627829));
#9396=CARTESIAN_POINT('Ctrl Pts',(-1.96705308016936,-5.79061829612747,0.856559628180341));
#9397=CARTESIAN_POINT('Ctrl Pts',(-1.80565479728124,-5.84295978184344,0.864282847732854));
#9398=CARTESIAN_POINT('Ctrl Pts',(-1.64235082019659,-5.88850654630693,0.872006067285365));
#9399=CARTESIAN_POINT('Ctrl Pts',(-1.47904053792382,-5.93405506933701,0.879729585032403));
#9400=CARTESIAN_POINT('Ctrl Pts',(-1.31382471842629,-5.97280825718594,0.88745310277944));
#9401=CARTESIAN_POINT('Ctrl Pts',(-1.14728412070452,-6.00462860707299,0.895176620526479));
#9402=CARTESIAN_POINT('Ctrl Pts',(-0.980754710335357,-6.03644681943033,
0.902899619446772));
#9403=CARTESIAN_POINT('Ctrl Pts',(-0.812901011161869,-6.0613330663143,0.910622618367064));
#9404=CARTESIAN_POINT('Ctrl Pts',(-0.644313448120322,-6.07920107769691,
0.918345617287356));
#9405=CARTESIAN_POINT('Ctrl Pts',(-0.475681076905236,-6.09707383814251,
0.926070668870785));
#9406=CARTESIAN_POINT('Ctrl Pts',(-0.306314767223509,-6.1079246000756,0.933795720454216));
#9407=CARTESIAN_POINT('Ctrl Pts',(-0.13681049800793,-6.11171894397434,0.941520772037645));
#9408=CARTESIAN_POINT('Ctrl Pts',(0.032041197129254,-6.11549868003762,0.949216082963561));
#9409=CARTESIAN_POINT('Ctrl Pts',(0.201029478545488,-6.11227626028111,0.956911393889477));
#9410=CARTESIAN_POINT('Ctrl Pts',(0.369564889392573,-6.10206910441272,0.964606704815394));
#9411=CARTESIAN_POINT('Ctrl Pts',(0.538745432485311,-6.0918228768421,0.972331472418656));
#9412=CARTESIAN_POINT('Ctrl Pts',(0.707529554106069,-6.07453467526001,0.980056240021918));
#9413=CARTESIAN_POINT('Ctrl Pts',(0.875323246504274,-6.05025906690195,0.98778100762518));
#9414=CARTESIAN_POINT('Ctrl Pts',(1.04308420820422,-6.02598819386856,0.995504268395653));
#9415=CARTESIAN_POINT('Ctrl Pts',(1.2098548127118,-5.99473267908254,1.00322752916613));
#9416=CARTESIAN_POINT('Ctrl Pts',(1.37504803630819,-5.95659873252723,1.0109507899366));
#9417=CARTESIAN_POINT('Ctrl Pts',(1.54024764358799,-5.91846331233373,1.01867434916273));
#9418=CARTESIAN_POINT('Ctrl Pts',(1.7038694382931,-5.87344899589648,1.02639790838885));
#9419=CARTESIAN_POINT('Ctrl Pts',(1.86533764988907,-5.82171289350534,1.03412146761498));
#9420=CARTESIAN_POINT('Ctrl Pts',(2.02679501619993,-5.76998026605689,1.04184450807521));
#9421=CARTESIAN_POINT('Ctrl Pts',(2.18609878702905,-5.71152685285931,1.04956754853543));
#9422=CARTESIAN_POINT('Ctrl Pts',(2.34268921528692,-5.64655937745087,1.05729058899566));
#9423=CARTESIAN_POINT('Ctrl Pts',(2.49932125676971,-5.58157463721853,1.06501568182029));
#9424=CARTESIAN_POINT('Ctrl Pts',(2.65323822105741,-5.51007249517287,1.07274077464491));
#9425=CARTESIAN_POINT('Ctrl Pts',(2.80390029083196,-5.43230786329093,1.08046586746954));
#9426=CARTESIAN_POINT('Ctrl Pts',(2.95397750286972,-5.35484510730033,1.08816097212055));
#9427=CARTESIAN_POINT('Ctrl Pts',(3.10082478327173,-5.27116856773365,1.09585607677155));
#9428=CARTESIAN_POINT('Ctrl Pts',(3.24393289200808,-5.18157552821997,1.10355118142256));
#9429=CARTESIAN_POINT('Ctrl Pts',(3.38759122044311,-5.09163802286407,1.11127587208515));
#9430=CARTESIAN_POINT('Ctrl Pts',(3.52753242794613,-4.99570655549234,1.11900056274774));
#9431=CARTESIAN_POINT('Ctrl Pts',(3.66326102202065,-4.89411322376631,1.12672525341033));
#9432=CARTESIAN_POINT('Ctrl Pts',(3.68324059854396,-4.87915844021963,1.1278623465134));
#9433=CARTESIAN_POINT('Ctrl Pts',(3.70312894502161,-4.86408104885361,1.12899943961647));
#9434=CARTESIAN_POINT('Ctrl Pts',(3.72292453512039,-4.84888218750453,1.13013653271955));
#9435=CARTESIAN_POINT('Origin',(0.,0.,0.));
#9436=CARTESIAN_POINT('',(-4.29183622825304,2.82247096572396,18.4117650535551));
#9437=CARTESIAN_POINT('',(-4.29183622819587,2.82247096581089,18.8886809208774));
#9438=CARTESIAN_POINT('',(-4.29183622825304,2.82247096572397,0.));
#9439=CARTESIAN_POINT('',(4.95630975100502,1.34951628911715,20.));
#9440=CARTESIAN_POINT('Ctrl Pts',(4.95630975100503,1.34951628911712,20.));
#9441=CARTESIAN_POINT('Ctrl Pts',(5.02530589382568,1.09611715773841,19.985760168123));
#9442=CARTESIAN_POINT('Ctrl Pts',(5.07476845806476,0.83779585568772,19.9717441009936));
#9443=CARTESIAN_POINT('Ctrl Pts',(5.1218150352685,0.421484983818935,19.9491973439681));
#9444=CARTESIAN_POINT('Ctrl Pts',(5.13226903371038,0.265428195636579,19.940758950191));
#9445=CARTESIAN_POINT('Ctrl Pts',(5.14045498932613,-0.119762154763499,19.9198304701504));
#9446=CARTESIAN_POINT('Ctrl Pts',(5.1300101780035,-0.348729313788184,19.9072951957962));
#9447=CARTESIAN_POINT('Ctrl Pts',(5.0889160140276,-0.712747505217411,19.8871692238277));
#9448=CARTESIAN_POINT('Ctrl Pts',(5.06803371909913,-0.84859285855697,19.8796172623197));
#9449=CARTESIAN_POINT('Ctrl Pts',(5.02581032745821,-1.06505691087385,19.8675528749467));
#9450=CARTESIAN_POINT('Ctrl Pts',(5.00790987497494,-1.14627872475244,19.8630201081034));
#9451=CARTESIAN_POINT('Ctrl Pts',(4.94234733308433,-1.41279905148079,19.8481473500308));
#9452=CARTESIAN_POINT('Ctrl Pts',(4.88630680506449,-1.59587177542111,19.837910809985));
#9453=CARTESIAN_POINT('Ctrl Pts',(4.74025411427273,-1.99240401217042,19.8152538320208));
#9454=CARTESIAN_POINT('Ctrl Pts',(4.64576155677645,-2.20376481251868,19.8028440551837));
#9455=CARTESIAN_POINT('Ctrl Pts',(4.41903586086519,-2.63097371493999,19.7766204234566));
#9456=CARTESIAN_POINT('Ctrl Pts',(4.2844518484464,-2.84488454292749,19.7628135131264));
#9457=CARTESIAN_POINT('Ctrl Pts',(4.03429872523108,-3.18422073988682,19.7397008754151));
#9458=CARTESIAN_POINT('Ctrl Pts',(3.9272322427042,-3.3153697839732,19.7304310371072));
#9459=CARTESIAN_POINT('Ctrl Pts',(3.66663412093714,-3.60420810666249,19.7093400446914));
#9460=CARTESIAN_POINT('Ctrl Pts',(3.50905321579256,-3.75780135782271,19.6975958355295));
#9461=CARTESIAN_POINT('Ctrl Pts',(3.17877746362949,-4.04077194245563,19.6742682237264));
#9462=CARTESIAN_POINT('Ctrl Pts',(3.00681386490056,-4.17031553658563,19.6627090710648));
#9463=CARTESIAN_POINT('Ctrl Pts',(2.61835356823536,-4.42640047801557,19.6374696580365));
#9464=CARTESIAN_POINT('Ctrl Pts',(2.3996891680016,-4.54865736647821,19.6237791038255));
#9465=CARTESIAN_POINT('Ctrl Pts',(2.02558012934287,-4.72331379219015,19.60114309389));
#9466=CARTESIAN_POINT('Ctrl Pts',(1.87497726074543,-4.78509454034322,19.5922303821311));
#9467=CARTESIAN_POINT('Ctrl Pts',(1.54278421990625,-4.90327212686748,19.5731008180843));
#9468=CARTESIAN_POINT('Ctrl Pts',(1.36047834009044,-4.95695086501791,19.5629341636872));
#9469=CARTESIAN_POINT('Ctrl Pts',(0.961109557259161,-5.05084406473322,19.5409398437521));
#9470=CARTESIAN_POINT('Ctrl Pts',(0.743582581930314,-5.08741977359763,19.529126018642));
#9471=CARTESIAN_POINT('Ctrl Pts',(0.195183186632527,-5.14369690873679,19.4992824241404));
#9472=CARTESIAN_POINT('Ctrl Pts',(-0.136505696197581,-5.14558740425137,
19.4811420150829));
#9473=CARTESIAN_POINT('Ctrl Pts',(-0.592490824100446,-5.10404490011886,
19.4560588194645));
#9474=CARTESIAN_POINT('Ctrl Pts',(-0.718460756107112,-5.08784190893735,
19.4491224236343));
#9475=CARTESIAN_POINT('Ctrl Pts',(-1.02388383251126,-5.03698596369529,19.4323493632291));
#9476=CARTESIAN_POINT('Ctrl Pts',(-1.20233897843037,-4.99739421619772,19.4225706137207));
#9477=CARTESIAN_POINT('Ctrl Pts',(-1.58954298069361,-4.88954350859193,19.4010211332803));
#9478=CARTESIAN_POINT('Ctrl Pts',(-1.7967906699977,-4.81724231554643,19.3892618014552));
#9479=CARTESIAN_POINT('Ctrl Pts',(-2.28769513182071,-4.60988248520833,19.3604080865111));
#9480=CARTESIAN_POINT('Ctrl Pts',(-2.56482071175491,-4.46164219223895,19.3432292750671));
#9481=CARTESIAN_POINT('Ctrl Pts',(-2.9406328057709,-4.21396527559979,19.3185687856875));
#9482=CARTESIAN_POINT('Ctrl Pts',(-3.05154649102943,-4.13435487165146,19.3111085090113));
#9483=CARTESIAN_POINT('Ctrl Pts',(-3.30622214787486,-3.93571842684582,19.2936094306021));
#9484=CARTESIAN_POINT('Ctrl Pts',(-3.4469307845396,-3.8130899551909,19.2836268860308));
#9485=CARTESIAN_POINT('Ctrl Pts',(-3.73922808706123,-3.52892087326279,19.2617703579193));
#9486=CARTESIAN_POINT('Ctrl Pts',(-3.88767255959531,-3.36468553894342,19.2499080068004));
#9487=CARTESIAN_POINT('Ctrl Pts',(-4.21225799055328,-2.95531055366526,19.2216103869056));
#9488=CARTESIAN_POINT('Ctrl Pts',(-4.378309695436,-2.70321545620731,19.2051098800644));
#9489=CARTESIAN_POINT('Ctrl Pts',(-4.58932323689831,-2.31189330743614,19.1807408091588));
#9490=CARTESIAN_POINT('Ctrl Pts',(-4.65203482714063,-2.18295945966545,19.1729009130736));
#9491=CARTESIAN_POINT('Ctrl Pts',(-4.79073388762263,-1.86458288424742,19.1540783763617));
#9492=CARTESIAN_POINT('Ctrl Pts',(-4.86098627431131,-1.67290645695063,19.143172468624));
#9493=CARTESIAN_POINT('Ctrl Pts',(-4.98416476824743,-1.26277320776459,19.120210720972));
#9494=CARTESIAN_POINT('Ctrl Pts',(-5.03453675361378,-1.04399777864826,19.1081697792498));
#9495=CARTESIAN_POINT('Ctrl Pts',(-5.11087974117963,-0.573445011447198,
19.0823187470383));
#9496=CARTESIAN_POINT('Ctrl Pts',(-5.13288301479651,-0.321617695963115,
19.0685066801584));
#9497=CARTESIAN_POINT('Ctrl Pts',(-5.13852726620075,0.0973098189321237,
19.0455334154845));
#9498=CARTESIAN_POINT('Ctrl Pts',(-5.13267227472482,0.263834269357301,19.0364080184376));
#9499=CARTESIAN_POINT('Ctrl Pts',(-5.10298853574141,0.617370407419794,19.0171609458188));
#9500=CARTESIAN_POINT('Ctrl Pts',(-5.07693775185344,0.803955134054031,19.0070812083906));
#9501=CARTESIAN_POINT('Ctrl Pts',(-4.99743022062426,1.20931325277453,18.984934710332));
#9502=CARTESIAN_POINT('Ctrl Pts',(-4.93972011366581,1.42685321071505,18.9728814821261));
#9503=CARTESIAN_POINT('Ctrl Pts',(-4.76694952668741,1.93970962557575,18.9435787367963));
#9504=CARTESIAN_POINT('Ctrl Pts',(-4.63847493686506,2.22953403684096,18.9262471762037));
#9505=CARTESIAN_POINT('Ctrl Pts',(-4.42388634110982,2.61356094779722,18.902142851062));
#9506=CARTESIAN_POINT('Ctrl Pts',(-4.35973477672137,2.71922474860137,18.8953862161405));
#9507=CARTESIAN_POINT('Ctrl Pts',(-4.29183622819587,2.8224709658109,18.8886809208774));
#9508=CARTESIAN_POINT('',(-2.03116440553747,4.71811103304888,20.));
#9509=CARTESIAN_POINT('Origin',(0.,0.,20.));
#9510=CARTESIAN_POINT('Ctrl Pts',(-2.03116440553748,4.71811103304888,20.));
#9511=CARTESIAN_POINT('Ctrl Pts',(-1.75876294038136,4.83538088027497,19.9838242100236));
#9512=CARTESIAN_POINT('Ctrl Pts',(-1.47671310578932,4.92884170022616,19.9675020813374));
#9513=CARTESIAN_POINT('Ctrl Pts',(-1.02673667725821,5.03582637935673,19.9422943163514));
#9514=CARTESIAN_POINT('Ctrl Pts',(-0.863532856038434,5.06636440626909,19.9333064352754));
#9515=CARTESIAN_POINT('Ctrl Pts',(-0.431451545577099,5.12572502375573,19.9097964073362));
#9516=CARTESIAN_POINT('Ctrl Pts',(-0.161285469164626,5.14132214210612,19.8953967529817));
#9517=CARTESIAN_POINT('Ctrl Pts',(0.211096044340629,5.13342946063892,19.8753425674653));
#9518=CARTESIAN_POINT('Ctrl Pts',(0.313252013380761,5.12820946562538,19.8698131775709));
#9519=CARTESIAN_POINT('Ctrl Pts',(0.664459217167201,5.09972949640327,19.8506286802133));
#9520=CARTESIAN_POINT('Ctrl Pts',(0.9119239339857,5.06133791149605,19.8368700328516));
#9521=CARTESIAN_POINT('Ctrl Pts',(1.30420074646597,4.9707664040537,19.814850744872));
#9522=CARTESIAN_POINT('Ctrl Pts',(1.45119646922876,4.92985683047897,19.8065459912916));
#9523=CARTESIAN_POINT('Ctrl Pts',(1.83322012950886,4.80496724601604,19.7847711270967));
#9524=CARTESIAN_POINT('Ctrl Pts',(2.06432719374341,4.71030387023003,19.7714126359105));
#9525=CARTESIAN_POINT('Ctrl Pts',(2.44210240830701,4.52239937182995,19.7487917799261));
#9526=CARTESIAN_POINT('Ctrl Pts',(2.5925895512669,4.43784154113219,19.7395456576355));
#9527=CARTESIAN_POINT('Ctrl Pts',(2.84885340339452,4.27635801571134,19.7231141398198));
#9528=CARTESIAN_POINT('Ctrl Pts',(2.95648431131262,4.20266619585462,19.7159828904466));
#9529=CARTESIAN_POINT('Ctrl Pts',(3.24673701093696,3.98726546220093,19.6961752000313));
#9530=CARTESIAN_POINT('Ctrl Pts',(3.42278213919766,3.83720630644497,19.6835004441861));
#9531=CARTESIAN_POINT('Ctrl Pts',(3.70898082723071,3.55783425299693,19.6617256398255));
#9532=CARTESIAN_POINT('Ctrl Pts',(3.82394472492539,3.43397319677323,19.6525909097226));
#9533=CARTESIAN_POINT('Ctrl Pts',(4.13971273079861,3.05820548543407,19.6261636191148));
#9534=CARTESIAN_POINT('Ctrl Pts',(4.32319237180496,2.79281963364292,19.609072260082));
#9535=CARTESIAN_POINT('Ctrl Pts',(4.57204856975284,2.34894135533897,19.5814745437388));
#9536=CARTESIAN_POINT('Ctrl Pts',(4.65450356788183,2.18099704756942,19.571220452595));
#9537=CARTESIAN_POINT('Ctrl Pts',(4.81576975519437,1.80149005543778,19.5486093361489));
#9538=CARTESIAN_POINT('Ctrl Pts',(4.89017290886852,1.58846379613654,19.536282487004));
#9539=CARTESIAN_POINT('Ctrl Pts',(5.03514514724615,1.06509540907264,19.5068128983632));
#9540=CARTESIAN_POINT('Ctrl Pts',(5.09136502481458,0.751745249377349,19.489851744901));
#9541=CARTESIAN_POINT('Ctrl Pts',(5.12964176007384,0.30159365592701,19.4656042644915));
#9542=CARTESIAN_POINT('Ctrl Pts',(5.13576651018031,0.167585179481134,19.4583926493008));
#9543=CARTESIAN_POINT('Ctrl Pts',(5.13786573095127,-0.154375327316645,19.4409097676649));
#9544=CARTESIAN_POINT('Ctrl Pts',(5.12878318906439,-0.342165695784814,19.4306008150461));
#9545=CARTESIAN_POINT('Ctrl Pts',(5.08672347758837,-0.74838099282315,19.4082085618613));
#9546=CARTESIAN_POINT('Ctrl Pts',(5.04991038522345,-0.966042645175719,19.3961551733762));
#9547=CARTESIAN_POINT('Ctrl Pts',(4.93085103721109,-1.4701681469757,19.3680573869256));
#9548=CARTESIAN_POINT('Ctrl Pts',(4.83746124673004,-1.75318535202099,19.352157458766));
#9549=CARTESIAN_POINT('Ctrl Pts',(4.66261804777703,-2.16042253749514,19.3283824011532));
#9550=CARTESIAN_POINT('Ctrl Pts',(4.59946231667175,-2.29180666574483,19.3205550036784));
#9551=CARTESIAN_POINT('Ctrl Pts',(4.43450863255362,-2.60059698282352,19.3015524206627));
#9552=CARTESIAN_POINT('Ctrl Pts',(4.32753760437117,-2.77495727721709,19.2903305536088));
#9553=CARTESIAN_POINT('Ctrl Pts',(4.08216582852423,-3.12606590849171,19.2668479553779));
#9554=CARTESIAN_POINT('Ctrl Pts',(3.94199337408599,-3.30106921498769,19.2546185202404));
#9555=CARTESIAN_POINT('Ctrl Pts',(3.62194279043492,-3.65107894683408,19.2289222747411));
#9556=CARTESIAN_POINT('Ctrl Pts',(3.43976506524457,-3.82320106591323,19.2155164664277));
#9557=CARTESIAN_POINT('Ctrl Pts',(3.11278065081963,-4.08977208511344,19.1928968803583));
#9558=CARTESIAN_POINT('Ctrl Pts',(2.97445016187949,-4.19145359471505,19.1836997073477));
#9559=CARTESIAN_POINT('Ctrl Pts',(2.68287896765122,-4.38406208132611,19.1647424728127));
#9560=CARTESIAN_POINT('Ctrl Pts',(2.52947310941184,-4.47432720799941,19.1549898266571));
#9561=CARTESIAN_POINT('Ctrl Pts',(2.16558623509264,-4.66373545881771,19.1324944427109));
#9562=CARTESIAN_POINT('Ctrl Pts',(1.95242925752933,-4.75691244497512,19.1197834178669));
#9563=CARTESIAN_POINT('Ctrl Pts',(1.43531652543014,-4.94232151271111,19.0899739422836));
#9564=CARTESIAN_POINT('Ctrl Pts',(1.12767482714869,-5.02145684046532,19.0730491469159));
#9565=CARTESIAN_POINT('Ctrl Pts',(0.681967033058751,-5.0930536087937,19.0488210854185));
#9566=CARTESIAN_POINT('Ctrl Pts',(0.54844774318353,-5.10915631787797,19.0415915442061));
#9567=CARTESIAN_POINT('Ctrl Pts',(0.226770606839126,-5.13519528115496,19.0240675179371));
#9568=CARTESIAN_POINT('Ctrl Pts',(0.0383985421090806,-5.14005635979088,
19.0137351640574));
#9569=CARTESIAN_POINT('Ctrl Pts',(-0.370040583681346,-5.12813928827051,
18.9913306270689));
#9570=CARTESIAN_POINT('Ctrl Pts',(-0.589631825340411,-5.10755130569912,
18.9792882671527));
#9571=CARTESIAN_POINT('Ctrl Pts',(-1.10031682802839,-5.02628904669437,18.9512386610511));
#9572=CARTESIAN_POINT('Ctrl Pts',(-1.38881776421128,-4.95433827868492,18.9353747119186));
#9573=CARTESIAN_POINT('Ctrl Pts',(-1.80772373185749,-4.8103742465423,18.9116122951975));
#9574=CARTESIAN_POINT('Ctrl Pts',(-1.94386254984276,-4.75699092412569,18.9037607272593));
#9575=CARTESIAN_POINT('Ctrl Pts',(-2.26490235117464,-4.61501774531452,18.884707078263));
#9576=CARTESIAN_POINT('Ctrl Pts',(-2.44713993640201,-4.52102595707778,18.8734581563373));
#9577=CARTESIAN_POINT('Ctrl Pts',(-2.81553184456781,-4.30220698923688,18.8499686921729));
#9578=CARTESIAN_POINT('Ctrl Pts',(-3.00013058062337,-4.17557479132149,18.8377591677673));
#9579=CARTESIAN_POINT('Ctrl Pts',(-3.36346396170165,-3.88976417072007,18.8127133070388));
#9580=CARTESIAN_POINT('Ctrl Pts',(-3.54052077378501,-3.72932472488589,18.7999225102669));
#9581=CARTESIAN_POINT('Ctrl Pts',(-3.83275328361216,-3.4248820219363,18.7772977795739));
#9582=CARTESIAN_POINT('Ctrl Pts',(-3.95255484781583,-3.28589867451037,18.7674765495375));
#9583=CARTESIAN_POINT('Ctrl Pts',(-4.1730526470859,-3.00054246384596,18.7479125947867));
#9584=CARTESIAN_POINT('Ctrl Pts',(-4.27410457203303,-2.8547595135527,18.7381935793223));
#9585=CARTESIAN_POINT('Ctrl Pts',(-4.42859745019339,-2.60523182163145,18.7221001709323));
#9586=CARTESIAN_POINT('Ctrl Pts',(-4.48640740096312,-2.50436761210014,18.7157299162025));
#9587=CARTESIAN_POINT('Ctrl Pts',(-4.57860830881648,-2.33004387857943,18.7049509495119));
#9588=CARTESIAN_POINT('Ctrl Pts',(-4.61477230822775,-2.25757286804229,18.7005344319853));
#9589=CARTESIAN_POINT('Ctrl Pts',(-4.72247152053522,-2.02833632249747,18.6867574872509));
#9590=CARTESIAN_POINT('Ctrl Pts',(-4.78784393728745,-1.86880652217347,18.6774498202014));
#9591=CARTESIAN_POINT('Ctrl Pts',(-4.94616864022449,-1.41923769466512,18.6518102469528));
#9592=CARTESIAN_POINT('Ctrl Pts',(-5.02154789416998,-1.12377448705335,18.6356373139083));
#9593=CARTESIAN_POINT('Ctrl Pts',(-5.10090104584609,-0.635126718511599,
18.6087926659858));
#9594=CARTESIAN_POINT('Ctrl Pts',(-5.12096401959124,-0.445311952233824,
18.5983302540382));
#9595=CARTESIAN_POINT('Ctrl Pts',(-5.14137951378069,-0.034284679017604,
18.5757641295428));
#9596=CARTESIAN_POINT('Ctrl Pts',(-5.13810193422646,0.18673673320556,18.563688843334));
#9597=CARTESIAN_POINT('Ctrl Pts',(-5.0950259670139,0.728873128613459,18.5341740124312));
#9598=CARTESIAN_POINT('Ctrl Pts',(-5.03912318960092,1.04775328274904,18.5169319461479));
#9599=CARTESIAN_POINT('Ctrl Pts',(-4.91889111265508,1.48592026110536,18.4925420780072));
#9600=CARTESIAN_POINT('Ctrl Pts',(-4.87929476383411,1.61118918792427,18.4854771887509));
#9601=CARTESIAN_POINT('Ctrl Pts',(-4.77302687055334,1.9073607047389,18.4683891135196));
#9602=CARTESIAN_POINT('Ctrl Pts',(-4.70191931669328,2.07647863647284,18.4583310561176));
#9603=CARTESIAN_POINT('Ctrl Pts',(-4.5246343402553,2.4420477874444,18.4360531501995));
#9604=CARTESIAN_POINT('Ctrl Pts',(-4.41438337869704,2.63612143528974,18.4238641311583));
#9605=CARTESIAN_POINT('Ctrl Pts',(-4.29185896137503,2.82243639764222,18.4117672979533));
#9606=CARTESIAN_POINT('Ctrl Pts',(-4.2918475948598,2.82245368171457,18.4117661757578));
#9607=CARTESIAN_POINT('Ctrl Pts',(-4.29183622825304,2.82247096572396,18.4117650535551));
#9608=CARTESIAN_POINT('Origin',(0.,0.,0.));
#9609=CARTESIAN_POINT('',(-4.2921400227931,2.82267100337914,16.6620149077712));
#9610=CARTESIAN_POINT('',(-4.29183622825303,2.82247096572397,17.1389378634518));
#9611=CARTESIAN_POINT('',(-4.29183622825304,2.82247096572397,0.));
#9612=CARTESIAN_POINT('',(-5.1367499996765,-5.76498924387363E-5,17.3009584946969));
#9613=CARTESIAN_POINT('Ctrl Pts',(-4.29183622825303,2.82247096572397,17.1389378634518));
#9614=CARTESIAN_POINT('Ctrl Pts',(-4.37359531714591,2.69814847526767,17.1470045559175));
#9615=CARTESIAN_POINT('Ctrl Pts',(-4.44995155153085,2.57026701404298,17.1550712483833));
#9616=CARTESIAN_POINT('Ctrl Pts',(-4.52061197112331,2.43931711120892,17.1631379408491));
#9617=CARTESIAN_POINT('Ctrl Pts',(-4.59127033350124,2.30837102086345,17.1712043984604));
#9618=CARTESIAN_POINT('Ctrl Pts',(-4.65623305756608,2.1743569599479,17.1792708560717));
#9619=CARTESIAN_POINT('Ctrl Pts',(-4.71525317845947,2.03778998562851,17.187337313683));
#9620=CARTESIAN_POINT('Ctrl Pts',(-4.77428652497719,1.90119240846606,17.1954055788802));
#9621=CARTESIAN_POINT('Ctrl Pts',(-4.82737447737193,1.76204107923804,17.2034738440774));
#9622=CARTESIAN_POINT('Ctrl Pts',(-4.87431801938217,1.62087149658026,17.2115421092746));
#9623=CARTESIAN_POINT('Ctrl Pts',(-4.892875195019,1.56506597727393,17.2147315621351));
#9624=CARTESIAN_POINT('Ctrl Pts',(-4.91047273029335,1.50894526372987,17.2179210149957));
#9625=CARTESIAN_POINT('Ctrl Pts',(-4.92710046533172,1.45254313775113,17.2211104678562));
#9626=CARTESIAN_POINT('Ctrl Pts',(-4.96940617618376,1.30904000713293,17.2292253476149));
#9627=CARTESIAN_POINT('Ctrl Pts',(-5.00544537854101,1.16366362598839,17.2373402273735));
#9628=CARTESIAN_POINT('Ctrl Pts',(-5.03507358990828,1.0169732084515,17.2454551071321));
#9629=CARTESIAN_POINT('Ctrl Pts',(-5.06469490923402,0.870316913678134,17.2535680992274));
#9630=CARTESIAN_POINT('Ctrl Pts',(-5.08790814974416,0.722347508930372,17.2616810913227));
#9631=CARTESIAN_POINT('Ctrl Pts',(-5.10461981860422,0.573634962334952,17.269794083418));
#9632=CARTESIAN_POINT('Ctrl Pts',(-5.12132933420445,0.424941577006755,17.277906030173));
#9633=CARTESIAN_POINT('Ctrl Pts',(-5.13153891306429,0.275505561659813,17.286017976928));
#9634=CARTESIAN_POINT('Ctrl Pts',(-5.13520681056804,0.125903038865496,17.2941299236831));
#9635=CARTESIAN_POINT('Ctrl Pts',(-5.13623601269556,0.083924975251689,17.296406114021));
#9636=CARTESIAN_POINT('Ctrl Pts',(-5.13675047094801,0.0419338240484392,
17.298682304359));
#9637=CARTESIAN_POINT('Ctrl Pts',(-5.1367499996765,-5.76498924387363E-5,
17.3009584946969));
#9638=CARTESIAN_POINT('Ctrl Pts',(-4.29183622819587,2.82247096581089,18.8886809208774));
#9639=CARTESIAN_POINT('Ctrl Pts',(-4.28567102649408,2.83184574285497,18.8880720787348));
#9640=CARTESIAN_POINT('Ctrl Pts',(-4.27947493157269,2.84120058855997,18.8874636785894));
#9641=CARTESIAN_POINT('Ctrl Pts',(-4.16840366187836,3.00770793814683,18.8766188854153));
#9642=CARTESIAN_POINT('Ctrl Pts',(-4.0549659063518,3.15897928524874,18.8665078330849));
#9643=CARTESIAN_POINT('Ctrl Pts',(-3.78354837421278,3.48213842336234,18.843881669676));
#9644=CARTESIAN_POINT('Ctrl Pts',(-3.62167446121573,3.65020511107423,18.8313769842141));
#9645=CARTESIAN_POINT('Ctrl Pts',(-3.24892560801987,3.98792386684946,18.8041072757814));
#9646=CARTESIAN_POINT('Ctrl Pts',(-3.03493035403199,4.15310079458692,18.7893320173679));
#9647=CARTESIAN_POINT('Ctrl Pts',(-2.67675336823147,4.38704061934109,18.7658765148313));
#9648=CARTESIAN_POINT('Ctrl Pts',(-2.54063689495991,4.46724746478873,18.757230077586));
#9649=CARTESIAN_POINT('Ctrl Pts',(-2.1976262844609,4.64861099894477,18.7361942724354));
#9650=CARTESIAN_POINT('Ctrl Pts',(-1.9872115651427,4.7423770187691,18.7239105215631));
#9651=CARTESIAN_POINT('Ctrl Pts',(-1.57763255577205,4.8928322999547,18.7005036795224));
#9652=CARTESIAN_POINT('Ctrl Pts',(-1.37994470544255,4.95221995041138,18.6894146110521));
#9653=CARTESIAN_POINT('Ctrl Pts',(-1.01465516975105,5.03837928221641,18.6690532135946));
#9654=CARTESIAN_POINT('Ctrl Pts',(-0.848270549384174,5.06904589571288,18.6598277199854));
#9655=CARTESIAN_POINT('Ctrl Pts',(-0.43721538511567,5.12400015846466,18.6371130870805));
#9656=CARTESIAN_POINT('Ctrl Pts',(-0.191728009324919,5.1390444046113,18.6236045150092));
#9657=CARTESIAN_POINT('Ctrl Pts',(0.22726986279079,5.13464815936065,18.6008770042723));
#9658=CARTESIAN_POINT('Ctrl Pts',(0.400446477283491,5.12405192758401,18.5915844507442));
#9659=CARTESIAN_POINT('Ctrl Pts',(0.818354410610287,5.0771619706189,18.5690376532882));
#9660=CARTESIAN_POINT('Ctrl Pts',(1.06163820392017,5.03191801728217,18.5557985573287));
#9661=CARTESIAN_POINT('Ctrl Pts',(1.51725978741158,4.91265989925699,18.5302814731074));
#9662=CARTESIAN_POINT('Ctrl Pts',(1.72986335144501,4.84188739353601,18.5180600379684));
#9663=CARTESIAN_POINT('Ctrl Pts',(2.12661365437589,4.68033709088422,18.4945758632146));
#9664=CARTESIAN_POINT('Ctrl Pts',(2.31128519370989,4.59194986319994,18.4833443115668));
#9665=CARTESIAN_POINT('Ctrl Pts',(2.61774314215245,4.42209087481972,18.4643256788713));
#9666=CARTESIAN_POINT('Ctrl Pts',(2.74222388080037,4.34599542791154,18.4564918082633));
#9667=CARTESIAN_POINT('Ctrl Pts',(3.11014098228951,4.0989778829039,18.4327186936835));
#9668=CARTESIAN_POINT('Ctrl Pts',(3.3421236306895,3.91213527254424,18.4168269690776));
#9669=CARTESIAN_POINT('Ctrl Pts',(3.71579414655474,3.55355194399674,18.3887347512914));
#9670=CARTESIAN_POINT('Ctrl Pts',(3.86494412048878,3.39073164066515,18.3766783567414));
#9671=CARTESIAN_POINT('Ctrl Pts',(4.12085248980146,3.07246633493118,18.3542860162302));
#9672=CARTESIAN_POINT('Ctrl Pts',(4.2304274473692,2.91975339389395,18.3439800040664));
#9673=CARTESIAN_POINT('Ctrl Pts',(4.40353646433848,2.64822148498378,18.3264943475812));
#9674=CARTESIAN_POINT('Ctrl Pts',(4.47121732212872,2.53227703200014,18.3192771841691));
#9675=CARTESIAN_POINT('Ctrl Pts',(4.6834470684315,2.13360932565539,18.2950371532842));
#9676=CARTESIAN_POINT('Ctrl Pts',(4.8063163666821,1.84018594964896,18.278088669385));
#9677=CARTESIAN_POINT('Ctrl Pts',(4.96722982386203,1.32715383088493,18.2489121923307));
#9678=CARTESIAN_POINT('Ctrl Pts',(5.01955921314604,1.11298309318419,18.2368698918193));
#9679=CARTESIAN_POINT('Ctrl Pts',(5.08960228793428,0.71763845862642,18.2148542208892));
#9680=CARTESIAN_POINT('Ctrl Pts',(5.11175491925199,0.537605427652224,18.2049101328354));
#9681=CARTESIAN_POINT('Ctrl Pts',(5.13337913338866,0.227019551725915,18.1880014756885));
#9682=CARTESIAN_POINT('Ctrl Pts',(5.13748164677116,0.0969655137992032,18.181003285117));
#9683=CARTESIAN_POINT('Ctrl Pts',(5.13454497795426,-0.358674369149742,18.1565426970965));
#9684=CARTESIAN_POINT('Ctrl Pts',(5.10149933775087,-0.683300915123357,18.1391672353028));
#9685=CARTESIAN_POINT('Ctrl Pts',(4.99443205170792,-1.22129784171954,18.1093955110344));
#9686=CARTESIAN_POINT('Ctrl Pts',(4.93671781388726,-1.43691814050995,18.0972005153241));
#9687=CARTESIAN_POINT('Ctrl Pts',(4.80525064743935,-1.82500803399851,18.0747317140419));
#9688=CARTESIAN_POINT('Ctrl Pts',(4.73571723963228,-1.99851753693678,18.0644869468147));
#9689=CARTESIAN_POINT('Ctrl Pts',(4.58361934618337,-2.32524720069935,18.0449414942034));
#9690=CARTESIAN_POINT('Ctrl Pts',(4.50241766359103,-2.47882598243922,18.0356375836716));
#9691=CARTESIAN_POINT('Ctrl Pts',(4.28772277484999,-2.83939527562957,18.0131382829671));
#9692=CARTESIAN_POINT('Ctrl Pts',(4.14682833088724,-3.04147068432655,17.9999575263177));
#9693=CARTESIAN_POINT('Ctrl Pts',(3.85106930918717,-3.40670141279893,17.9744949527394));
#9694=CARTESIAN_POINT('Ctrl Pts',(3.69891246869681,-3.57132917596064,17.9622680148383));
#9695=CARTESIAN_POINT('Ctrl Pts',(3.38824820635048,-3.86623337151898,17.938785663064));
#9696=CARTESIAN_POINT('Ctrl Pts',(3.23172262745006,-3.99799413733433,17.92756151357));
#9697=CARTESIAN_POINT('Ctrl Pts',(2.95081342955522,-4.20715581820003,17.9085513872989));
#9698=CARTESIAN_POINT('Ctrl Pts',(2.83020990250404,-4.28921590616174,17.9007187680953));
#9699=CARTESIAN_POINT('Ctrl Pts',(2.4535433097544,-4.5226918201582,17.8769451451976));
#9700=CARTESIAN_POINT('Ctrl Pts',(2.18768863766049,-4.65710539250038,17.8610517034469));
#9701=CARTESIAN_POINT('Ctrl Pts',(1.70697725034928,-4.84985380145168,17.8329582245202));
#9702=CARTESIAN_POINT('Ctrl Pts',(1.49717687702778,-4.91866965582099,17.8209023604202));
#9703=CARTESIAN_POINT('Ctrl Pts',(1.10173955059713,-5.02072204643755,17.798509766197));
#9704=CARTESIAN_POINT('Ctrl Pts',(0.917430856515096,-5.05764788961084,17.7882029656857));
#9705=CARTESIAN_POINT('Ctrl Pts',(0.598698321023235,-5.10350523942269,17.7707175490202));
#9706=CARTESIAN_POINT('Ctrl Pts',(0.465185571669131,-5.11740253197068,17.7635013785421));
#9707=CARTESIAN_POINT('Ctrl Pts',(0.0144697610531822,-5.14653075311769,
17.7392603899139));
#9708=CARTESIAN_POINT('Ctrl Pts',(-0.303551289442379,-5.1375909656368,17.7223100080063));
#9709=CARTESIAN_POINT('Ctrl Pts',(-0.849440783413805,-5.07135818226045,
17.692470557552));
#9710=CARTESIAN_POINT('Ctrl Pts',(-1.07800685676574,-5.02773515923622,17.6797561353485));
#9711=CARTESIAN_POINT('Ctrl Pts',(-1.47458459914182,-4.9237515809517,17.657274299014));
#9712=CARTESIAN_POINT('Ctrl Pts',(-1.64389383976998,-4.86984025617014,17.6475385489272));
#9713=CARTESIAN_POINT('Ctrl Pts',(-1.97210636722166,-4.7462589722096,17.6285126079779));
#9714=CARTESIAN_POINT('Ctrl Pts',(-2.13095486650566,-4.67709431563192,17.6192323217107));
#9715=CARTESIAN_POINT('Ctrl Pts',(-2.50885491894068,-4.48929526969065,17.5966068682422));
#9716=CARTESIAN_POINT('Ctrl Pts',(-2.72335511615857,-4.36250603516885,17.5832776712024));
#9717=CARTESIAN_POINT('Ctrl Pts',(-3.11179307903059,-4.09305246121396,17.5576643949609));
#9718=CARTESIAN_POINT('Ctrl Pts',(-3.2872237599939,-3.95354154702929,17.5454392737154));
#9719=CARTESIAN_POINT('Ctrl Pts',(-3.60436348847681,-3.66559260309525,17.5219562055037));
#9720=CARTESIAN_POINT('Ctrl Pts',(-3.74739920314977,-3.51923377650921,17.5107294974293));
#9721=CARTESIAN_POINT('Ctrl Pts',(-3.93500875435967,-3.30282027969124,17.4951831740091));
#9722=CARTESIAN_POINT('Ctrl Pts',(-3.98719681820654,-3.23962613228291,17.4907607822306));
#9723=CARTESIAN_POINT('Ctrl Pts',(-4.13608238250839,-3.05029129528728,17.4777986243122));
#9724=CARTESIAN_POINT('Ctrl Pts',(-4.22846405416202,-2.92088116657053,17.4692975507402));
#9725=CARTESIAN_POINT('Ctrl Pts',(-4.42032734598644,-2.62388997790252,17.4503296429262));
#9726=CARTESIAN_POINT('Ctrl Pts',(-4.51657509823625,-2.45451414535387,17.439863364329));
#9727=CARTESIAN_POINT('Ctrl Pts',(-4.67047743021137,-2.1438204908354,17.4210657071102));
#9728=CARTESIAN_POINT('Ctrl Pts',(-4.73189225998554,-2.00462467103621,17.4127791494057));
#9729=CARTESIAN_POINT('Ctrl Pts',(-4.84196947364945,-1.72176421404937,17.3961713318408));
#9730=CARTESIAN_POINT('Ctrl Pts',(-4.89062846405803,-1.57825642847592,17.3878584696979));
#9731=CARTESIAN_POINT('Ctrl Pts',(-4.96275726543717,-1.32993147718,17.3736924384381));
#9732=CARTESIAN_POINT('Ctrl Pts',(-4.98941405036863,-1.22614247813126,17.3678355417351));
#9733=CARTESIAN_POINT('Ctrl Pts',(-5.03187807510936,-1.03635566764883,17.3572685016428));
#9734=CARTESIAN_POINT('Ctrl Pts',(-5.04877269601564,-0.950644272263282,
17.3525519515872));
#9735=CARTESIAN_POINT('Ctrl Pts',(-5.11223467734277,-0.578958407071054,
17.3322558616643));
#9736=CARTESIAN_POINT('Ctrl Pts',(-5.13674744982588,-0.289762218613553,
17.3168255570649));
#9737=CARTESIAN_POINT('Ctrl Pts',(-5.13674999980103,-4.52116533001395E-5,
17.3011889615917));
#9738=CARTESIAN_POINT('',(-5.13710816050031,7.20752253655782E-5,16.8240415053031));
#9739=CARTESIAN_POINT('Ctrl Pts',(-4.29183622825304,2.82247096572396,18.4117650535551));
#9740=CARTESIAN_POINT('Ctrl Pts',(-4.17729142014888,2.99664726838564,18.4004562709275));
#9741=CARTESIAN_POINT('Ctrl Pts',(-4.0522485494874,3.16369132246763,18.3892490601967));
#9742=CARTESIAN_POINT('Ctrl Pts',(-3.76714717503251,3.49982275379707,18.3656070223839));
#9743=CARTESIAN_POINT('Ctrl Pts',(-3.60505464161424,3.66656979677188,18.3532065310692));
#9744=CARTESIAN_POINT('Ctrl Pts',(-3.40233792251312,3.84862474822056,18.3384239057725));
#9745=CARTESIAN_POINT('Ctrl Pts',(-3.3721224706653,3.87512655160327,18.3362377016896));
#9746=CARTESIAN_POINT('Ctrl Pts',(-3.16459498699542,4.05288239833501,18.3213445081467));
#9747=CARTESIAN_POINT('Ctrl Pts',(-2.97747823462929,4.19227149667809,18.308528637086));
#9748=CARTESIAN_POINT('Ctrl Pts',(-2.6276227720543,4.41761479696217,18.285761427677));
#9749=CARTESIAN_POINT('Ctrl Pts',(-2.46850719240987,4.50845832669544,18.2757979316256));
#9750=CARTESIAN_POINT('Ctrl Pts',(-2.23495718032712,4.62572032282574,18.2616626597772));
#9751=CARTESIAN_POINT('Ctrl Pts',(-2.1642419495692,4.65922515641597,18.2574426905591));
#9752=CARTESIAN_POINT('Ctrl Pts',(-1.91113091214703,4.7721427390743,18.2425244393054));
#9753=CARTESIAN_POINT('Ctrl Pts',(-1.72491935742319,4.84256349010087,18.2318918003444));
#9754=CARTESIAN_POINT('Ctrl Pts',(-1.42338688275734,4.93699023108016,18.2149285670648));
#9755=CARTESIAN_POINT('Ctrl Pts',(-1.31051830412915,4.96814288313003,18.2086315397027));
#9756=CARTESIAN_POINT('Ctrl Pts',(-1.02879923236747,5.03563067068677,18.1929225210189));
#9757=CARTESIAN_POINT('Ctrl Pts',(-0.858994116135272,5.06735940509753,18.1834611450474));
#9758=CARTESIAN_POINT('Ctrl Pts',(-0.440305647335727,5.12394016925705,18.1602935892258));
#9759=CARTESIAN_POINT('Ctrl Pts',(-0.190577052903982,5.13929149893427,18.1466237460747));
#9760=CARTESIAN_POINT('Ctrl Pts',(0.283097573035408,5.13382488326603,18.1209350438989));
#9761=CARTESIAN_POINT('Ctrl Pts',(0.506510921764593,5.11661526517205,18.1089163947818));
#9762=CARTESIAN_POINT('Ctrl Pts',(0.930586198121767,5.05589307083235,18.0859453006201));
#9763=CARTESIAN_POINT('Ctrl Pts',(1.13116455350242,5.01482891895945,18.075008035215));
#9764=CARTESIAN_POINT('Ctrl Pts',(1.46969291534403,4.92417416753471,18.0560127457752));
#9765=CARTESIAN_POINT('Ctrl Pts',(1.60895616593196,4.88044536116322,18.0480301927375));
#9766=CARTESIAN_POINT('Ctrl Pts',(2.02565778031868,4.7298237745217,18.0237429862404));
#9767=CARTESIAN_POINT('Ctrl Pts',(2.29586269470293,4.60473069894816,18.0074693807844));
#9768=CARTESIAN_POINT('Ctrl Pts',(2.74505358913806,4.34735559338287,17.9794278079863));
#9769=CARTESIAN_POINT('Ctrl Pts',(2.9291168759043,4.22552916188098,17.9675994920698));
#9770=CARTESIAN_POINT('Ctrl Pts',(3.25452720053356,3.97864093698851,17.9456998901642));
#9771=CARTESIAN_POINT('Ctrl Pts',(3.39791956332195,3.85689916695081,17.9356404723725));
#9772=CARTESIAN_POINT('Ctrl Pts',(3.63175183942997,3.63519027744683,17.9181817162467));
#9773=CARTESIAN_POINT('Ctrl Pts',(3.72552755113281,3.53902143615341,17.9108423986012));
#9774=CARTESIAN_POINT('Ctrl Pts',(4.02786888909865,3.20361490148474,17.8861005576203));
#9775=CARTESIAN_POINT('Ctrl Pts',(4.21802522448991,2.94875379992072,17.8687163620516));
#9776=CARTESIAN_POINT('Ctrl Pts',(4.49743004609412,2.49140974007656,17.8396978938611));
#9777=CARTESIAN_POINT('Ctrl Pts',(4.59938362969397,2.29775370792452,17.8279726521861));
#9778=CARTESIAN_POINT('Ctrl Pts',(4.76359026749968,1.9308117096969,17.8064197243696));
#9779=CARTESIAN_POINT('Ctrl Pts',(4.82947421410003,1.7595461372621,17.7966035667384));
#9780=CARTESIAN_POINT('Ctrl Pts',(4.92659405520577,1.46018039391778,17.7795535273557));
#9781=CARTESIAN_POINT('Ctrl Pts',(4.96232099674567,1.33372583620419,17.772375401574));
#9782=CARTESIAN_POINT('Ctrl Pts',(5.06898965010618,0.892105387063896,17.7474856355408));
#9783=CARTESIAN_POINT('Ctrl Pts',(5.11504369155602,0.571704615707682,17.7297880473185));
#9784=CARTESIAN_POINT('Ctrl Pts',(5.14141410628452,0.0285588752323948,17.7003483308169));
#9785=CARTESIAN_POINT('Ctrl Pts',(5.13789071047248,-0.192447469864089,17.6885093298539));
#9786=CARTESIAN_POINT('Ctrl Pts',(5.10483646691397,-0.602690807280177,17.6664437945442));
#9787=CARTESIAN_POINT('Ctrl Pts',(5.07893563493334,-0.791834426917885,17.6562312185668));
#9788=CARTESIAN_POINT('Ctrl Pts',(4.98456698068468,-1.27785603291861,17.6293697419292));
#9789=CARTESIAN_POINT('Ctrl Pts',(4.90012152203756,-1.57087018022075,17.6125991913699));
#9790=CARTESIAN_POINT('Ctrl Pts',(4.72802933968859,-2.01534667133899,17.5865624835649));
#9791=CARTESIAN_POINT('Ctrl Pts',(4.65777824027157,-2.17278335127782,17.5772047004971));
#9792=CARTESIAN_POINT('Ctrl Pts',(4.54307083848007,-2.39859673866215,17.5635237235733));
#9793=CARTESIAN_POINT('Ctrl Pts',(4.50469127772786,-2.46992219036066,17.5591617511586));
#9794=CARTESIAN_POINT('Ctrl Pts',(4.40715765450393,-2.64133925662669,17.5485584336382));
#9795=CARTESIAN_POINT('Ctrl Pts',(4.34626128713217,-2.7403876877419,17.5423290476631));
#9796=CARTESIAN_POINT('Ctrl Pts',(4.18416721160263,-2.98502157341648,17.5265954811246));
#9797=CARTESIAN_POINT('Ctrl Pts',(4.07869897615658,-3.12759034978395,17.5171007480445));
#9798=CARTESIAN_POINT('Ctrl Pts',(3.84963645989993,-3.40588770933626,17.4975538640286));
#9799=CARTESIAN_POINT('Ctrl Pts',(3.72571187768934,-3.54102149480902,17.4875067109068));
#9800=CARTESIAN_POINT('Ctrl Pts',(3.42427514565471,-3.83634668577909,17.4643662207096));
#9801=CARTESIAN_POINT('Ctrl Pts',(3.24225257793722,-3.99136898997188,17.4513075558077));
#9802=CARTESIAN_POINT('Ctrl Pts',(2.87014197802326,-4.2659710436289,17.426228460559));
#9803=CARTESIAN_POINT('Ctrl Pts',(2.6816964310369,-4.38688170404235,17.4142190445261));
#9804=CARTESIAN_POINT('Ctrl Pts',(2.30674190297485,-4.59424521869185,17.3912439148772));
#9805=CARTESIAN_POINT('Ctrl Pts',(2.12175088500714,-4.68255458339153,17.3802934988848));
#9806=CARTESIAN_POINT('Ctrl Pts',(1.79663375006475,-4.81452456928245,17.3612751315745));
#9807=CARTESIAN_POINT('Ctrl Pts',(1.65900102015976,-4.86366668708399,17.3532828890041));
#9808=CARTESIAN_POINT('Ctrl Pts',(1.2358383332995,-4.99470336099618,17.3290011250798));
#9809=CARTESIAN_POINT('Ctrl Pts',(0.945123498846985,-5.05777693692968,17.31274279804));
#9810=CARTESIAN_POINT('Ctrl Pts',(0.431998916036982,-5.12329363451995,17.2847233468242));
#9811=CARTESIAN_POINT('Ctrl Pts',(0.211838217465618,-5.13710889563219,17.272902084057));
#9812=CARTESIAN_POINT('Ctrl Pts',(-0.196746411185736,-5.13643033591684,
17.2509961470586));
#9813=CARTESIAN_POINT('Ctrl Pts',(-0.384799276862744,-5.12577338476215,
17.2409233903086));
#9814=CARTESIAN_POINT('Ctrl Pts',(-0.705440872973576,-5.08985532941652,
17.2234419372848));
#9815=CARTESIAN_POINT('Ctrl Pts',(-0.838401333636091,-5.06965045985436,
17.2160934956458));
#9816=CARTESIAN_POINT('Ctrl Pts',(-1.28168693270424,-4.98437124144774,17.1913595633278));
#9817=CARTESIAN_POINT('Ctrl Pts',(-1.58675955301951,-4.89580245744769,17.1739926276419));
#9818=CARTESIAN_POINT('Ctrl Pts',(-2.09164237291725,-4.69703415192307,17.1446132711876));
#9819=CARTESIAN_POINT('Ctrl Pts',(-2.29589307964555,-4.60064941949856,17.1325188221545));
#9820=CARTESIAN_POINT('Ctrl Pts',(-2.65656459669882,-4.40043179080046,17.1104026466122));
#9821=CARTESIAN_POINT('Ctrl Pts',(-2.81490597897205,-4.3008646990373,17.1003943481458));
#9822=CARTESIAN_POINT('Ctrl Pts',(-3.10941204607132,-4.09243186596577,17.0808215241124));
#9823=CARTESIAN_POINT('Ctrl Pts',(-3.24616379704547,-3.98482882862778,17.0712887915749));
#9824=CARTESIAN_POINT('Ctrl Pts',(-3.56233202808911,-3.70895723318056,17.0482794560179));
#9825=CARTESIAN_POINT('Ctrl Pts',(-3.73564590013667,-3.53433551753394,17.0348392238272));
#9826=CARTESIAN_POINT('Ctrl Pts',(-3.99530004859555,-3.23219503921335,17.0132352581982));
#9827=CARTESIAN_POINT('Ctrl Pts',(-4.08959266601737,-3.11203153742824,17.0050069522831));
#9828=CARTESIAN_POINT('Ctrl Pts',(-4.32456907535156,-2.78342549388566,16.9833014808359));
#9829=CARTESIAN_POINT('Ctrl Pts',(-4.45554330830702,-2.56855711066458,16.9699079677962));
#9830=CARTESIAN_POINT('Ctrl Pts',(-4.61619745960899,-2.25544806061679,16.950888944624));
#9831=CARTESIAN_POINT('Ctrl Pts',(-4.65948979842799,-2.1645966928949,16.945415547154));
#9832=CARTESIAN_POINT('Ctrl Pts',(-4.82299626053955,-1.79379738452305,16.9232744878646));
#9833=CARTESIAN_POINT('Ctrl Pts',(-4.92087083109501,-1.50467191251198,16.9065229113958));
#9834=CARTESIAN_POINT('Ctrl Pts',(-5.0313610192208,-1.04824654846185,16.8809774766104));
#9835=CARTESIAN_POINT('Ctrl Pts',(-5.06242885400186,-0.886132218254847,
16.8720620011718));
#9836=CARTESIAN_POINT('Ctrl Pts',(-5.11967574179977,-0.483342487670679,
16.8501678933299));
#9837=CARTESIAN_POINT('Ctrl Pts',(-5.13675391529282,-0.241780142526097,
16.837267788286));
#9838=CARTESIAN_POINT('Ctrl Pts',(-5.13674999932672,8.31682109386084E-5,
16.8242476778055));
#9839=CARTESIAN_POINT('Ctrl Pts',(-5.13710816050031,7.20752253655782E-5,
16.8240415053031));
#9840=CARTESIAN_POINT('Ctrl Pts',(-5.13715779729353,0.0723514105409758,
16.8201215600253));
#9841=CARTESIAN_POINT('Ctrl Pts',(-5.1180136959542,0.998597169429349,16.7698867892109));
#9842=CARTESIAN_POINT('Ctrl Pts',(-4.82253505916112,1.98281728759478,16.7158779233678));
#9843=CARTESIAN_POINT('Ctrl Pts',(-4.33041692566161,2.76455369449908,16.6657890028017));
#9844=CARTESIAN_POINT('Ctrl Pts',(-4.2921400227931,2.82267100337914,16.6620149077712));
#9845=CARTESIAN_POINT('Origin',(0.,0.,0.));
#9846=CARTESIAN_POINT('',(-4.29183622825303,2.82247096572397,14.9120225013103));
#9847=CARTESIAN_POINT('',(-4.29193634902365,2.82253681971926,15.3889288619751));
#9848=CARTESIAN_POINT('',(-4.29183622825304,2.82247096572397,0.));
#9849=CARTESIAN_POINT('',(-5.13679173984141,-1.83418071718305E-5,15.5509584943052));
#9850=CARTESIAN_POINT('Ctrl Pts',(-4.29193634902365,2.82253681971926,15.3889288619751));
#9851=CARTESIAN_POINT('Ctrl Pts',(-4.37956752146452,2.68958806914296,15.397563331971));
#9852=CARTESIAN_POINT('Ctrl Pts',(-4.8888867266577,1.83254938415906,15.4515732081804));
#9853=CARTESIAN_POINT('Ctrl Pts',(-5.13701666034835,0.836615721865797,15.5055830843898));
#9854=CARTESIAN_POINT('Ctrl Pts',(-5.13718616213208,-1.8274961578194E-5,
15.5509584906033));
#9855=CARTESIAN_POINT('Ctrl Pts',(-5.13674999996723,-1.83488811297034E-5,
15.5509584946969));
#9856=CARTESIAN_POINT('Ctrl Pts',(-5.13674993810036,-0.0173379132944814,
15.5518979126546));
#9857=CARTESIAN_POINT('Ctrl Pts',(-5.13666228124092,-0.034657405979478,
15.5528373306123));
#9858=CARTESIAN_POINT('Ctrl Pts',(-5.13648703461004,-0.0519760116108816,
15.55377674857));
#9859=CARTESIAN_POINT('Ctrl Pts',(-5.13498191205194,-0.200718523118732,
15.5618450301256));
#9860=CARTESIAN_POINT('Ctrl Pts',(-5.12701123425339,-0.349423111989173,
15.5699133116812));
#9861=CARTESIAN_POINT('Ctrl Pts',(-5.11259965267357,-0.497519199611531,
15.5779815932369));
#9862=CARTESIAN_POINT('Ctrl Pts',(-5.09819097957807,-0.64558539910911,15.5860482464861));
#9863=CARTESIAN_POINT('Ctrl Pts',(-5.07734402803056,-0.793043013100553,
15.5941148997355));
#9864=CARTESIAN_POINT('Ctrl Pts',(-5.05013535894052,-0.939326045033739,
15.6021815529848));
#9865=CARTESIAN_POINT('Ctrl Pts',(-5.02292570899642,-1.08561435037093,15.6102484970315));
#9866=CARTESIAN_POINT('Ctrl Pts',(-4.98935393939874,-1.23072766280729,15.6183154410782));
#9867=CARTESIAN_POINT('Ctrl Pts',(-4.94954793737664,-1.37410908522963,15.626382385125));
#9868=CARTESIAN_POINT('Ctrl Pts',(-4.90974434327348,-1.51748183431567,15.6344488411914));
#9869=CARTESIAN_POINT('Ctrl Pts',(-4.86370736054753,-1.65912258423355,15.6425152972578));
#9870=CARTESIAN_POINT('Ctrl Pts',(-4.81161506599276,-1.79848853741454,15.6505817533242));
#9871=CARTESIAN_POINT('Ctrl Pts',(-4.75950977124494,-1.93788927086987,15.6586502224615));
#9872=CARTESIAN_POINT('Ctrl Pts',(-4.7013462603938,-2.07501376276413,15.6667186915989));
#9873=CARTESIAN_POINT('Ctrl Pts',(-4.63735142535981,-2.20933752971639,15.6747871607363));
#9874=CARTESIAN_POINT('Ctrl Pts',(-4.58993691686327,-2.30885955186182,15.6807651822167));
#9875=CARTESIAN_POINT('Ctrl Pts',(-4.53932232389019,-2.40684448201293,15.686743203697));
#9876=CARTESIAN_POINT('Ctrl Pts',(-4.48561650980242,-2.50308711184569,15.6927212251774));
#9877=CARTESIAN_POINT('Ctrl Pts',(-4.41313205475769,-2.63298169949865,15.7007895067334));
#9878=CARTESIAN_POINT('Ctrl Pts',(-4.33498817017062,-2.75974967557468,15.7088577882893));
#9879=CARTESIAN_POINT('Ctrl Pts',(-4.25147948462556,-2.8829017940797,15.7169260698452));
#9880=CARTESIAN_POINT('Ctrl Pts',(-4.16798765244924,-3.0060290585465,15.7249927230947));
#9881=CARTESIAN_POINT('Ctrl Pts',(-4.07913336499658,-3.12554164748738,15.7330593763443));
#9882=CARTESIAN_POINT('Ctrl Pts',(-3.98525464170453,-3.24097917353267,15.7411260295938));
#9883=CARTESIAN_POINT('Ctrl Pts',(-3.89137253414861,-3.35642086102195,15.7491929736407));
#9884=CARTESIAN_POINT('Ctrl Pts',(-3.79246583420825,-3.46778693246239,15.7572599176875));
#9885=CARTESIAN_POINT('Ctrl Pts',(-3.68891327886389,-3.57464954695165,15.7653268617344));
#9886=CARTESIAN_POINT('Ctrl Pts',(-3.58536698755379,-3.6815056971767,15.7733933178008));
#9887=CARTESIAN_POINT('Ctrl Pts',(-3.47717563402646,-3.78385869829883,15.7814597738673));
#9888=CARTESIAN_POINT('Ctrl Pts',(-3.36475528239498,-3.88131710274941,15.7895262299338));
#9889=CARTESIAN_POINT('Ctrl Pts',(-3.25230687505414,-3.97879982899432,15.7975946990712));
#9890=CARTESIAN_POINT('Ctrl Pts',(-3.13562761053602,-4.07138530033998,15.8056631682087));
#9891=CARTESIAN_POINT('Ctrl Pts',(-3.01516765674759,-4.1587215059683,15.8137316373462));
#9892=CARTESIAN_POINT('Ctrl Pts',(-2.92591749306916,-4.22342990408932,15.8197096588255));
#9893=CARTESIAN_POINT('Ctrl Pts',(-2.83459264143782,-4.28525752760166,15.8256876803049));
#9894=CARTESIAN_POINT('Ctrl Pts',(-2.74138687527713,-4.34407626113519,15.8316657017843));
#9895=CARTESIAN_POINT('Ctrl Pts',(-2.61559101345333,-4.42346140629326,15.83973398334));
#9896=CARTESIAN_POINT('Ctrl Pts',(-2.48632132122764,-4.4973933555963,15.8478022648957));
#9897=CARTESIAN_POINT('Ctrl Pts',(-2.35407058924334,-4.56558344829656,15.8558705464515));
#9898=CARTESIAN_POINT('Ctrl Pts',(-2.22184654754109,-4.63375977916141,15.8639371997008));
#9899=CARTESIAN_POINT('Ctrl Pts',(-2.0866429603596,-4.69619641365086,15.8720038529502));
#9900=CARTESIAN_POINT('Ctrl Pts',(-1.94897691417263,-4.75265079198147,15.8800705061996));
#9901=CARTESIAN_POINT('Ctrl Pts',(-1.81130590521841,-4.809107205454,15.8881374502463));
#9902=CARTESIAN_POINT('Ctrl Pts',(-1.67117256443708,-4.85958080213363,15.896204394293));
#9903=CARTESIAN_POINT('Ctrl Pts',(-1.52911416225848,-4.90387708260317,15.9042713383398));
#9904=CARTESIAN_POINT('Ctrl Pts',(-1.38706435338487,-4.94817068353075,15.9123377944061));
#9905=CARTESIAN_POINT('Ctrl Pts',(-1.24309003234839,-4.98628761806158,15.9204042504725));
#9906=CARTESIAN_POINT('Ctrl Pts',(-1.09774383587324,-5.01808320310677,15.9284707065389));
#9907=CARTESIAN_POINT('Ctrl Pts',(-0.952361366689644,-5.04988672308259,
15.9365391756762));
#9908=CARTESIAN_POINT('Ctrl Pts',(-0.805606661340605,-5.07536566987868,
15.9446076448136));
#9909=CARTESIAN_POINT('Ctrl Pts',(-0.6580434362872,-5.0944263070987,15.9526761139509));
#9910=CARTESIAN_POINT('Ctrl Pts',(-0.548712147532794,-5.10854855219731,
15.9586541354311));
#9911=CARTESIAN_POINT('Ctrl Pts',(-0.438937267950764,-5.11914852251498,
15.9646321569114));
#9912=CARTESIAN_POINT('Ctrl Pts',(-0.328950249182865,-5.12620642347365,
15.9706101783916));
#9913=CARTESIAN_POINT('Ctrl Pts',(-0.180505443845024,-5.1357321724724,15.9786784599477));
#9914=CARTESIAN_POINT('Ctrl Pts',(-0.0316191457278236,-5.13880734577375,
15.9867467415038));
#9915=CARTESIAN_POINT('Ctrl Pts',(0.117137809096552,-5.13541422829552,15.9948150230599));
#9916=CARTESIAN_POINT('Ctrl Pts',(0.265864742422901,-5.13202179560187,16.0028816763096));
#9917=CARTESIAN_POINT('Ctrl Pts',(0.414462053806652,-5.12216368398763,16.0109483295594));
#9918=CARTESIAN_POINT('Ctrl Pts',(0.562359628422229,-5.10587428466671,16.0190149828091));
#9919=CARTESIAN_POINT('Ctrl Pts',(0.710262534644763,-5.08958429812403,16.0270819268562));
#9920=CARTESIAN_POINT('Ctrl Pts',(0.857465324196741,-5.06686259241309,16.0351488709033));
#9921=CARTESIAN_POINT('Ctrl Pts',(1.00340315167862,-5.0377954184049,16.0432158149504));
#9922=CARTESIAN_POINT('Ctrl Pts',(1.14933215118369,-5.00873000270943,16.0512822710171));
#9923=CARTESIAN_POINT('Ctrl Pts',(1.29399601721132,-4.97331995210457,16.0593487270838));
#9924=CARTESIAN_POINT('Ctrl Pts',(1.43684024440614,-4.93170261416429,16.0674151831505));
#9925=CARTESIAN_POINT('Ctrl Pts',(1.57972011991608,-4.89007489016917,16.0754836522882));
#9926=CARTESIAN_POINT('Ctrl Pts',(1.72077913104728,-4.84223687544647,16.0835521214259));
#9927=CARTESIAN_POINT('Ctrl Pts',(1.85947741742588,-4.78837595606101,16.0916205905636));
#9928=CARTESIAN_POINT('Ctrl Pts',(1.9622405712331,-4.74846978210946,16.097598612042));
#9929=CARTESIAN_POINT('Ctrl Pts',(2.06370809445908,-4.70525837990009,16.1035766335203));
#9930=CARTESIAN_POINT('Ctrl Pts',(2.16366727307025,-4.65883510053154,16.1095546549987));
#9931=CARTESIAN_POINT('Ctrl Pts',(2.29857792870794,-4.59617957311044,16.1176229365539));
#9932=CARTESIAN_POINT('Ctrl Pts',(2.43079012661376,-4.52764840371988,16.1256912181092));
#9933=CARTESIAN_POINT('Ctrl Pts',(2.55979412531764,-4.45349914095527,16.1337594996644));
#9934=CARTESIAN_POINT('Ctrl Pts',(2.68877208898131,-4.37936484268057,16.1418261529133));
#9935=CARTESIAN_POINT('Ctrl Pts',(2.81454285834313,-4.29961487788759,16.1498928061621));
#9936=CARTESIAN_POINT('Ctrl Pts',(2.93662225445447,-4.21455220600514,16.1579594594109));
#9937=CARTESIAN_POINT('Ctrl Pts',(3.05870605144513,-4.12948646767112,16.1660264034572));
#9938=CARTESIAN_POINT('Ctrl Pts',(3.17709793515927,-4.03910782512636,16.1740933475034));
#9939=CARTESIAN_POINT('Ctrl Pts',(3.29134316504544,-3.9437622560708,16.1821602915496));
#9940=CARTESIAN_POINT('Ctrl Pts',(3.40558148408308,-3.84842245459773,16.1902267476155));
#9941=CARTESIAN_POINT('Ctrl Pts',(3.5156733974926,-3.74811654043978,16.1982932036813));
#9942=CARTESIAN_POINT('Ctrl Pts',(3.62119769074238,-3.64323041366616,16.2063596597472));
#9943=CARTESIAN_POINT('Ctrl Pts',(3.726748318716,-3.53831811143001,16.214428128884));
#9944=CARTESIAN_POINT('Ctrl Pts',(3.82772881343532,-3.42882354555812,16.2224965980209));
#9945=CARTESIAN_POINT('Ctrl Pts',(3.92375476038674,-3.31516954963731,16.2305650671577));
#9946=CARTESIAN_POINT('Ctrl Pts',(3.99490148773244,-3.23096199828018,16.2365430886405));
#9947=CARTESIAN_POINT('Ctrl Pts',(4.06332917017486,-3.14447190726514,16.2425211101232));
#9948=CARTESIAN_POINT('Ctrl Pts',(4.12889567986362,-3.05588301924395,16.2484991316059));
#9949=CARTESIAN_POINT('Ctrl Pts',(4.21738801171579,-2.93631836170157,16.2565674131628));
#9950=CARTESIAN_POINT('Ctrl Pts',(4.30069967843036,-2.81288517065804,16.2646356947197));
#9951=CARTESIAN_POINT('Ctrl Pts',(4.37850628149582,-2.68605348148574,16.2727039762766));
#9952=CARTESIAN_POINT('Ctrl Pts',(4.45629718196249,-2.55924738894728,16.280770629527));
#9953=CARTESIAN_POINT('Ctrl Pts',(4.52858506228784,-2.42904444859185,16.2888372827775));
#9954=CARTESIAN_POINT('Ctrl Pts',(4.5950896969485,-2.29594234237223,16.296903936028));
#9955=CARTESIAN_POINT('Ctrl Pts',(4.66159672905597,-2.16283543791232,16.3049708800759));
#9956=CARTESIAN_POINT('Ctrl Pts',(4.72231994697923,-2.02682945285514,16.3130378241237));
#9957=CARTESIAN_POINT('Ctrl Pts',(4.77702555701905,-1.8884457604302,16.3211047681716));
#9958=CARTESIAN_POINT('Ctrl Pts',(4.83172785784242,-1.75007043902227,16.329171224239));
#9959=CARTESIAN_POINT('Ctrl Pts',(4.88041315809126,-1.6093180061423,16.3372376803065));
#9960=CARTESIAN_POINT('Ctrl Pts',(4.92289620416854,-1.46672885206603,16.345304136374));
#9961=CARTESIAN_POINT('Ctrl Pts',(4.96538985234736,-1.3241041133312,16.3533726055124));
#9962=CARTESIAN_POINT('Ctrl Pts',(5.00167805827274,-1.17964205468374,16.3614410746508));
#9963=CARTESIAN_POINT('Ctrl Pts',(5.03162555347915,-1.03389789248049,16.3695095437893));
#9964=CARTESIAN_POINT('Ctrl Pts',(5.05381399671215,-0.925914368406157,16.3754875652639));
#9965=CARTESIAN_POINT('Ctrl Pts',(5.07252274191634,-0.817227357277184,16.3814655867385));
#9966=CARTESIAN_POINT('Ctrl Pts',(5.08771489077454,-0.708066206432031,16.3874436082131));
#9967=CARTESIAN_POINT('Ctrl Pts',(5.10821908851433,-0.560736039822586,16.3955118897678));
#9968=CARTESIAN_POINT('Ctrl Pts',(5.122323189392,-0.412487394673058,16.4035801713225));
#9969=CARTESIAN_POINT('Ctrl Pts',(5.12996720927492,-0.26388822304926,16.4116484528772));
#9970=CARTESIAN_POINT('Ctrl Pts',(5.13760968647414,-0.11531904108037,16.4197151061255));
#9971=CARTESIAN_POINT('Ctrl Pts',(5.13879466669358,0.0336001958547929,16.4277817593738));
#9972=CARTESIAN_POINT('Ctrl Pts',(5.13351418218723,0.182298392155877,16.4358484126221));
#9973=CARTESIAN_POINT('Ctrl Pts',(5.12823350732299,0.331001948925982,16.4439153566678));
#9974=CARTESIAN_POINT('Ctrl Pts',(5.11648690929533,0.479484118190521,16.4519823007134));
#9975=CARTESIAN_POINT('Ctrl Pts',(5.09831852795476,0.627175214763183,16.4600492447591));
#9976=CARTESIAN_POINT('Ctrl Pts',(5.08015124564415,0.774857377301651,16.4681157008244));
#9977=CARTESIAN_POINT('Ctrl Pts',(5.05556299840837,0.921748234430995,16.4761821568897));
#9978=CARTESIAN_POINT('Ctrl Pts',(5.02464964873995,1.06728462460466,16.484248612955));
#9979=CARTESIAN_POINT('Ctrl Pts',(4.99372858431214,1.21285733495211,16.4923170820914));
#9980=CARTESIAN_POINT('Ctrl Pts',(4.95647933147031,1.3570745788207,16.5003855512277));
#9981=CARTESIAN_POINT('Ctrl Pts',(4.91304873918663,1.4993840898438,16.508454020364));
#9982=CARTESIAN_POINT('Ctrl Pts',(4.88087051436959,1.60482284162026,16.5144320418494));
#9983=CARTESIAN_POINT('Ctrl Pts',(4.84530010708197,1.70921455443603,16.5204100633349));
#9984=CARTESIAN_POINT('Ctrl Pts',(4.80641484242291,1.81234017917077,16.5263880848203));
#9985=CARTESIAN_POINT('Ctrl Pts',(4.75393305318738,1.95152445243119,16.5344563663762));
#9986=CARTESIAN_POINT('Ctrl Pts',(4.69539174482462,2.08845327215774,16.5425246479321));
#9987=CARTESIAN_POINT('Ctrl Pts',(4.63100996858054,2.22259920665146,16.550592929488));
#9988=CARTESIAN_POINT('Ctrl Pts',(4.56664118559372,2.35671806838113,16.5586595827375));
#9989=CARTESIAN_POINT('Ctrl Pts',(4.49643442939982,2.48805486710282,16.566726235987));
#9990=CARTESIAN_POINT('Ctrl Pts',(4.42065593215064,2.61610429685848,16.5747928892365));
#9991=CARTESIAN_POINT('Ctrl Pts',(4.34487470313824,2.74415834270886,16.5828598332834));
#9992=CARTESIAN_POINT('Ctrl Pts',(4.26352149645798,2.86892449566634,16.5909267773303));
#9993=CARTESIAN_POINT('Ctrl Pts',(4.17690762651911,2.98992361809236,16.5989937213771));
#9994=CARTESIAN_POINT('Ctrl Pts',(4.09029899597056,3.11091542111755,16.6070601774436));
#9995=CARTESIAN_POINT('Ctrl Pts',(3.9984305321498,3.22814038079684,16.6151266335101));
#9996=CARTESIAN_POINT('Ctrl Pts',(3.90165584736817,3.34114983369464,16.6231930895766));
#9997=CARTESIAN_POINT('Ctrl Pts',(3.80485701142197,3.45418748931822,16.631261558714));
#9998=CARTESIAN_POINT('Ctrl Pts',(3.70314972283527,3.56300728402921,16.6393300278515));
#9999=CARTESIAN_POINT('Ctrl Pts',(3.5969271539055,3.66719451515696,16.6473984969889));
#10000=CARTESIAN_POINT('Ctrl Pts',(3.51822563223433,3.74438803166739,16.6533765184684));
#10001=CARTESIAN_POINT('Ctrl Pts',(3.43704628064773,3.81903919663655,16.659354539948));
#10002=CARTESIAN_POINT('Ctrl Pts',(3.35356179983878,3.89099265190287,16.6653325614275));
#10003=CARTESIAN_POINT('Ctrl Pts',(3.24088634369147,3.9881051728762,16.6734008429876));
#10004=CARTESIAN_POINT('Ctrl Pts',(3.12396894054375,4.0803380700494,16.6814691245477));
#10005=CARTESIAN_POINT('Ctrl Pts',(3.00325428376368,4.16733299240115,16.6895374061078));
#10006=CARTESIAN_POINT('Ctrl Pts',(2.88256398910342,4.25431035780681,16.6976040593616));
#10007=CARTESIAN_POINT('Ctrl Pts',(2.75807823807291,4.33605166393318,16.7056707126153));
#10008=CARTESIAN_POINT('Ctrl Pts',(2.63027256922376,4.41224056167488,16.7137373658691));
#10009=CARTESIAN_POINT('Ctrl Pts',(2.50246229306723,4.48843220597449,16.7218043099202));
#10010=CARTESIAN_POINT('Ctrl Pts',(2.37133214197831,4.55907086861316,16.7298712539713));
#10011=CARTESIAN_POINT('Ctrl Pts',(2.23738472272639,4.62388474824044,16.7379381980224));
#10012=CARTESIAN_POINT('Ctrl Pts',(2.10344540613535,4.68869470718832,16.7460046540932));
#10013=CARTESIAN_POINT('Ctrl Pts',(1.96668946065899,4.7476804445871,16.7540711101639));
#10014=CARTESIAN_POINT('Ctrl Pts',(1.82764205620876,4.80061715583289,16.7621375662346));
#10015=CARTESIAN_POINT('Ctrl Pts',(1.68855995098234,4.85356707800466,16.7702060353763));
#10016=CARTESIAN_POINT('Ctrl Pts',(1.54718555337111,4.90046483909873,16.778274504518));
#10017=CARTESIAN_POINT('Ctrl Pts',(1.40406252411984,4.94113438299974,16.7863429736596));
#10018=CARTESIAN_POINT('Ctrl Pts',(1.29802102789186,4.97126691519064,16.792320995118));
#10019=CARTESIAN_POINT('Ctrl Pts',(1.19102001986929,4.99798147585057,16.7982990165764));
#10020=CARTESIAN_POINT('Ctrl Pts',(1.08328548092466,5.02122426598512,16.8042770380347));
#10021=CARTESIAN_POINT('Ctrl Pts',(0.937880751627644,5.05259407218404,16.8123453195757));
#10022=CARTESIAN_POINT('Ctrl Pts',(0.791085612671925,5.07764948186624,16.8204136011166));
#10023=CARTESIAN_POINT('Ctrl Pts',(0.643462006519024,5.09628857195769,16.8284818826575));
#10024=CARTESIAN_POINT('Ctrl Pts',(0.495868193137679,5.11492390038684,16.836548535892));
#10025=CARTESIAN_POINT('Ctrl Pts',(0.347446574330549,5.1271454511757,16.8446151891264));
#10026=CARTESIAN_POINT('Ctrl Pts',(0.198766083575153,5.13290294146696,16.8526818423609));
#10027=CARTESIAN_POINT('Ctrl Pts',(0.0500802329885989,5.13866063931186,
16.8607487863928));
#10028=CARTESIAN_POINT('Ctrl Pts',(-0.0988641776145617,5.13795379376828,
16.8688157304246));
#10029=CARTESIAN_POINT('Ctrl Pts',(-0.247495758396923,5.13078419075248,
16.8768826744565));
#10030=CARTESIAN_POINT('Ctrl Pts',(-0.396118348255007,5.1236150214356,16.8849491305081));
#10031=CARTESIAN_POINT('Ctrl Pts',(-0.544427815545846,5.1099838935302,16.8930155865596));
#10032=CARTESIAN_POINT('Ctrl Pts',(-0.691855441765988,5.08994465688958,
16.9010820426112));
#10033=CARTESIAN_POINT('Ctrl Pts',(-0.839319860141933,5.06990041924111,
16.909150511734));
#10034=CARTESIAN_POINT('Ctrl Pts',(-0.985901669447363,5.04344492126959,
16.9172189808567));
#10035=CARTESIAN_POINT('Ctrl Pts',(-1.13103923659801,5.01068366670415,16.9252874499795));
#10036=CARTESIAN_POINT('Ctrl Pts',(-1.23857332906836,4.98641047646784,16.9312654715336));
#10037=CARTESIAN_POINT('Ctrl Pts',(-1.34531473632737,4.95867681758785,16.9372434930878));
#10038=CARTESIAN_POINT('Ctrl Pts',(-1.45103927964805,4.92754356362463,16.9432215146419));
#10039=CARTESIAN_POINT('Ctrl Pts',(-1.59373120185918,4.88552433409507,16.9512897962328));
#10040=CARTESIAN_POINT('Ctrl Pts',(-1.73462308709432,4.83729505542724,16.9593580778237));
#10041=CARTESIAN_POINT('Ctrl Pts',(-1.87317271602301,4.78303507602097,16.9674263594146));
#10042=CARTESIAN_POINT('Ctrl Pts',(-2.01169438345545,4.72878604713275,16.9754930126992));
#10043=CARTESIAN_POINT('Ctrl Pts',(-2.14787442960605,4.66850886626966,16.9835596659838));
#10044=CARTESIAN_POINT('Ctrl Pts',(-2.28118920234082,4.60243157316039,16.9916263192685));
#10045=CARTESIAN_POINT('Ctrl Pts',(-2.41450878097982,4.53635189801096,16.9996932633503));
#10046=CARTESIAN_POINT('Ctrl Pts',(-2.54496258125869,4.46447183581378,17.0077602074322));
#10047=CARTESIAN_POINT('Ctrl Pts',(-2.67204970527385,4.38706632444119,17.015827151514));
#10048=CARTESIAN_POINT('Ctrl Pts',(-2.79912914161421,4.30966549543438,17.0238936076154));
#10049=CARTESIAN_POINT('Ctrl Pts',(-2.9228420268321,4.22674005883158,17.0319600637167));
#10050=CARTESIAN_POINT('Ctrl Pts',(-3.0427147177022,4.13860939316317,17.040026519818));
#10051=CARTESIAN_POINT('Ctrl Pts',(-3.16261732408451,4.05045673354446,17.0480949889897));
#10052=CARTESIAN_POINT('Ctrl Pts',(-3.27867755390728,3.95709644480316,17.0561634581614));
#10053=CARTESIAN_POINT('Ctrl Pts',(-3.39045269856158,3.85888987421467,17.0642319273331));
#10054=CARTESIAN_POINT('Ctrl Pts',(-3.47326818461293,3.7861275002372,17.0702099486384));
#10055=CARTESIAN_POINT('Ctrl Pts',(-3.55373200387586,3.71070564241949,17.0761879699437));
#10056=CARTESIAN_POINT('Ctrl Pts',(-3.63167642287095,3.63278500906168,17.082165991249));
#10057=CARTESIAN_POINT('Ctrl Pts',(-3.73687374245287,3.52761979165358,17.0902341996702));
#10058=CARTESIAN_POINT('Ctrl Pts',(-3.83751941607202,3.41786264164616,17.0983024080914));
#10059=CARTESIAN_POINT('Ctrl Pts',(-3.93322312273905,3.30393045163648,17.1063706165126));
#10060=CARTESIAN_POINT('Ctrl Pts',(-4.02890965857688,3.19001870294767,17.1144373773636));
#10061=CARTESIAN_POINT('Ctrl Pts',(-4.11965578295557,3.07193366143052,17.1225041382147));
#10062=CARTESIAN_POINT('Ctrl Pts',(-4.20511075000905,2.95012612317818,17.1305708990657));
#10063=CARTESIAN_POINT('Ctrl Pts',(-4.23465580446763,2.90801259279815,17.1333598871944));
#10064=CARTESIAN_POINT('Ctrl Pts',(-4.26356874076661,2.86545437577467,17.1361488753231));
#10065=CARTESIAN_POINT('Ctrl Pts',(-4.29183622825303,2.82247096572397,17.1389378634518));
#10066=CARTESIAN_POINT('',(-5.13670694023125,8.22511334899522E-6,15.0740415053031));
#10067=CARTESIAN_POINT('Ctrl Pts',(-4.2921400227931,2.82267100337914,16.6620149077712));
#10068=CARTESIAN_POINT('Ctrl Pts',(-3.86069158380266,3.47775593229212,16.6194741772661));
#10069=CARTESIAN_POINT('Ctrl Pts',(-2.64190503851504,4.63775144658851,16.5306186212244));
#10070=CARTESIAN_POINT('Ctrl Pts',(-0.171207780293172,5.35198763020908,
16.3954482396483));
#10071=CARTESIAN_POINT('Ctrl Pts',(2.41020538539942,4.78163086175811,16.2565037630408));
#10072=CARTESIAN_POINT('Ctrl Pts',(4.40413631567179,3.04576213958252,16.1175592864337));
#10073=CARTESIAN_POINT('Ctrl Pts',(5.32456875345049,0.567495627922317,15.9786148098264));
#10074=CARTESIAN_POINT('Ctrl Pts',(4.94714932645596,-2.04909668870878,15.8396703332193));
#10075=CARTESIAN_POINT('Ctrl Pts',(3.36387318580941,-4.16622621658075,15.7007258566122));
#10076=CARTESIAN_POINT('Ctrl Pts',(0.96066039128185,-5.26784731276012,15.5617813800049));
#10077=CARTESIAN_POINT('Ctrl Pts',(-1.67671125027514,-5.08544226996355,
15.4228369033978));
#10078=CARTESIAN_POINT('Ctrl Pts',(-3.90538823060865,-3.66347191420326,
15.2838924267906));
#10079=CARTESIAN_POINT('Ctrl Pts',(-4.97373718467484,-1.72639559785503,
15.1676272940924));
#10080=CARTESIAN_POINT('Ctrl Pts',(-5.13628689006179,-0.435997775582432,
15.0976769869299));
#10081=CARTESIAN_POINT('Ctrl Pts',(-5.13631118563065,8.22447965037609E-6,
15.0740415053031));
#10082=CARTESIAN_POINT('Ctrl Pts',(-5.13674999999342,8.22518229806563E-6,
15.0740415053031));
#10083=CARTESIAN_POINT('Ctrl Pts',(-5.13674975849047,0.150830448247622,
15.0658662706561));
#10084=CARTESIAN_POINT('Ctrl Pts',(-5.13010264657814,0.301636878576586,
15.057691036009));
#10085=CARTESIAN_POINT('Ctrl Pts',(-5.11683883531417,0.451841671297237,
15.049515801362));
#10086=CARTESIAN_POINT('Ctrl Pts',(-5.10357056040029,0.602097012204711,
15.0413378155159));
#10087=CARTESIAN_POINT('Ctrl Pts',(-5.08368116440342,0.751750000235891,
15.0331598296698));
#10088=CARTESIAN_POINT('Ctrl Pts',(-5.05725273714425,0.900219592736657,
15.0249818438237));
#10089=CARTESIAN_POINT('Ctrl Pts',(-5.03680889000711,1.01506901695079,15.0186557204079));
#10090=CARTESIAN_POINT('Ctrl Pts',(-5.01245321882611,1.1292103786262,15.0123295969921));
#10091=CARTESIAN_POINT('Ctrl Pts',(-4.98424474906023,1.24237870392465,15.0060034735762));
#10092=CARTESIAN_POINT('Ctrl Pts',(-4.94826626642743,1.3867192037861,14.9979348217373));
#10093=CARTESIAN_POINT('Ctrl Pts',(-4.9060069054024,1.52952246934126,14.9898661698984));
#10094=CARTESIAN_POINT('Ctrl Pts',(-4.85762305893994,1.67023913849334,14.9817975180595));
#10095=CARTESIAN_POINT('Ctrl Pts',(-4.80925007919966,1.81092420352419,14.9737306783915));
#10096=CARTESIAN_POINT('Ctrl Pts',(-4.75475546663133,1.94952329448943,14.9656638387235));
#10097=CARTESIAN_POINT('Ctrl Pts',(-4.69434503816343,2.08550359030387,14.9575969990554));
#10098=CARTESIAN_POINT('Ctrl Pts',(-4.63393365557878,2.22148603377861,14.9495300319805));
#10099=CARTESIAN_POINT('Ctrl Pts',(-4.56760640109698,2.35484929530895,14.9414630649055));
#10100=CARTESIAN_POINT('Ctrl Pts',(-4.49561689424886,2.48508134728911,14.9333960978305));
#10101=CARTESIAN_POINT('Ctrl Pts',(-4.43203766392339,2.60009885457767,14.9262715656571));
#10102=CARTESIAN_POINT('Ctrl Pts',(-4.36404265913438,2.7126742026278,14.9191470334837));
#10103=CARTESIAN_POINT('Ctrl Pts',(-4.29183622825303,2.82247096572397,14.9120225013103));
#10104=CARTESIAN_POINT('Origin',(0.,0.,0.));
#10105=CARTESIAN_POINT('',(-4.29183623954907,2.82247094854727,13.1619495546845));
#10106=CARTESIAN_POINT('',(-4.29183622825304,2.82247096572396,13.6389404220384));
#10107=CARTESIAN_POINT('',(-4.29183622825304,2.82247096572397,0.));
#10108=CARTESIAN_POINT('',(-5.13674999929672,8.50009777041742E-5,13.8009584946969));
#10109=CARTESIAN_POINT('Ctrl Pts',(-4.29183622825304,2.82247096572396,13.6389404220384));
#10110=CARTESIAN_POINT('Ctrl Pts',(-4.37357958870702,2.69817239185872,13.6470067765585));
#10111=CARTESIAN_POINT('Ctrl Pts',(-4.4499279442811,2.57030743963229,13.6550731310786));
#10112=CARTESIAN_POINT('Ctrl Pts',(-4.5205860970387,2.43936506119121,13.6631394855987));
#10113=CARTESIAN_POINT('Ctrl Pts',(-4.59124771236917,2.3084162659743,13.6712062354071));
#10114=CARTESIAN_POINT('Ctrl Pts',(-4.65621840730926,2.17439003276196,13.6792729852155));
#10115=CARTESIAN_POINT('Ctrl Pts',(-4.71524868839109,2.0378003751904,13.6873397350239));
#10116=CARTESIAN_POINT('Ctrl Pts',(-4.77427676683697,1.90121581427913,13.6954061838323));
#10117=CARTESIAN_POINT('Ctrl Pts',(-4.8273647452265,1.76206832492696,13.7034726326407));
#10118=CARTESIAN_POINT('Ctrl Pts',(-4.87431107211784,1.62089238838654,13.7115390814491));
#10119=CARTESIAN_POINT('Ctrl Pts',(-4.92126820165559,1.47968396637121,13.7196073863983));
#10120=CARTESIAN_POINT('Ctrl Pts',(-4.96208075214552,1.33644647894745,13.7276756913476));
#10121=CARTESIAN_POINT('Ctrl Pts',(-4.99659670171705,1.191730658702,13.7357439962968));
#10122=CARTESIAN_POINT('Ctrl Pts',(-5.01335857333664,1.12145277180072,13.7396621817567));
#10123=CARTESIAN_POINT('Ctrl Pts',(-5.02863625144882,1.05082645350585,13.7435803672166));
#10124=CARTESIAN_POINT('Ctrl Pts',(-5.04241664468204,0.979915784102628,
13.7474985526766));
#10125=CARTESIAN_POINT('Ctrl Pts',(-5.07155666765262,0.829968064883282,
13.7557839486281));
#10126=CARTESIAN_POINT('Ctrl Pts',(-5.09400667909746,0.678705261588683,
13.7640693445797));
#10127=CARTESIAN_POINT('Ctrl Pts',(-5.10967360315828,0.526722157961372,
13.7723547405312));
#10128=CARTESIAN_POINT('Ctrl Pts',(-5.12533565923321,0.374786278128614,
13.7806375620661));
#10129=CARTESIAN_POINT('Ctrl Pts',(-5.1342188057037,0.222130834218837,13.788920383601));
#10130=CARTESIAN_POINT('Ctrl Pts',(-5.13628175387216,0.0693563792299268,
13.7972032051359));
#10131=CARTESIAN_POINT('Ctrl Pts',(-5.13659352233936,0.0462679379463962,
13.7984549683229));
#10132=CARTESIAN_POINT('Ctrl Pts',(-5.13674961718268,0.0231767855100868,
13.7997067315099));
#10133=CARTESIAN_POINT('Ctrl Pts',(-5.13674999929672,8.50009777041742E-5,
13.8009584946969));
#10134=CARTESIAN_POINT('Ctrl Pts',(-5.1364024164725,8.49952260370549E-5,
13.8009584946969));
#10135=CARTESIAN_POINT('Ctrl Pts',(-5.13609293759186,-0.525535431478061,
13.8294533395592));
#10136=CARTESIAN_POINT('Ctrl Pts',(-4.92543237478305,-1.90572893214436,
13.9042630099572));
#10137=CARTESIAN_POINT('Ctrl Pts',(-3.70837745769343,-3.86277367330787,
14.0253875058909));
#10138=CARTESIAN_POINT('Ctrl Pts',(-1.40835915724232,-5.16619863188995,
14.1643319824982));
#10139=CARTESIAN_POINT('Ctrl Pts',(1.23494357489379,-5.21037409278427,14.3032764591053));
#10140=CARTESIAN_POINT('Ctrl Pts',(3.57723154024265,-3.98453238503892,14.4422209357125));
#10141=CARTESIAN_POINT('Ctrl Pts',(5.04757722440252,-1.78746971544192,14.5811654123197));
#10142=CARTESIAN_POINT('Ctrl Pts',(5.28758711676144,0.845284746454227,14.7201098889269));
#10143=CARTESIAN_POINT('Ctrl Pts',(4.23875933654995,3.2720029197328,14.8590543655341));
#10144=CARTESIAN_POINT('Ctrl Pts',(2.15674333697306,4.90117761342644,14.9979988421412));
#10145=CARTESIAN_POINT('Ctrl Pts',(-0.450974083946612,5.33570109690734,
15.1369433187485));
#10146=CARTESIAN_POINT('Ctrl Pts',(-2.79354640822019,4.52347794157121,15.2672533253597));
#10147=CARTESIAN_POINT('Ctrl Pts',(-3.90951869796817,3.40271790699677,15.3512485064353));
#10148=CARTESIAN_POINT('Ctrl Pts',(-4.29193634902365,2.82253681971926,15.3889288619751));
#10149=CARTESIAN_POINT('',(-5.13674999926869,-8.66784045078238E-5,13.3240415053031));
#10150=CARTESIAN_POINT('Ctrl Pts',(-4.29183622825303,2.82247096572397,14.9120225013103));
#10151=CARTESIAN_POINT('Ctrl Pts',(-4.21006206974841,2.94681637096182,14.9039539315706));
#10152=CARTESIAN_POINT('Ctrl Pts',(-4.12288583257787,3.06759728781872,14.8958853618309));
#10153=CARTESIAN_POINT('Ctrl Pts',(-4.03064505549953,3.18435252430965,14.8878167920912));
#10154=CARTESIAN_POINT('Ctrl Pts',(-3.95154325620129,3.28447688987175,14.8808975270505));
#10155=CARTESIAN_POINT('Ctrl Pts',(-3.86871774776158,3.38164113034757,14.8739782620097));
#10156=CARTESIAN_POINT('Ctrl Pts',(-3.78240512199835,3.47557362971649,14.8670589969689));
#10157=CARTESIAN_POINT('Ctrl Pts',(-3.68175937965753,3.58510460557681,14.8589907154131));
#10158=CARTESIAN_POINT('Ctrl Pts',(-3.57633413088022,3.69028113992072,14.8509224338573));
#10159=CARTESIAN_POINT('Ctrl Pts',(-3.46652948335297,3.79069570178676,14.8428541523014));
#10160=CARTESIAN_POINT('Ctrl Pts',(-3.35674699613402,3.89108999841176,14.834787499052));
#10161=CARTESIAN_POINT('Ctrl Pts',(-3.2425871175593,3.9867240166137,14.8267208458025));
#10162=CARTESIAN_POINT('Ctrl Pts',(-3.12448546588943,4.07722836445859,14.8186541925531));
#10163=CARTESIAN_POINT('Ctrl Pts',(-3.00637955673554,4.16773597492353,14.8105872485062));
#10164=CARTESIAN_POINT('Ctrl Pts',(-2.88433185056216,4.25311334065131,14.8025203044594));
#10165=CARTESIAN_POINT('Ctrl Pts',(-2.75881002016174,4.33303217564273,14.7944533604126));
#10166=CARTESIAN_POINT('Ctrl Pts',(-2.63329578274698,4.4129461762355,14.7863869043462));
#10167=CARTESIAN_POINT('Ctrl Pts',(-2.50430812121457,4.48740212958203,14.7783204482798));
#10168=CARTESIAN_POINT('Ctrl Pts',(-2.37234257241721,4.55611581081922,14.7702539922134));
#10169=CARTESIAN_POINT('Ctrl Pts',(-2.24034409019586,4.62484664029563,14.7621855230759));
#10170=CARTESIAN_POINT('Ctrl Pts',(-2.10536652916291,4.68783218062042,14.7541170539385));
#10171=CARTESIAN_POINT('Ctrl Pts',(-1.96792944869695,4.74483448051155,14.7460485848011));
#10172=CARTESIAN_POINT('Ctrl Pts',(-1.86610073681253,4.78706813938064,14.7400705633214));
#10173=CARTESIAN_POINT('Ctrl Pts',(-1.76292238556871,4.8260182535111,14.7340925418416));
#10174=CARTESIAN_POINT('Ctrl Pts',(-1.65861260668985,4.86160516531624,14.7281145203618));
#10175=CARTESIAN_POINT('Ctrl Pts',(-1.51783013077032,4.90963530791749,14.720046238806));
#10176=CARTESIAN_POINT('Ctrl Pts',(-1.37493393765075,4.95155504608902,14.7119779572501));
#10177=CARTESIAN_POINT('Ctrl Pts',(-1.23047034706621,4.98719793947371,14.7039096756943));
#10178=CARTESIAN_POINT('Ctrl Pts',(-1.08603591151098,5.02283363956078,14.6958430224448));
#10179=CARTESIAN_POINT('Ctrl Pts',(-0.940035030750641,5.05219494285085,
14.6877763691954));
#10180=CARTESIAN_POINT('Ctrl Pts',(-0.793026960456183,5.07516588915965,
14.6797097159459));
#10181=CARTESIAN_POINT('Ctrl Pts',(-0.64601359062089,5.09813766355542,14.6716427718991));
#10182=CARTESIAN_POINT('Ctrl Pts',(-0.497993285043127,5.11471856514564,
14.6635758278523));
#10183=CARTESIAN_POINT('Ctrl Pts',(-0.349533781033704,5.12484406576593,
14.6555088838054));
#10184=CARTESIAN_POINT('Ctrl Pts',(-0.201083257540819,5.13496895388097,
14.647442427739));
#10185=CARTESIAN_POINT('Ctrl Pts',(-0.0521939190847952,5.13863920054417,
14.6393759716725));
#10186=CARTESIAN_POINT('Ctrl Pts',(0.0965631090010042,5.13584229980634,
14.6313095156061));
#10187=CARTESIAN_POINT('Ctrl Pts',(0.245357261005208,5.13304470107181,14.6232410464687));
#10188=CARTESIAN_POINT('Ctrl Pts',(0.394018705526142,5.1237767355219,14.6151725773312));
#10189=CARTESIAN_POINT('Ctrl Pts',(0.54197736105783,5.10807802432586,14.6071041081938));
#10190=CARTESIAN_POINT('Ctrl Pts',(0.651601628785827,5.09644666884379,14.6011260867141));
#10191=CARTESIAN_POINT('Ctrl Pts',(0.760840106234247,5.08128624006824,14.5951480652344));
#10192=CARTESIAN_POINT('Ctrl Pts',(0.869463065472354,5.06263118746363,14.5891700437547));
#10193=CARTESIAN_POINT('Ctrl Pts',(1.01606685763618,5.03745325570746,14.5811017621988));
#10194=CARTESIAN_POINT('Ctrl Pts',(1.16160336386802,5.00589835418219,14.573033480643));
#10195=CARTESIAN_POINT('Ctrl Pts',(1.30551321661218,4.96808170260423,14.5649651990871));
#10196=CARTESIAN_POINT('Ctrl Pts',(1.44939402607999,4.93027268302256,14.5568985458377));
#10197=CARTESIAN_POINT('Ctrl Pts',(1.59164851704583,4.88620451862095,14.5488318925882));
#10198=CARTESIAN_POINT('Ctrl Pts',(1.731730113762,4.83604294600346,14.5407652393387));
#10199=CARTESIAN_POINT('Ctrl Pts',(1.87181676032434,4.78587956509544,14.5326982952919));
#10200=CARTESIAN_POINT('Ctrl Pts',(2.00973004299052,4.72962244443411,14.5246313512451));
#10201=CARTESIAN_POINT('Ctrl Pts',(2.14494054464602,4.66748654228736,14.5165644071983));
#10202=CARTESIAN_POINT('Ctrl Pts',(2.28014286723538,4.60535439882539,14.5084979511318));
#10203=CARTESIAN_POINT('Ctrl Pts',(2.41264243545598,4.5373443242932,14.5004314950653));
#10204=CARTESIAN_POINT('Ctrl Pts',(2.54193174603147,4.46371857995297,14.4923650389989));
#10205=CARTESIAN_POINT('Ctrl Pts',(2.67125332214657,4.39007446151546,14.4842965698614));
#10206=CARTESIAN_POINT('Ctrl Pts',(2.79736275163924,4.31081203620864,14.476228100724));
#10207=CARTESIAN_POINT('Ctrl Pts',(2.91977838698316,4.22623884008063,14.4681596315866));
#10208=CARTESIAN_POINT('Ctrl Pts',(3.01047753759911,4.16357758743804,14.4621816101069));
#10209=CARTESIAN_POINT('Ctrl Pts',(3.09914950382448,4.09800193676208,14.4562035886272));
#10210=CARTESIAN_POINT('Ctrl Pts',(3.18560903719751,4.02965204758743,14.4502255671475));
#10211=CARTESIAN_POINT('Ctrl Pts',(3.30229979530371,3.93740310668865,14.4421572855916));
#10212=CARTESIAN_POINT('Ctrl Pts',(3.41500241293278,3.84006500296762,14.4340890040358));
#10213=CARTESIAN_POINT('Ctrl Pts',(3.52328081931377,3.73800653166306,14.4260207224799));
#10214=CARTESIAN_POINT('Ctrl Pts',(3.63153737340575,3.63596865736657,14.4179540692305));
#10215=CARTESIAN_POINT('Ctrl Pts',(3.73537125682889,3.52921254294249,14.409887415981));
#10216=CARTESIAN_POINT('Ctrl Pts',(3.83438180038918,3.41814522385229,14.4018207627315));
#10217=CARTESIAN_POINT('Ctrl Pts',(3.93339591321226,3.30707390086075,14.3937538186847));
#10218=CARTESIAN_POINT('Ctrl Pts',(4.02758611514645,3.19169130676403,14.3856868746379));
#10219=CARTESIAN_POINT('Ctrl Pts',(4.11659035352502,3.07243949065962,14.377619930591));
#10220=CARTESIAN_POINT('Ctrl Pts',(4.20558920791671,2.95319488825903,14.3695534745246));
#10221=CARTESIAN_POINT('Ctrl Pts',(4.28940252901126,2.83008179787626,14.3614870184581));
#10222=CARTESIAN_POINT('Ctrl Pts',(4.36771013839118,2.70357332238187,14.3534205623917));
#10223=CARTESIAN_POINT('Ctrl Pts',(4.44603729027829,2.57703327533508,14.3453520932542));
#10224=CARTESIAN_POINT('Ctrl Pts',(4.51885581004324,2.44709643124632,14.3372836241168));
#10225=CARTESIAN_POINT('Ctrl Pts',(4.58588988465929,2.31426327981058,14.3292151549793));
#10226=CARTESIAN_POINT('Ctrl Pts',(4.63555620067292,2.2158456718391,14.3232371334997));
#10227=CARTESIAN_POINT('Ctrl Pts',(4.68204805989948,2.11583871917326,14.31725911202));
#10228=CARTESIAN_POINT('Ctrl Pts',(4.72526984724929,2.01445412784126,14.3112810905403));
#10229=CARTESIAN_POINT('Ctrl Pts',(4.78360445693056,1.8776196532467,14.3032128089844));
#10230=CARTESIAN_POINT('Ctrl Pts',(4.83600217201594,1.73822429496611,14.2951445274286));
#10231=CARTESIAN_POINT('Ctrl Pts',(4.88225650980574,1.59680053073623,14.2870762458728));
#10232=CARTESIAN_POINT('Ctrl Pts',(4.92850151274114,1.45540530805098,14.2790095926233));
#10233=CARTESIAN_POINT('Ctrl Pts',(4.96860550904096,1.31198281053287,14.2709429393739));
#10234=CARTESIAN_POINT('Ctrl Pts',(5.00241139829535,1.16708215850673,14.2628762861245));
#10235=CARTESIAN_POINT('Ctrl Pts',(5.03621850622907,1.02217628291059,14.2548093420776));
#10236=CARTESIAN_POINT('Ctrl Pts',(5.06372697389811,0.875792467660107,14.2467423980308));
#10237=CARTESIAN_POINT('Ctrl Pts',(5.08483036262077,0.728492104191907,14.238675453984));
#10238=CARTESIAN_POINT('Ctrl Pts',(5.10593247477088,0.581200651122109,14.2306089979176));
#10239=CARTESIAN_POINT('Ctrl Pts',(5.1206302369751,0.432993088553311,14.2225425418511));
#10240=CARTESIAN_POINT('Ctrl Pts',(5.12886883845637,0.284438043185459,14.2144760857847));
#10241=CARTESIAN_POINT('Ctrl Pts',(5.13710949596936,0.13584592430631,14.2064076166473));
#10242=CARTESIAN_POINT('Ctrl Pts',(5.13888775276455,-0.0130935200164274,
14.1983391475099));
#10243=CARTESIAN_POINT('Ctrl Pts',(5.13420085913043,-0.161808839697807,
14.1902706783724));
#10244=CARTESIAN_POINT('Ctrl Pts',(5.1307282857908,-0.271993728589038,14.1842926568926));
#10245=CARTESIAN_POINT('Ctrl Pts',(5.12370775009287,-0.382055509579282,
14.1783146354129));
#10246=CARTESIAN_POINT('Ctrl Pts',(5.11315657628578,-0.491762533023262,
14.1723366139331));
#10247=CARTESIAN_POINT('Ctrl Pts',(5.09891610536943,-0.639829440576593,
14.1642683323772));
#10248=CARTESIAN_POINT('Ctrl Pts',(5.0782370906738,-0.7873047429416,14.1562000508214));
#10249=CARTESIAN_POINT('Ctrl Pts',(5.05119296727215,-0.933622070154904,
14.1481317692655));
#10250=CARTESIAN_POINT('Ctrl Pts',(5.02415430180085,-1.0799098682255,14.1400651160161));
#10251=CARTESIAN_POINT('Ctrl Pts',(4.99075315052114,-1.22503983207459,14.1319984627666));
#10252=CARTESIAN_POINT('Ctrl Pts',(4.951114274685,-1.36845460337946,14.1239318095172));
#10253=CARTESIAN_POINT('Ctrl Pts',(4.91147396989435,-1.51187454468931,14.1158648654703));
#10254=CARTESIAN_POINT('Ctrl Pts',(4.86559557510579,-1.65357884967861,14.1077979214235));
#10255=CARTESIAN_POINT('Ctrl Pts',(4.81365420981613,-1.79302362249343,14.0997309773767));
#10256=CARTESIAN_POINT('Ctrl Pts',(4.76171598652996,-1.93245996010518,14.0916645213102));
#10257=CARTESIAN_POINT('Ctrl Pts',(4.70371564279289,-2.06963672906724,14.0835980652438));
#10258=CARTESIAN_POINT('Ctrl Pts',(4.63987709547407,-2.20402838035157,14.0755316091773));
#10259=CARTESIAN_POINT('Ctrl Pts',(4.5760226165583,-2.33845357051968,14.0674631400399));
#10260=CARTESIAN_POINT('Ctrl Pts',(4.50632716422018,-2.47009195472382,14.0593946709024));
#10261=CARTESIAN_POINT('Ctrl Pts',(4.43106172229953,-2.59844041218419,14.051326201765));
#10262=CARTESIAN_POINT('Ctrl Pts',(4.37529669168255,-2.69353525886649,14.0453481802853));
#10263=CARTESIAN_POINT('Ctrl Pts',(4.316475001119,-2.78682455233121,14.0393701588056));
#10264=CARTESIAN_POINT('Ctrl Pts',(4.25472269144943,-2.87811316340504,14.0333921373259));
#10265=CARTESIAN_POINT('Ctrl Pts',(4.17137822324551,-3.00132152247264,14.02532385577));
#10266=CARTESIAN_POINT('Ctrl Pts',(4.08266294289405,-3.12092998993459,14.0172555742142));
#10267=CARTESIAN_POINT('Ctrl Pts',(3.98891230360449,-3.2364763550276,14.0091872926583));
#10268=CARTESIAN_POINT('Ctrl Pts',(3.89518058467149,-3.35199940104307,14.0011206394089));
#10269=CARTESIAN_POINT('Ctrl Pts',(3.7964157426101,-3.46346172331502,13.9930539861594));
#10270=CARTESIAN_POINT('Ctrl Pts',(3.6929939900547,-3.57043358038206,13.9849873329099));
#10271=CARTESIAN_POINT('Ctrl Pts',(3.5895685092155,-3.67740929371177,13.9769203888631));
#10272=CARTESIAN_POINT('Ctrl Pts',(3.48148600929417,-3.7798939773071,13.9688534448163));
#10273=CARTESIAN_POINT('Ctrl Pts',(3.36916048297568,-3.87749380430906,13.9607865007695));
#10274=CARTESIAN_POINT('Ctrl Pts',(3.25684175138037,-3.97508772736532,13.952720044703));
#10275=CARTESIAN_POINT('Ctrl Pts',(3.14028075728999,-4.06779716848725,13.9446535886365));
#10276=CARTESIAN_POINT('Ctrl Pts',(3.01992556597796,-4.15526775773267,13.9365871325701));
#10277=CARTESIAN_POINT('Ctrl Pts',(2.89954033873187,-4.24276017620558,13.9285186634326));
#10278=CARTESIAN_POINT('Ctrl Pts',(2.7753592897203,-4.325010935101,13.9204501942952));
#10279=CARTESIAN_POINT('Ctrl Pts',(2.64786108462242,-4.40170787752234,13.9123817251578));
#10280=CARTESIAN_POINT('Ctrl Pts',(2.55339619968378,-4.45853352330625,13.9064037036781));
#10281=CARTESIAN_POINT('Ctrl Pts',(2.45711101131606,-4.51231127016196,13.9004256821984));
#10282=CARTESIAN_POINT('Ctrl Pts',(2.3592095547749,-4.56293007169284,13.8944476607187));
#10283=CARTESIAN_POINT('Ctrl Pts',(2.22707611919215,-4.63124811707906,13.8863793791628));
#10284=CARTESIAN_POINT('Ctrl Pts',(2.09194872668348,-4.69383545006435,13.878311097607));
#10285=CARTESIAN_POINT('Ctrl Pts',(1.95434308261613,-4.75044668193745,13.8702428160512));
#10286=CARTESIAN_POINT('Ctrl Pts',(1.81676520953644,-4.80704648877175,13.8621761628017));
#10287=CARTESIAN_POINT('Ctrl Pts',(1.67671038864624,-4.85767247477758,13.8541095095522));
#10288=CARTESIAN_POINT('Ctrl Pts',(1.53471458296422,-4.90212726388626,13.8460428563028));
#10289=CARTESIAN_POINT('Ctrl Pts',(1.3927136584301,-4.94658365555981,13.8379759122559));
#10290=CARTESIAN_POINT('Ctrl Pts',(1.24877192383751,-4.98486830265642,13.8299089682091));
#10291=CARTESIAN_POINT('Ctrl Pts',(1.10344133525766,-5.0168334417384,13.8218420241623));
#10292=CARTESIAN_POINT('Ctrl Pts',(0.958119537921845,-5.04879664720586,
13.8137755680959));
#10293=CARTESIAN_POINT('Ctrl Pts',(0.811409378153299,-5.07444103912968,
13.8057091120294));
#10294=CARTESIAN_POINT('Ctrl Pts',(0.663873854709686,-5.0936698035437,13.7976426559629));
#10295=CARTESIAN_POINT('Ctrl Pts',(0.516301512187403,-5.11290336670295,
13.7895741868255));
#10296=CARTESIAN_POINT('Ctrl Pts',(0.367903722721964,-5.12571805960758,
13.7815057176881));
#10297=CARTESIAN_POINT('Ctrl Pts',(0.21925016013056,-5.13206877679779,13.7734372485507));
#10298=CARTESIAN_POINT('Ctrl Pts',(0.10911102777809,-5.13677409612517,13.7674592270709));
#10299=CARTESIAN_POINT('Ctrl Pts',(-0.00116835654856688,-5.13793208944069,
13.7614812055912));
#10300=CARTESIAN_POINT('Ctrl Pts',(-0.111355696321223,-5.13554286043811,
13.7555031841115));
#10301=CARTESIAN_POINT('Ctrl Pts',(-0.26007086641402,-5.13231821958333,
13.7474349025556));
#10302=CARTESIAN_POINT('Ctrl Pts',(-0.408673367827961,-5.12262889401346,
13.7393666209998));
#10303=CARTESIAN_POINT('Ctrl Pts',(-0.5565929450814,-5.10650613002527,13.7312983394439));
#10304=CARTESIAN_POINT('Ctrl Pts',(-0.704482669832755,-5.09038661986495,
13.7232316861944));
#10305=CARTESIAN_POINT('Ctrl Pts',(-0.851689416522729,-5.06783629741423,
13.715165032945));
#10306=CARTESIAN_POINT('Ctrl Pts',(-0.997648111549489,-5.03893826197759,
13.7070983796955));
#10307=CARTESIAN_POINT('Ctrl Pts',(-1.14361206828793,-5.01003918478643,
13.6990314356487));
#10308=CARTESIAN_POINT('Ctrl Pts',(-1.28832755789921,-4.97479199727496,
13.6909644916018));
#10309=CARTESIAN_POINT('Ctrl Pts',(-1.43123919899822,-4.93333101643818,
13.682897547555));
#10310=CARTESIAN_POINT('Ctrl Pts',(-1.57414219517855,-4.89187254363226,
13.6748310914886));
#10311=CARTESIAN_POINT('Ctrl Pts',(-1.71524124345498,-4.8442011225082,13.6667646354221));
#10312=CARTESIAN_POINT('Ctrl Pts',(-1.8539956412884,-4.79050109326609,13.6586981793556));
#10313=CARTESIAN_POINT('Ctrl Pts',(-1.99278466677606,-4.73678766260338,
13.6506297102182));
#10314=CARTESIAN_POINT('Ctrl Pts',(-2.12922756351663,-4.67704273644587,
13.6425612410808));
#10315=CARTESIAN_POINT('Ctrl Pts',(-2.26280250628869,-4.61149925512665,
13.6344927719433));
#10316=CARTESIAN_POINT('Ctrl Pts',(-2.36176971598311,-4.56293733681169,
13.6285147504636));
#10317=CARTESIAN_POINT('Ctrl Pts',(-2.45916294008812,-4.51119331827604,
13.622536728984));
#10318=CARTESIAN_POINT('Ctrl Pts',(-2.5547782425683,-4.45637842802871,13.6165587075043));
#10319=CARTESIAN_POINT('Ctrl Pts',(-2.68382615316517,-4.38239710001397,
13.6084904259485));
#10320=CARTESIAN_POINT('Ctrl Pts',(-2.80968223221986,-4.30279286758047,
13.6004221443926));
#10321=CARTESIAN_POINT('Ctrl Pts',(-2.93186067264955,-4.21786599581719,
13.5923538628368));
#10322=CARTESIAN_POINT('Ctrl Pts',(-3.05401445554449,-4.13295626363504,
13.5842872095874));
#10323=CARTESIAN_POINT('Ctrl Pts',(-3.17249180889903,-4.04272622398234,
13.5762205563379));
#10324=CARTESIAN_POINT('Ctrl Pts',(-3.28683628396969,-3.94751919626496,
13.5681539030885));
#10325=CARTESIAN_POINT('Ctrl Pts',(-3.40118488108078,-3.85230873639908,
13.5600869590417));
#10326=CARTESIAN_POINT('Ctrl Pts',(-3.51140004498186,-3.75212113832894,
13.5520200149948));
#10327=CARTESIAN_POINT('Ctrl Pts',(-3.61705834195898,-3.64734006001153,
13.543953070948));
#10328=CARTESIAN_POINT('Ctrl Pts',(-3.72271024752267,-3.54256532004342,
13.5358866148816));
#10329=CARTESIAN_POINT('Ctrl Pts',(-3.82380560316017,-3.43319788940275,
13.5278201588152));
#10330=CARTESIAN_POINT('Ctrl Pts',(-3.91995779759971,-3.31965832993958,
13.5197537027487));
#10331=CARTESIAN_POINT('Ctrl Pts',(-4.01613398785483,-3.20609043545664,
13.5116852336113));
#10332=CARTESIAN_POINT('Ctrl Pts',(-4.10736433736911,-3.08834858393419,
13.5036167644739));
#10333=CARTESIAN_POINT('Ctrl Pts',(-4.19330206326122,-2.96688698280693,
13.4955482953365));
#10334=CARTESIAN_POINT('Ctrl Pts',(-4.25697431168338,-2.87689468710158,
13.4895702738567));
#10335=CARTESIAN_POINT('Ctrl Pts',(-4.31774199246088,-2.78486114686199,
13.4835922523769));
#10336=CARTESIAN_POINT('Ctrl Pts',(-4.37547923900897,-2.69098160370923,
13.4776142308972));
#10337=CARTESIAN_POINT('Ctrl Pts',(-4.45340474713679,-2.56427637371713,
13.4695459493413));
#10338=CARTESIAN_POINT('Ctrl Pts',(-4.5258372627426,-2.4341605901263,13.4614776677855));
#10339=CARTESIAN_POINT('Ctrl Pts',(-4.59249384154503,-2.30113034786624,
13.4534093862297));
#10340=CARTESIAN_POINT('Ctrl Pts',(-4.65913696799926,-2.1681269532058,13.4453427329802));
#10341=CARTESIAN_POINT('Ctrl Pts',(-4.72000633500855,-2.03221056908114,
13.4372760797307));
#10342=CARTESIAN_POINT('Ctrl Pts',(-4.77486537706007,-1.89390105165317,
13.4292094264813));
#10343=CARTESIAN_POINT('Ctrl Pts',(-4.82972639674276,-1.75558654826113,
13.4211424824344));
#10344=CARTESIAN_POINT('Ctrl Pts',(-4.87857653234138,-1.61487904521717,
13.4130755383876));
#10345=CARTESIAN_POINT('Ctrl Pts',(-4.92122750884501,-1.47231802566128,
13.4050085943408));
#10346=CARTESIAN_POINT('Ctrl Pts',(-4.96387590533327,-1.32976562981468,
13.3969421382743));
#10347=CARTESIAN_POINT('Ctrl Pts',(-5.00032579884621,-1.18536025914133,
13.3888756822079));
#10348=CARTESIAN_POINT('Ctrl Pts',(-5.03043890502238,-1.03965618611985,
13.3808092261414));
#10349=CARTESIAN_POINT('Ctrl Pts',(-5.06055952624849,-0.893915751077784,
13.372740757004));
#10350=CARTESIAN_POINT('Ctrl Pts',(-5.08434013248878,-0.746876290254184,
13.3646722878666));
#10351=CARTESIAN_POINT('Ctrl Pts',(-5.10169351076287,-0.599102566127044,
13.3566038187291));
#10352=CARTESIAN_POINT('Ctrl Pts',(-5.11455082809301,-0.489615316200809,
13.3506257972494));
#10353=CARTESIAN_POINT('Ctrl Pts',(-5.12388097766677,-0.379725226270334,
13.3446477757697));
#10354=CARTESIAN_POINT('Ctrl Pts',(-5.12966684205185,-0.269663961355155,
13.3386697542899));
#10355=CARTESIAN_POINT('Ctrl Pts',(-5.13438618858459,-0.179890469548952,
13.3337936712943));
#10356=CARTESIAN_POINT('Ctrl Pts',(-5.13674848218115,-0.0899925721050492,
13.3289175882987));
#10357=CARTESIAN_POINT('Ctrl Pts',(-5.13674999926869,-8.66784045078238E-5,
13.3240415053031));
#10358=CARTESIAN_POINT('Ctrl Pts',(-5.13674999942792,-7.66631357963787E-5,
13.3242245870723));
#10359=CARTESIAN_POINT('Ctrl Pts',(-5.13675482000189,0.322921907747067,
13.3065553374322));
#10360=CARTESIAN_POINT('Ctrl Pts',(-5.10629412606806,0.645211665566582,
13.2888158745499));
#10361=CARTESIAN_POINT('Ctrl Pts',(-5.0354960278084,1.01635935148288,13.2683148233289));
#10362=CARTESIAN_POINT('Ctrl Pts',(-5.02436109757278,1.0700477581446,13.2653458440043));
#10363=CARTESIAN_POINT('Ctrl Pts',(-4.93693907417981,1.46005464630582,13.2437409801159));
#10364=CARTESIAN_POINT('Ctrl Pts',(-4.8278152561397,1.78810590632312,13.2254297836528));
#10365=CARTESIAN_POINT('Ctrl Pts',(-4.65003687406371,2.18434367576704,13.201989082554));
#10366=CARTESIAN_POINT('Ctrl Pts',(-4.61130000993693,2.26497503841401,13.1971366758318));
#10367=CARTESIAN_POINT('Ctrl Pts',(-4.48624034085036,2.50876666159917,13.1821954669199));
#10368=CARTESIAN_POINT('Ctrl Pts',(-4.3932231057094,2.66830254988752,13.1720601586962));
#10369=CARTESIAN_POINT('Ctrl Pts',(-4.29183623954907,2.82247094854728,13.1619495546845));
#10370=CARTESIAN_POINT('Origin',(0.,0.,0.));
#10371=CARTESIAN_POINT('',(-4.29183622844418,2.82247096543331,11.4121712634621));
#10372=CARTESIAN_POINT('',(-4.29155726418515,2.82228712074135,11.8889308194183));
#10373=CARTESIAN_POINT('',(-4.29183622825304,2.82247096572397,0.));
#10374=CARTESIAN_POINT('',(-5.13674999832603,-0.000131139391237522,12.0509584946969));
#10375=CARTESIAN_POINT('Ctrl Pts',(-4.29155726418515,2.82228712074135,11.8889308194183));
#10376=CARTESIAN_POINT('Ctrl Pts',(-4.46838982832423,2.55377308187227,11.9063606652066));
#10377=CARTESIAN_POINT('Ctrl Pts',(-4.9388247281808,1.67089962616198,11.9603698894268));
#10378=CARTESIAN_POINT('Ctrl Pts',(-5.13610861091696,0.674465849271032,
12.014379113647));
#10379=CARTESIAN_POINT('Ctrl Pts',(-5.13680565136043,-0.00013109253210184,
12.050958492079));
#10380=CARTESIAN_POINT('Ctrl Pts',(-5.13674999832603,-0.000131139391237522,
12.0509584946969));
#10381=CARTESIAN_POINT('Ctrl Pts',(-5.13674597131034,-0.157869959281706,
12.0595118252836));
#10382=CARTESIAN_POINT('Ctrl Pts',(-5.12947186524448,-0.315573404970336,
12.0680651558703));
#10383=CARTESIAN_POINT('Ctrl Pts',(-5.11496338830488,-0.472599300465667,
12.076618486457));
#10384=CARTESIAN_POINT('Ctrl Pts',(-5.11295823985499,-0.494301111913994,
12.0778006021015));
#10385=CARTESIAN_POINT('Ctrl Pts',(-5.11081499098403,-0.515989987668825,
12.0789827177459));
#10386=CARTESIAN_POINT('Ctrl Pts',(-5.10853381397671,-0.537664239053161,
12.0801648333904));
#10387=CARTESIAN_POINT('Ctrl Pts',(-5.09296412038498,-0.685597280548789,
12.0882331149463));
#10388=CARTESIAN_POINT('Ctrl Pts',(-5.07096145592205,-0.832880915801725,
12.0963013965022));
#10389=CARTESIAN_POINT('Ctrl Pts',(-5.04260433929914,-0.978949457214977,
12.1043696780582));
#10390=CARTESIAN_POINT('Ctrl Pts',(-5.0142529455893,-1.12498851969439,12.1124363313077));
#10391=CARTESIAN_POINT('Ctrl Pts',(-4.97954972124561,-1.26981265281502,
12.1205029845572));
#10392=CARTESIAN_POINT('Ctrl Pts',(-4.93862442815397,-1.41286564122031,
12.1285696378067));
#10393=CARTESIAN_POINT('Ctrl Pts',(-4.89769765973334,-1.55592378658856,
12.1366365818536));
#10394=CARTESIAN_POINT('Ctrl Pts',(-4.85054846112362,-1.697210340201,12.1447035259005));
#10395=CARTESIAN_POINT('Ctrl Pts',(-4.79735682951735,-1.83618300089704,
12.1527704699474));
#10396=CARTESIAN_POINT('Ctrl Pts',(-4.7441684155448,-1.97514725494891,12.1608369260139));
#10397=CARTESIAN_POINT('Ctrl Pts',(-4.68493841891923,-2.11179758724498,
12.1689033820804));
#10398=CARTESIAN_POINT('Ctrl Pts',(-4.61989546746367,-2.24561048096251,
12.1769698381469));
#10399=CARTESIAN_POINT('Ctrl Pts',(-4.55483628383924,-2.37945676912844,
12.1850383072844));
#10400=CARTESIAN_POINT('Ctrl Pts',(-4.48396139081855,-2.5104639056216,12.1931067764219));
#10401=CARTESIAN_POINT('Ctrl Pts',(-4.40754627986778,-2.638131223674,12.2011752455594));
#10402=CARTESIAN_POINT('Ctrl Pts',(-4.35092944626179,-2.73272140633764,
12.2071532670387));
#10403=CARTESIAN_POINT('Ctrl Pts',(-4.29127229175841,-2.82547865657246,
12.2131312885181));
#10404=CARTESIAN_POINT('Ctrl Pts',(-4.22870260458065,-2.91620898505453,
12.2191093099975));
#10405=CARTESIAN_POINT('Ctrl Pts',(-4.14425495668391,-3.03866385383857,
12.2271775915533));
#10406=CARTESIAN_POINT('Ctrl Pts',(-4.05446904407064,-3.15747074064452,
12.2352458731091));
#10407=CARTESIAN_POINT('Ctrl Pts',(-3.95968445756145,-3.2721704660739,12.2433141546649));
#10408=CARTESIAN_POINT('Ctrl Pts',(-3.86491900007579,-3.38684704329083,
12.2513808079144));
#10409=CARTESIAN_POINT('Ctrl Pts',(-3.76515709203226,-3.49741785778094,
12.2594474611638));
#10410=CARTESIAN_POINT('Ctrl Pts',(-3.66077879042398,-3.60345656420081,
12.2675141144133));
#10411=CARTESIAN_POINT('Ctrl Pts',(-3.55639672604888,-3.70949909324397,
12.2755810584601));
#10412=CARTESIAN_POINT('Ctrl Pts',(-3.44739816459536,-3.81100894873496,
12.2836480025069));
#10413=CARTESIAN_POINT('Ctrl Pts',(-3.33420061903242,-3.90759603778894,
12.2917149465537));
#10414=CARTESIAN_POINT('Ctrl Pts',(-3.22100992094223,-4.00417728415917,
12.2997814026201));
#10415=CARTESIAN_POINT('Ctrl Pts',(-3.10362099924908,-4.09583614559698,
12.3078478586866));
#10416=CARTESIAN_POINT('Ctrl Pts',(-2.98248508377152,-4.18222229055085,
12.315914314753));
#10417=CARTESIAN_POINT('Ctrl Pts',(-2.86131893752182,-4.26862999409742,
12.3239827838904));
#10418=CARTESIAN_POINT('Ctrl Pts',(-2.73640419822553,-4.3497621589822,12.3320512530278));
#10419=CARTESIAN_POINT('Ctrl Pts',(-2.60822231575517,-4.4253109398207,12.3401197221653));
#10420=CARTESIAN_POINT('Ctrl Pts',(-2.51325088639444,-4.48128589949841,
12.3460977436451));
#10421=CARTESIAN_POINT('Ctrl Pts',(-2.41648660036535,-4.53419673492632,
12.3520757651249));
#10422=CARTESIAN_POINT('Ctrl Pts',(-2.31813448200849,-4.58393423663814,
12.3580537866048));
#10423=CARTESIAN_POINT('Ctrl Pts',(-2.18539280732642,-4.65106282910802,
12.3661220681606));
#10424=CARTESIAN_POINT('Ctrl Pts',(-2.04970876430788,-4.71243405140835,
12.3741903497165));
#10425=CARTESIAN_POINT('Ctrl Pts',(-1.9116002413709,-4.76780715630265,12.3822586312723));
#10426=CARTESIAN_POINT('Ctrl Pts',(-1.77351959091066,-4.8231690860316,12.3903252845218));
#10427=CARTESIAN_POINT('Ctrl Pts',(-1.63301574374822,-4.87253519025532,
12.3983919377713));
#10428=CARTESIAN_POINT('Ctrl Pts',(-1.49062641393189,-4.9157129143786,12.4064585910207));
#10429=CARTESIAN_POINT('Ctrl Pts',(-1.348231951077,-4.95889219502949,12.4145255350676));
#10430=CARTESIAN_POINT('Ctrl Pts',(-1.20395218521327,-4.99588254949151,
12.4225924791144));
#10431=CARTESIAN_POINT('Ctrl Pts',(-1.05834037722278,-5.02654117743404,
12.4306594231612));
#10432=CARTESIAN_POINT('Ctrl Pts',(-0.912737377487716,-5.05719795079465,
12.4387258792277));
#10433=CARTESIAN_POINT('Ctrl Pts',(-0.765802820923515,-5.08152369649344,
12.4467923352941));
#10434=CARTESIAN_POINT('Ctrl Pts',(-0.61810055307335,-5.09942666079143,
12.4548587913606));
#10435=CARTESIAN_POINT('Ctrl Pts',(-0.470361424531666,-5.11733409296695,
12.462927260498));
#10436=CARTESIAN_POINT('Ctrl Pts',(-0.321854530562556,-5.12881550037983,
12.4709957296355));
#10437=CARTESIAN_POINT('Ctrl Pts',(-0.173149927102597,-5.13383089566109,
12.4790641987729));
#10438=CARTESIAN_POINT('Ctrl Pts',(-0.062972977985472,-5.13754685964505,
12.4850422202526));
#10439=CARTESIAN_POINT('Ctrl Pts',(0.0473123587203552,-5.13771438107194,
12.4910202417323));
#10440=CARTESIAN_POINT('Ctrl Pts',(0.157473796786609,-5.13433564989918,
12.4969982632119));
#10441=CARTESIAN_POINT('Ctrl Pts',(0.306154008448005,-5.12977552001405,
12.5050665447678));
#10442=CARTESIAN_POINT('Ctrl Pts',(0.454663496287294,-5.11875197802132,
12.5131348263236));
#10443=CARTESIAN_POINT('Ctrl Pts',(0.602432308446221,-5.10130139045324,
12.5212031078794));
#10444=CARTESIAN_POINT('Ctrl Pts',(0.750171298529824,-5.08385432468878,
12.5292697611289));
#10445=CARTESIAN_POINT('Ctrl Pts',(0.897169582619754,-5.05998283985507,
12.5373364143783));
#10446=CARTESIAN_POINT('Ctrl Pts',(1.04286285622328,-5.02977510686212,12.5454030676277));
#10447=CARTESIAN_POINT('Ctrl Pts',(1.18856138197026,-4.99956628490093,12.5534700116746));
#10448=CARTESIAN_POINT('Ctrl Pts',(1.33295447821516,-4.96302082119344,12.5615369557214));
#10449=CARTESIAN_POINT('Ctrl Pts',(1.47548799227996,-4.92027801522817,12.5696038997682));
#10450=CARTESIAN_POINT('Ctrl Pts',(1.61801288429949,-4.87753779483311,12.5776703558346));
#10451=CARTESIAN_POINT('Ctrl Pts',(1.75867810234035,-4.82860107804601,12.5857368119011));
#10452=CARTESIAN_POINT('Ctrl Pts',(1.89694462123966,-4.77365705371154,12.5938032679675));
#10453=CARTESIAN_POINT('Ctrl Pts',(2.03524564603772,-4.71869931750411,12.6018717371049));
#10454=CARTESIAN_POINT('Ctrl Pts',(2.17114646751808,-4.65773139976573,12.6099402062423));
#10455=CARTESIAN_POINT('Ctrl Pts',(2.30412737355467,-4.59099091797578,12.6180086753798));
#10456=CARTESIAN_POINT('Ctrl Pts',(2.40265445460921,-4.54154212825909,12.6239866968596));
#10457=CARTESIAN_POINT('Ctrl Pts',(2.49957903493763,-4.48892550270796,12.6299647183393));
#10458=CARTESIAN_POINT('Ctrl Pts',(2.5946981856787,-4.43325409690621,12.6359427398191));
#10459=CARTESIAN_POINT('Ctrl Pts',(2.72307646135506,-4.35811676624644,12.644011021375));
#10460=CARTESIAN_POINT('Ctrl Pts',(2.84821253460503,-4.27738542395611,12.6520793029308));
#10461=CARTESIAN_POINT('Ctrl Pts',(2.96962331463579,-4.1913646860744,12.6601475844867));
#10462=CARTESIAN_POINT('Ctrl Pts',(3.09100959205767,-4.10536130853331,12.6682142377361));
#10463=CARTESIAN_POINT('Ctrl Pts',(3.20867180623876,-4.01407085630716,12.6762808909856));
#10464=CARTESIAN_POINT('Ctrl Pts',(3.32215661021474,-3.91784073434673,12.684347544235));
#10465=CARTESIAN_POINT('Ctrl Pts',(3.43564550524069,-3.82160714335588,12.6924144882819));
#10466=CARTESIAN_POINT('Ctrl Pts',(3.54495643380937,-3.72043373748103,12.7004814323287));
#10467=CARTESIAN_POINT('Ctrl Pts',(3.64966942493724,-3.61470796208743,12.7085483763755));
#10468=CARTESIAN_POINT('Ctrl Pts',(3.75437608183454,-3.5089885821891,12.716614832442));
#10469=CARTESIAN_POINT('Ctrl Pts',(3.85448512536721,-3.39871761946791,12.7246812885084));
#10470=CARTESIAN_POINT('Ctrl Pts',(3.94961373694471,-3.28431909098944,12.7327477445749));
#10471=CARTESIAN_POINT('Ctrl Pts',(4.04476608889159,-3.1698920131263,12.7408162137123));
#10472=CARTESIAN_POINT('Ctrl Pts',(4.13493531302918,-3.05133556542775,12.7488846828497));
#10473=CARTESIAN_POINT('Ctrl Pts',(4.21977871972388,-2.92910705148608,12.7569531519872));
#10474=CARTESIAN_POINT('Ctrl Pts',(4.2826401744799,-2.8385465412665,12.7629311734669));
#10475=CARTESIAN_POINT('Ctrl Pts',(4.34257884620506,-2.74597095491807,12.7689091949466));
#10476=CARTESIAN_POINT('Ctrl Pts',(4.39947062686654,-2.65157665660236,12.7748872164263));
#10477=CARTESIAN_POINT('Ctrl Pts',(4.47625504561576,-2.52417668344032,12.7829554979822));
#10478=CARTESIAN_POINT('Ctrl Pts',(4.54751606300949,-2.39341562709532,12.791023779538));
#10479=CARTESIAN_POINT('Ctrl Pts',(4.61297520163336,-2.25979210362715,12.7990920610938));
#10480=CARTESIAN_POINT('Ctrl Pts',(4.67842112957137,-2.12619554749205,12.8071587143433));
#10481=CARTESIAN_POINT('Ctrl Pts',(4.73806736920513,-1.98973797382458,12.8152253675928));
#10482=CARTESIAN_POINT('Ctrl Pts',(4.79168203341927,-1.8509413424274,12.8232920208422));
#10483=CARTESIAN_POINT('Ctrl Pts',(4.84529863040559,-1.71213970750606,12.831358964889));
#10484=CARTESIAN_POINT('Ctrl Pts',(4.89288309406887,-1.57099915352256,12.8394259089359));
#10485=CARTESIAN_POINT('Ctrl Pts',(4.93425200211901,-1.42806083276747,12.8474928529827));
#10486=CARTESIAN_POINT('Ctrl Pts',(4.9756184077079,-1.28513115854491,12.8555593090491));
#10487=CARTESIAN_POINT('Ctrl Pts',(5.01076991864176,-1.14040425332142,12.8636257651156));
#10488=CARTESIAN_POINT('Ctrl Pts',(5.03957323408765,-0.994435609160971,
12.871692221182));
#10489=CARTESIAN_POINT('Ctrl Pts',(5.06838373771108,-0.848430536953496,
12.8797606903195));
#10490=CARTESIAN_POINT('Ctrl Pts',(5.09084281542292,-0.701183431376395,
12.8878291594569));
#10491=CARTESIAN_POINT('Ctrl Pts',(5.10686832992285,-0.553259815395071,
12.8958976285944));
#10492=CARTESIAN_POINT('Ctrl Pts',(5.11874181772727,-0.443661508872842,
12.901875650074));
#10493=CARTESIAN_POINT('Ctrl Pts',(5.12708466209961,-0.333692056279775,
12.9078536715537));
#10494=CARTESIAN_POINT('Ctrl Pts',(5.13188182689416,-0.223583267024828,
12.9138316930334));
#10495=CARTESIAN_POINT('Ctrl Pts',(5.13835635636243,-0.074974113227048,
12.9218999745893));
#10496=CARTESIAN_POINT('Ctrl Pts',(5.13837260241816,0.0739439387092463,
12.9299682561451));
#10497=CARTESIAN_POINT('Ctrl Pts',(5.13192457927966,0.222599809266103,12.938036537701));
#10498=CARTESIAN_POINT('Ctrl Pts',(5.12547785745385,0.371225678725344,12.9461031909504));
#10499=CARTESIAN_POINT('Ctrl Pts',(5.11256948346549,0.51958914186445,12.9541698441999));
#10500=CARTESIAN_POINT('Ctrl Pts',(5.09324555201993,0.667120910577073,12.9622364974493));
#10501=CARTESIAN_POINT('Ctrl Pts',(5.07392092395979,0.814657997709612,12.9703034414962));
#10502=CARTESIAN_POINT('Ctrl Pts',(5.04818031487552,0.961363001730773,12.978370385543));
#10503=CARTESIAN_POINT('Ctrl Pts',(5.01612155994829,1.1066729680994,12.9864373295898));
#10504=CARTESIAN_POINT('Ctrl Pts',(4.98406474429854,1.25197414447146,12.9945037856563));
#10505=CARTESIAN_POINT('Ctrl Pts',(4.94569061953874,1.39588012893846,13.0025702417228));
#10506=CARTESIAN_POINT('Ctrl Pts',(4.90114789437699,1.53783935440083,13.0106366977892));
#10507=CARTESIAN_POINT('Ctrl Pts',(4.85659405309853,1.67983400731659,13.0187051669267));
#10508=CARTESIAN_POINT('Ctrl Pts',(4.80586863383362,1.81988061424758,13.0267736360641));
#10509=CARTESIAN_POINT('Ctrl Pts',(4.74917007240058,1.95744327782818,13.0348421052015));
#10510=CARTESIAN_POINT('Ctrl Pts',(4.70716145684518,2.05936503568366,13.0408201266812));
#10511=CARTESIAN_POINT('Ctrl Pts',(4.66187492398926,2.15992354351756,13.0467981481609));
#10512=CARTESIAN_POINT('Ctrl Pts',(4.61340817460148,2.25890804970459,13.0527761696406));
#10513=CARTESIAN_POINT('Ctrl Pts',(4.54799466254168,2.39250323137016,13.0608444511965));
#10514=CARTESIAN_POINT('Ctrl Pts',(4.47676217731939,2.52327983289129,13.0689127327523));
#10515=CARTESIAN_POINT('Ctrl Pts',(4.39997868380664,2.65073351066214,13.0769810143081));
#10516=CARTESIAN_POINT('Ctrl Pts',(4.3232106864131,2.77816146627195,13.0850476675576));
#10517=CARTESIAN_POINT('Ctrl Pts',(4.24089408643114,2.90226755266968,13.093114320807));
#10518=CARTESIAN_POINT('Ctrl Pts',(4.15334172490436,3.02257391616292,13.1011809740565));
#10519=CARTESIAN_POINT('Ctrl Pts',(4.06578620717445,3.1428846166188,13.1092479181033));
#10520=CARTESIAN_POINT('Ctrl Pts',(3.97299474191275,3.25939505020903,13.1173148621501));
#10521=CARTESIAN_POINT('Ctrl Pts',(3.8753225746625,3.37165767906696,13.1253818061969));
#10522=CARTESIAN_POINT('Ctrl Pts',(3.77765631573385,3.48391351700653,13.1334482622634));
#10523=CARTESIAN_POINT('Ctrl Pts',(3.67511016337259,3.59192181507812,13.1415147183298));
#10524=CARTESIAN_POINT('Ctrl Pts',(3.56807858840896,3.69526937440798,13.1495811743962));
#10525=CARTESIAN_POINT('Ctrl Pts',(3.46102030256325,3.79864272523414,13.1576496435337));
#10526=CARTESIAN_POINT('Ctrl Pts',(3.34947459514941,3.89735278262419,13.1657181126711));
#10527=CARTESIAN_POINT('Ctrl Pts',(3.23387210681231,3.99102389861065,13.1737865818085));
#10528=CARTESIAN_POINT('Ctrl Pts',(3.14822089508619,4.06042590460018,13.1797646032883));
#10529=CARTESIAN_POINT('Ctrl Pts',(3.06034347728788,4.12706255365521,13.1857426247681));
#10530=CARTESIAN_POINT('Ctrl Pts',(2.97042647675405,4.19079552217697,13.1917206462478));
#10531=CARTESIAN_POINT('Ctrl Pts',(2.84906932214722,4.27681320146484,13.1997889278037));
#10532=CARTESIAN_POINT('Ctrl Pts',(2.72395086647462,4.35757184500561,13.2078572093595));
#10533=CARTESIAN_POINT('Ctrl Pts',(2.59554770941672,4.43275677774471,13.2159254909154));
#10534=CARTESIAN_POINT('Ctrl Pts',(2.46717046613967,4.50792653697939,13.2239921441648));
#10535=CARTESIAN_POINT('Ctrl Pts',(2.33551012946518,4.57752466238813,13.2320587974143));
#10536=CARTESIAN_POINT('Ctrl Pts',(2.20107003246214,4.6412812104738,13.2401254506638));
#10537=CARTESIAN_POINT('Ctrl Pts',(2.06662508898502,4.70504005693967,13.2481923947106));
#10538=CARTESIAN_POINT('Ctrl Pts',(1.92940048210627,4.76295675943438,13.2562593387574));
#10539=CARTESIAN_POINT('Ctrl Pts',(1.78992227741529,4.81480828313158,13.2643262828042));
#10540=CARTESIAN_POINT('Ctrl Pts',(1.65045250994969,4.86665667025993,13.2723927388707));
#10541=CARTESIAN_POINT('Ctrl Pts',(1.50872972796709,4.91244049801187,13.2804591949372));
#10542=CARTESIAN_POINT('Ctrl Pts',(1.36529801302686,4.9519856520516,13.2885256510036));
#10543=CARTESIAN_POINT('Ctrl Pts',(1.22183050315766,4.99154067501036,13.2965941201411));
#10544=CARTESIAN_POINT('Ctrl Pts',(1.07665352722731,5.02485382454942,13.3046625892785));
#10545=CARTESIAN_POINT('Ctrl Pts',(0.93032496300189,5.05180126546121,13.3127310584159));
#10546=CARTESIAN_POINT('Ctrl Pts',(0.82190844865043,5.07176693402233,13.3187090798956));
#10547=CARTESIAN_POINT('Ctrl Pts',(0.712860072264733,5.08823918837666,13.3246871013753));
#10548=CARTESIAN_POINT('Ctrl Pts',(0.603409890723613,5.10118584902343,13.330665122855));
#10549=CARTESIAN_POINT('Ctrl Pts',(0.455689631769934,5.11865940673158,13.3387334044109));
#10550=CARTESIAN_POINT('Ctrl Pts',(0.307182552668397,5.12971535142931,13.3468016859667));
#10551=CARTESIAN_POINT('Ctrl Pts',(0.158457717789245,5.13430537796234,13.3548699675226));
#10552=CARTESIAN_POINT('Ctrl Pts',(0.00976289792575968,5.13889447815568,
13.362936620772));
#10553=CARTESIAN_POINT('Ctrl Pts',(-0.139149259385165,5.13702025333934,
13.3710032740215));
#10554=CARTESIAN_POINT('Ctrl Pts',(-0.287707615372341,5.12868646834224,
13.379069927271));
#10555=CARTESIAN_POINT('Ctrl Pts',(-0.436271326787243,5.12035238291785,
13.3871368713178));
#10556=CARTESIAN_POINT('Ctrl Pts',(-0.584480880663312,5.10555828609689,
13.3952038153646));
#10557=CARTESIAN_POINT('Ctrl Pts',(-0.731767618689695,5.08436001033928,
13.4032707594114));
#10558=CARTESIAN_POINT('Ctrl Pts',(-0.879045447141863,5.06316301689407,
13.4113372154779));
#10559=CARTESIAN_POINT('Ctrl Pts',(-1.02540024388673,5.03556266750755,13.4194036715444));
#10560=CARTESIAN_POINT('Ctrl Pts',(-1.1702709353133,5.00166637236641,13.4274701276108));
#10561=CARTESIAN_POINT('Ctrl Pts',(-1.31517778078097,4.9677616180398,13.4355385967483));
#10562=CARTESIAN_POINT('Ctrl Pts',(-1.4585994582288,4.92755785315958,13.4436070658857));
#10563=CARTESIAN_POINT('Ctrl Pts',(-1.59998683424193,4.88121323983623,13.4516755350231));
#10564=CARTESIAN_POINT('Ctrl Pts',(-1.70474236547937,4.84687598338817,13.4576535565028));
#10565=CARTESIAN_POINT('Ctrl Pts',(-1.8083813997389,4.8091687674524,13.4636315779825));
#10566=CARTESIAN_POINT('Ctrl Pts',(-1.91068652245528,4.76817340030831,13.4696095994622));
#10567=CARTESIAN_POINT('Ctrl Pts',(-2.04876339914168,4.71284369536714,13.4776778810181));
#10568=CARTESIAN_POINT('Ctrl Pts',(-2.18446082938609,4.65150207913866,13.4857461625739));
#10569=CARTESIAN_POINT('Ctrl Pts',(-2.31725599231094,4.5843783906435,13.4938144441298));
#10570=CARTESIAN_POINT('Ctrl Pts',(-2.45002435507905,4.51726824876654,13.5018810973793));
#10571=CARTESIAN_POINT('Ctrl Pts',(-2.57989132382215,4.44437851188141,13.5099477506287));
#10572=CARTESIAN_POINT('Ctrl Pts',(-2.70635716787987,4.36598573547432,13.5180144038782));
#10573=CARTESIAN_POINT('Ctrl Pts',(-2.83282757094512,4.28759013306104,13.526081347925));
#10574=CARTESIAN_POINT('Ctrl Pts',(-2.95589632064838,4.20369126532515,13.5341482919719));
#10575=CARTESIAN_POINT('Ctrl Pts',(-3.07509077516368,4.11461022297413,13.5422152360187));
#10576=CARTESIAN_POINT('Ctrl Pts',(-3.19427801944507,4.02553456925596,13.5502816920851));
#10577=CARTESIAN_POINT('Ctrl Pts',(-3.30959117273334,3.93127756688894,13.5583481481516));
#10578=CARTESIAN_POINT('Ctrl Pts',(-3.42058892981839,3.83220196958666,13.5664146042181));
#10579=CARTESIAN_POINT('Ctrl Pts',(-3.53161438758902,3.73310164690216,13.5744830733555));
#10580=CARTESIAN_POINT('Ctrl Pts',(-3.63832204968099,3.62918054642988,13.5825515424929));
#10581=CARTESIAN_POINT('Ctrl Pts',(-3.74030537708679,3.52084027593352,13.5906200116304));
#10582=CARTESIAN_POINT('Ctrl Pts',(-3.81586599601171,3.44056972484016,13.5965980331101));
#10583=CARTESIAN_POINT('Ctrl Pts',(-3.88883390261718,3.35787408915469,13.6025760545898));
#10584=CARTESIAN_POINT('Ctrl Pts',(-3.95905731897123,3.2729292243494,13.6085540760694));
#10585=CARTESIAN_POINT('Ctrl Pts',(-4.0538341891485,3.15828358558858,13.6166222988235));
#10586=CARTESIAN_POINT('Ctrl Pts',(-4.14364540353534,3.03949718774696,13.6246905215776));
#10587=CARTESIAN_POINT('Ctrl Pts',(-4.22814182866341,2.91702198126905,13.6327587443317));
#10588=CARTESIAN_POINT('Ctrl Pts',(-4.24972153642287,2.88574279804247,13.6348193035673));
#10589=CARTESIAN_POINT('Ctrl Pts',(-4.2709547958896,2.85422317469389,13.6368798628028));
#10590=CARTESIAN_POINT('Ctrl Pts',(-4.29183622825304,2.82247096572396,13.6389404220384));
#10591=CARTESIAN_POINT('Ctrl Pts',(-4.29183623954907,2.82247094854727,13.1619495546845));
#10592=CARTESIAN_POINT('Ctrl Pts',(-4.27694788375811,2.84511011334144,13.1604648429513));
#10593=CARTESIAN_POINT('Ctrl Pts',(-4.26187904818184,2.86763352754246,13.1589805421803));
#10594=CARTESIAN_POINT('Ctrl Pts',(-4.16093974471724,3.01595400996317,13.1491586060886));
#10595=CARTESIAN_POINT('Ctrl Pts',(-4.06968960576698,3.137997118523,13.1408514072985));
#10596=CARTESIAN_POINT('Ctrl Pts',(-3.77192941324118,3.50136210079973,13.1153590904081));
#10597=CARTESIAN_POINT('Ctrl Pts',(-3.54837648818902,3.72773607014882,13.0984083992163));
#10598=CARTESIAN_POINT('Ctrl Pts',(-3.20264554166019,4.01836621106547,13.0741672541801));
#10599=CARTESIAN_POINT('Ctrl Pts',(-3.09659155107452,4.10064938220204,13.0669512453703));
#10600=CARTESIAN_POINT('Ctrl Pts',(-2.83464457250743,4.28792130895749,13.0494663601919));
#10601=CARTESIAN_POINT('Ctrl Pts',(-2.67597616762272,4.38869330300458,13.0391599348284));
#10602=CARTESIAN_POINT('Ctrl Pts',(-2.31975579620537,4.58841852998751,13.0167674912027));
#10603=CARTESIAN_POINT('Ctrl Pts',(-2.12061153784892,4.68378711199637,13.0047114042907));
#10604=CARTESIAN_POINT('Ctrl Pts',(-1.64006458124989,4.87696655148323,12.9766174890269));
#10605=CARTESIAN_POINT('Ctrl Pts',(-1.35506677707031,4.96370954684383,12.9607238377605));
#10606=CARTESIAN_POINT('Ctrl Pts',(-0.921521330346854,5.05551767954514,
12.9369501121487));
#10607=CARTESIAN_POINT('Ctrl Pts',(-0.777657732610997,5.07963658288696,
12.9291176039509));
#10608=CARTESIAN_POINT('Ctrl Pts',(-0.430106790533545,5.12279168066443,
12.9101078301565));
#10609=CARTESIAN_POINT('Ctrl Pts',(-0.225928294720977,5.13584861424016,
12.8988839253612));
#10610=CARTESIAN_POINT('Ctrl Pts',(0.2024130186388,5.1376430220503,12.8754016531683));
#10611=CARTESIAN_POINT('Ctrl Pts',(0.426170633355844,5.12393688968866,12.8631745524838));
#10612=CARTESIAN_POINT('Ctrl Pts',(0.894375700366544,5.06436719888638,12.8376028269245));
#10613=CARTESIAN_POINT('Ctrl Pts',(1.1378409355763,5.01528105320431,12.8243159654074));
#10614=CARTESIAN_POINT('Ctrl Pts',(1.54133081496255,4.90302585910194,12.8018610211369));
#10615=CARTESIAN_POINT('Ctrl Pts',(1.70346547231188,4.84907893628779,12.792708243885));
#10616=CARTESIAN_POINT('Ctrl Pts',(2.03990341334884,4.71817620875839,12.773131893461));
#10617=CARTESIAN_POINT('Ctrl Pts',(2.21322660189523,4.63939850648156,12.7626962755128));
#10618=CARTESIAN_POINT('Ctrl Pts',(2.57759304934542,4.4487144054424,12.7401458882247));
#10619=CARTESIAN_POINT('Ctrl Pts',(2.76659457459465,4.33370552808602,12.7280595992305));
#10620=CARTESIAN_POINT('Ctrl Pts',(3.21258915589885,4.02121390944499,12.6985047889758));
#10621=CARTESIAN_POINT('Ctrl Pts',(3.45944206411802,3.8109257157081,12.6812347620744));
#10622=CARTESIAN_POINT('Ctrl Pts',(3.77618668904046,3.48479454645855,12.65683021443));
#10623=CARTESIAN_POINT('Ctrl Pts',(3.86386780007027,3.38731512600791,12.6497794423507));
#10624=CARTESIAN_POINT('Ctrl Pts',(4.06474417199863,3.14603018619013,12.6327292376255));
#10625=CARTESIAN_POINT('Ctrl Pts',(4.17417195529512,2.99932292928893,12.622695197408));
#10626=CARTESIAN_POINT('Ctrl Pts',(4.39679822601708,2.66500050505871,12.600670836019));
#10627=CARTESIAN_POINT('Ctrl Pts',(4.50630075151071,2.47534223162136,12.5887092463883));
#10628=CARTESIAN_POINT('Ctrl Pts',(4.74450149151707,1.99425659393549,12.5595784550069));
#10629=CARTESIAN_POINT('Ctrl Pts',(4.85884977599643,1.696742899886,12.5425975696677));
#10630=CARTESIAN_POINT('Ctrl Pts',(4.98119209192641,1.26168531451468,12.5183413937063));
#10631=CARTESIAN_POINT('Ctrl Pts',(5.01238159027475,1.1314390876598,12.5111414052029));
#10632=CARTESIAN_POINT('Ctrl Pts',(5.07492676279779,0.816347627802187,12.4936978806807));
#10633=CARTESIAN_POINT('Ctrl Pts',(5.10132354831581,0.630715080651572,12.483417067094));
#10634=CARTESIAN_POINT('Ctrl Pts',(5.13619445156669,0.228848147858504,12.4612994593529));
#10635=CARTESIAN_POINT('Ctrl Pts',(5.14127489907074,0.0126700805803074,
12.449490302741));
#10636=CARTESIAN_POINT('Ctrl Pts',(5.12024888680174,-0.518468830665231,
12.4206471108741));
#10637=CARTESIAN_POINT('Ctrl Pts',(5.07874522800982,-0.831931102533435,
12.4037983456324));
#10638=CARTESIAN_POINT('Ctrl Pts',(4.97874548083299,-1.27144673564097,12.3796072818303));
#10639=CARTESIAN_POINT('Ctrl Pts',(4.94355449794596,-1.40205256011753,12.3723365704161));
#10640=CARTESIAN_POINT('Ctrl Pts',(4.84680110178377,-1.71189584239804,12.354711560401));
#10641=CARTESIAN_POINT('Ctrl Pts',(4.78039617850477,-1.88941234290117,12.3443188062455));
#10642=CARTESIAN_POINT('Ctrl Pts',(4.61609835217616,-2.26409390721354,12.3218866113472));
#10643=CARTESIAN_POINT('Ctrl Pts',(4.51503098505734,-2.45946820235544,12.3098767248542));
#10644=CARTESIAN_POINT('Ctrl Pts',(4.24939101342763,-2.90107875766833,12.2819232038512));
#10645=CARTESIAN_POINT('Ctrl Pts',(4.07543835190121,-3.14076233381926,12.2661211137436));
#10646=CARTESIAN_POINT('Ctrl Pts',(3.78561896444567,-3.47517974901731,12.2423821719534));
#10647=CARTESIAN_POINT('Ctrl Pts',(3.68468308490064,-3.58202380726063,12.2344908577794));
#10648=CARTESIAN_POINT('Ctrl Pts',(3.43154529156971,-3.82794166823245,12.2153349307228));
#10649=CARTESIAN_POINT('Ctrl Pts',(3.27528254605842,-3.96246928792975,12.2040228135355));
#10650=CARTESIAN_POINT('Ctrl Pts',(2.93407652322816,-4.22220814896818,12.1805151065899));
#10651=CARTESIAN_POINT('Ctrl Pts',(2.74818948803948,-4.34549249156184,12.16834989307));
#10652=CARTESIAN_POINT('Ctrl Pts',(2.34821702770868,-4.57480346760217,12.1433710880637));
#10653=CARTESIAN_POINT('Ctrl Pts',(2.13355075891114,-4.67877349436502,12.1306018926181));
#10654=CARTESIAN_POINT('Ctrl Pts',(1.74199567743333,-4.83584349816913,12.1079834482912));
#10655=CARTESIAN_POINT('Ctrl Pts',(1.56801725073646,-4.89502230494025,12.098147981642));
#10656=CARTESIAN_POINT('Ctrl Pts',(1.22081083018172,-4.99271168462182,12.0785802687795));
#10657=CARTESIAN_POINT('Ctrl Pts',(1.04801034427448,-5.03182091013587,12.0688728460095));
#10658=CARTESIAN_POINT('Ctrl Pts',(0.75894002071506,-5.08170587791294,12.0527870960109));
#10659=CARTESIAN_POINT('Ctrl Pts',(0.64370193501755,-5.09758498577776,12.0464129556961));
#10660=CARTESIAN_POINT('Ctrl Pts',(0.447458996757989,-5.11786489007452,
12.0356294002439));
#10661=CARTESIAN_POINT('Ctrl Pts',(0.366707872342953,-5.12428396099191,
12.031212166141));
#10662=CARTESIAN_POINT('Ctrl Pts',(0.1138367927602,-5.13837699370879,12.0174358132956));
#10663=CARTESIAN_POINT('Ctrl Pts',(-0.0585403322878479,-5.13930460856412,
12.0081294257262));
#10664=CARTESIAN_POINT('Ctrl Pts',(-0.534759809341479,-5.11790073709783,
11.9824861011697));
#10665=CARTESIAN_POINT('Ctrl Pts',(-0.837055304337044,-5.07722433240468,
11.9663083528191));
#10666=CARTESIAN_POINT('Ctrl Pts',(-1.32000612392216,-4.96791415071457,
11.9394573374936));
#10667=CARTESIAN_POINT('Ctrl Pts',(-1.50356008218921,-4.91547475334482,
11.9289935131619));
#10668=CARTESIAN_POINT('Ctrl Pts',(-1.89279561245778,-4.78042648073306,
11.906401947339));
#10669=CARTESIAN_POINT('Ctrl Pts',(-2.09692245108785,-4.69447251309896,
11.8943028392958));
#10670=CARTESIAN_POINT('Ctrl Pts',(-2.59734217930105,-4.44458269703522,
11.8639478713378));
#10671=CARTESIAN_POINT('Ctrl Pts',(-2.88416196309347,-4.26404908910189,
11.8459240815326));
#10672=CARTESIAN_POINT('Ctrl Pts',(-3.24638423165515,-3.98267858431652,
11.8212860429036));
#10673=CARTESIAN_POINT('Ctrl Pts',(-3.33897108149012,-3.90538229021187,
11.8147912500703));
#10674=CARTESIAN_POINT('Ctrl Pts',(-3.58248587675597,-3.68708847015701,
11.7970207386546));
#10675=CARTESIAN_POINT('Ctrl Pts',(-3.72776945354604,-3.54013555732661,
11.7856806415028));
#10676=CARTESIAN_POINT('Ctrl Pts',(-4.00583540217605,-3.22272186408579,
11.7625517642465));
#10677=CARTESIAN_POINT('Ctrl Pts',(-4.13751607794587,-3.05182202124432,
11.7507893483979));
#10678=CARTESIAN_POINT('Ctrl Pts',(-4.40844481800982,-2.65030002825791,
11.7245500082159));
#10679=CARTESIAN_POINT('Ctrl Pts',(-4.54109025864236,-2.41598390962851,
11.7101701848864));
#10680=CARTESIAN_POINT('Ctrl Pts',(-4.71976620185243,-2.03312951712328,
11.6875101452456));
#10681=CARTESIAN_POINT('Ctrl Pts',(-4.7784646404832,-1.89105337558102,11.679261924774));
#10682=CARTESIAN_POINT('Ctrl Pts',(-4.88758287393664,-1.58925028925234,
11.6618454136832));
#10683=CARTESIAN_POINT('Ctrl Pts',(-4.93674089618645,-1.42925528175306,
11.6526772545995));
#10684=CARTESIAN_POINT('Ctrl Pts',(-5.02105464071223,-1.09802838236001,
11.633935117075));
#10685=CARTESIAN_POINT('Ctrl Pts',(-5.05545848627692,-0.92682079579276,
11.6243733966469));
#10686=CARTESIAN_POINT('Ctrl Pts',(-5.09239223521895,-0.677994207856829,
11.6106635818307));
#10687=CARTESIAN_POINT('Ctrl Pts',(-5.10198717475003,-0.601549559696101,
11.606475931118));
#10688=CARTESIAN_POINT('Ctrl Pts',(-5.1277785174244,-0.350481287022635,
11.5927912891983));
#10689=CARTESIAN_POINT('Ctrl Pts',(-5.13675406642089,-0.175239897197318,
11.5833522487284));
#10690=CARTESIAN_POINT('Ctrl Pts',(-5.13674532147658,0.201746395123558,
11.5631162684455));
#10691=CARTESIAN_POINT('Ctrl Pts',(-5.12486929042445,0.403196514690206,
11.5523466561477));
#10692=CARTESIAN_POINT('Ctrl Pts',(-5.08956653666402,0.701636399335537,
11.5361450535164));
#10693=CARTESIAN_POINT('Ctrl Pts',(-5.07511543220857,0.799489803161525,
11.5307860856218));
#10694=CARTESIAN_POINT('Ctrl Pts',(-5.01650915027294,1.12999859525954,11.512486978629));
#10695=CARTESIAN_POINT('Ctrl Pts',(-4.9591002514135,1.35999468364453,11.4994660930734));
#10696=CARTESIAN_POINT('Ctrl Pts',(-4.83030861967047,1.75696454065474,11.4766397854257));
#10697=CARTESIAN_POINT('Ctrl Pts',(-4.76556619713695,1.92566529187235,11.4668168454676));
#10698=CARTESIAN_POINT('Ctrl Pts',(-4.66008657145207,2.1623993146635,11.452801983407));
#10699=CARTESIAN_POINT('Ctrl Pts',(-4.62645574087763,2.23344690984212,11.4485639156551));
#10700=CARTESIAN_POINT('Ctrl Pts',(-4.50159121627279,2.48229881749279,11.4335806477222));
#10701=CARTESIAN_POINT('Ctrl Pts',(-4.40163066974278,2.65551804842615,11.4229009965103));
#10702=CARTESIAN_POINT('Ctrl Pts',(-4.29183622844418,2.82247096543331,11.4121712634621));
#10703=CARTESIAN_POINT('Origin',(0.,0.,0.));
#10704=CARTESIAN_POINT('',(-4.29147790789384,2.82223516558083,9.66201704729454));
#10705=CARTESIAN_POINT('',(-4.29183622628417,2.82247096871782,10.1386883748835));
#10706=CARTESIAN_POINT('',(-4.29183622825304,2.82247096572397,0.));
#10707=CARTESIAN_POINT('',(-5.13684723413363,0.000128082860076971,10.3009584946969));
#10708=CARTESIAN_POINT('Ctrl Pts',(-4.29183622628417,2.82247096871782,10.1386883748835));
#10709=CARTESIAN_POINT('Ctrl Pts',(-4.34083109202366,2.74796960377439,10.1435395218449));
#10710=CARTESIAN_POINT('Ctrl Pts',(-4.38788013653966,2.672201517456,10.1484139523655));
#10711=CARTESIAN_POINT('Ctrl Pts',(-4.56670902924153,2.36674391274659,10.1677992315681));
#10712=CARTESIAN_POINT('Ctrl Pts',(-4.68261820116927,2.12823849428426,10.1823314494109));
#10713=CARTESIAN_POINT('Ctrl Pts',(-4.83954528871763,1.72966906163324,10.2056276174853));
#10714=CARTESIAN_POINT('Ctrl Pts',(-4.892164775472,1.57469968683397,10.2144657681278));
#10715=CARTESIAN_POINT('Ctrl Pts',(-5.02439454951934,1.11412362911239,10.2402507046387));
#10716=CARTESIAN_POINT('Ctrl Pts',(-5.08334220896111,0.803390581211435,
10.257011770707));
#10717=CARTESIAN_POINT('Ctrl Pts',(-5.12895407492712,0.326652854974812,
10.2829990761926));
#10718=CARTESIAN_POINT('Ctrl Pts',(-5.13674602407281,0.163434288575042,
10.2919476345316));
#10719=CARTESIAN_POINT('Ctrl Pts',(-5.13674999847882,0.00012501145318828,
10.3009025249688));
#10720=CARTESIAN_POINT('Ctrl Pts',(-5.13684723413363,0.000128082860076971,
10.3009584946969));
#10721=CARTESIAN_POINT('Ctrl Pts',(-5.13614064254843,-0.687574204925511,
10.3382493678326));
#10722=CARTESIAN_POINT('Ctrl Pts',(-4.82448783135896,-2.23001569616463,
10.4218550665042));
#10723=CARTESIAN_POINT('Ctrl Pts',(-3.32632042058165,-4.19626932876706,
10.5517755907113));
#10724=CARTESIAN_POINT('Ctrl Pts',(-0.913310824303407,-5.27626261269656,
10.6907200673184));
#10725=CARTESIAN_POINT('Ctrl Pts',(1.72231626671068,-5.07017854689106,10.8296645439257));
#10726=CARTESIAN_POINT('Ctrl Pts',(3.93813257454472,-3.6282496668833,10.9686090205328));
#10727=CARTESIAN_POINT('Ctrl Pts',(5.19403777177804,-1.3019429500838,11.10755349714));
#10728=CARTESIAN_POINT('Ctrl Pts',(5.18390774250871,1.34170948311754,11.2464979737472));
#10729=CARTESIAN_POINT('Ctrl Pts',(3.91021165898081,3.65832319538621,11.3854424503544));
#10730=CARTESIAN_POINT('Ctrl Pts',(1.68341012630706,5.08322871476155,11.5243869269616));
#10731=CARTESIAN_POINT('Ctrl Pts',(-0.953718903816859,5.26910847036118,
11.6633314035688));
#10732=CARTESIAN_POINT('Ctrl Pts',(-3.05672897793555,4.30844986953081,11.7848460343876));
#10733=CARTESIAN_POINT('Ctrl Pts',(-3.99850791102981,3.26727227258147,11.8600458396708));
#10734=CARTESIAN_POINT('Ctrl Pts',(-4.29155726418515,2.82228712074135,11.8889308194183));
#10735=CARTESIAN_POINT('',(-5.13658335629485,-0.000126015287452153,9.82404150530312));
#10736=CARTESIAN_POINT('Ctrl Pts',(-4.29183622844418,2.82247096543331,11.4121712634621));
#10737=CARTESIAN_POINT('Ctrl Pts',(-4.28994791435063,2.82534232706525,11.4119867267416));
#10738=CARTESIAN_POINT('Ctrl Pts',(-4.28805669151549,2.82821183506285,11.4118021730424));
#10739=CARTESIAN_POINT('Ctrl Pts',(-4.2474485640806,2.8896912235692,11.4078451540581));
#10740=CARTESIAN_POINT('Ctrl Pts',(-4.20753668038186,2.94750226562249,11.4040669279646));
#10741=CARTESIAN_POINT('Ctrl Pts',(-4.10824353578134,3.08519686448068,11.3949026479613));
#10742=CARTESIAN_POINT('Ctrl Pts',(-4.04770306037154,3.16420666041538,11.3894981061057));
#10743=CARTESIAN_POINT('Ctrl Pts',(-3.9029307218828,3.34218623597612,11.3769747001215));
#10744=CARTESIAN_POINT('Ctrl Pts',(-3.8171617097086,3.43981876560561,11.3698496147885));
#10745=CARTESIAN_POINT('Ctrl Pts',(-3.56864371293256,3.7019571099109,11.3500426044299));
#10746=CARTESIAN_POINT('Ctrl Pts',(-3.39834304240547,3.85888233888637,11.3373971069978));
#10747=CARTESIAN_POINT('Ctrl Pts',(-3.04479348620101,4.14304715807517,11.3127984920234));
#10748=CARTESIAN_POINT('Ctrl Pts',(-2.8626847733648,4.27090691818338,11.3008621114949));
#10749=CARTESIAN_POINT('Ctrl Pts',(-2.49628564729489,4.49416459800045,11.2778550967654));
#10750=CARTESIAN_POINT('Ctrl Pts',(-2.31337396437934,4.59099719008163,11.2668007368887));
#10751=CARTESIAN_POINT('Ctrl Pts',(-1.99090324041689,4.73753541914524,11.2476015538077));
#10752=CARTESIAN_POINT('Ctrl Pts',(-1.85411610055745,4.79272254575252,11.2395343469497));
#10753=CARTESIAN_POINT('Ctrl Pts',(-1.43727006089289,4.94038058340897,11.2152934471992));
#10754=CARTESIAN_POINT('Ctrl Pts',(-1.15142682466936,5.01471131485522,11.1991520408148));
#10755=CARTESIAN_POINT('Ctrl Pts',(-0.64452096905599,5.10087395656544,11.171300297607));
#10756=CARTESIAN_POINT('Ctrl Pts',(-0.426121213311639,5.12374332014506,
11.1595314524612));
#10757=CARTESIAN_POINT('Ctrl Pts',(-0.0169939703559984,5.14023781924363,
11.1375784423278));
#10758=CARTESIAN_POINT('Ctrl Pts',(0.173214079208224,5.1373463946278,11.1274065948019));
#10759=CARTESIAN_POINT('Ctrl Pts',(0.498162248590264,5.11433714102349,11.1097555289829));
#10760=CARTESIAN_POINT('Ctrl Pts',(0.633069238389082,5.0993952412627,11.102338301211));
#10761=CARTESIAN_POINT('Ctrl Pts',(1.0783485223739,5.03213401156622,11.0776624747847));
#10762=CARTESIAN_POINT('Ctrl Pts',(1.38450712203306,4.95664781813367,11.0604240957339));
#10763=CARTESIAN_POINT('Ctrl Pts',(1.90152583266395,4.77749519085442,11.0307954595874));
#10764=CARTESIAN_POINT('Ctrl Pts',(2.11579872560115,4.686540208976,11.018335390638));
#10765=CARTESIAN_POINT('Ctrl Pts',(2.48246751895757,4.50060603847139,10.9962940172645));
#10766=CARTESIAN_POINT('Ctrl Pts',(2.63743670803161,4.41157850905834,10.9867261142502));
#10767=CARTESIAN_POINT('Ctrl Pts',(3.05750386593181,4.14019777102209,10.9596040627519));
#10768=CARTESIAN_POINT('Ctrl Pts',(3.31058060893463,3.94076439789699,10.9418788746898));
#10769=CARTESIAN_POINT('Ctrl Pts',(3.66590715162429,3.60221876841865,10.9150897212574));
#10770=CARTESIAN_POINT('Ctrl Pts',(3.782618036974,3.47946231159423,10.9059042506902));
#10771=CARTESIAN_POINT('Ctrl Pts',(4.11356483860027,3.09500071104522,10.8785226599394));
#10772=CARTESIAN_POINT('Ctrl Pts',(4.3082478311266,2.8177011514594,10.8605818924567));
#10773=CARTESIAN_POINT('Ctrl Pts',(4.5260579832811,2.43148329251716,10.8366112656184));
#10774=CARTESIAN_POINT('Ctrl Pts',(4.57499822588214,2.33809795426995,10.8308730381771));
#10775=CARTESIAN_POINT('Ctrl Pts',(4.69208663977523,2.09690194140828,10.8162166512067));
#10776=CARTESIAN_POINT('Ctrl Pts',(4.75614850802074,1.94723547338733,10.8072825660391));
#10777=CARTESIAN_POINT('Ctrl Pts',(4.87725248574582,1.62247550730087,10.7882956303873));
#10778=CARTESIAN_POINT('Ctrl Pts',(4.93220779666497,1.44684035708545,10.7782636247326));
#10779=CARTESIAN_POINT('Ctrl Pts',(5.03496889322559,1.04364591474228,10.7557066859083));
#10780=CARTESIAN_POINT('Ctrl Pts',(5.07699163525871,0.815026068638081,10.7432498333393));
#10781=CARTESIAN_POINT('Ctrl Pts',(5.12490878482816,0.396540013934391,10.7206663874709));
#10782=CARTESIAN_POINT('Ctrl Pts',(5.13602910212463,0.207693518775206,10.7105503519872));
#10783=CARTESIAN_POINT('Ctrl Pts',(5.13720662253577,-0.116308156197909,
10.6929950160979));
#10784=CARTESIAN_POINT('Ctrl Pts',(5.13237683428155,-0.251248834867124,
10.6856167286514));
#10785=CARTESIAN_POINT('Ctrl Pts',(5.09850530505004,-0.700912836497425,
10.6609083338576));
#10786=CARTESIAN_POINT('Ctrl Pts',(5.04575103091411,-1.01313430145774,10.6435975141725));
#10787=CARTESIAN_POINT('Ctrl Pts',(4.90513714330223,-1.54258652848114,10.6139356606848));
#10788=CARTESIAN_POINT('Ctrl Pts',(4.83053091859768,-1.7623612582539,10.6015120011097));
#10789=CARTESIAN_POINT('Ctrl Pts',(4.67246591390906,-2.14156558158247,10.5794861141244));
#10790=CARTESIAN_POINT('Ctrl Pts',(4.59500939537069,-2.30306906815642,10.5698972670432));
#10791=CARTESIAN_POINT('Ctrl Pts',(4.42726639454091,-2.61052450520569,10.5509026113368));
#10792=CARTESIAN_POINT('Ctrl Pts',(4.33778470847257,-2.75665521805149,10.5415176360143));
#10793=CARTESIAN_POINT('Ctrl Pts',(4.09994198056717,-3.10472908850223,10.5184005935865));
#10794=CARTESIAN_POINT('Ctrl Pts',(3.94378684083705,-3.30082067618229,10.5047047641667));
#10795=CARTESIAN_POINT('Ctrl Pts',(3.62214065505836,-3.64916123866251,10.4789931638158));
#10796=CARTESIAN_POINT('Ctrl Pts',(3.45974175700126,-3.80348137401556,10.4669770503808));
#10797=CARTESIAN_POINT('Ctrl Pts',(3.1305729833851,-4.07769373658459,10.4440048452982));
#10798=CARTESIAN_POINT('Ctrl Pts',(2.96566780625345,-4.19915286595873,10.4330639655872));
#10799=CARTESIAN_POINT('Ctrl Pts',(2.67148765708166,-4.3898355796708,10.4140623026202));
#10800=CARTESIAN_POINT('Ctrl Pts',(2.54568756441235,-4.46396414770112,10.4060770551772));
#10801=CARTESIAN_POINT('Ctrl Pts',(2.15473449075717,-4.67242933519697,10.3817913667956));
#10802=CARTESIAN_POINT('Ctrl Pts',(1.88092231938915,-4.78921870273098,10.3655220146556));
#10803=CARTESIAN_POINT('Ctrl Pts',(1.38903662920752,-4.95029095580603,10.3374866115439));
#10804=CARTESIAN_POINT('Ctrl Pts',(1.17532187686411,-5.00533957868389,10.3256602702292));
#10805=CARTESIAN_POINT('Ctrl Pts',(0.773999581664107,-5.08158264302437,
10.303758895609));
#10806=CARTESIAN_POINT('Ctrl Pts',(0.587484770776609,-5.10650728876771,
10.2936957441874));
#10807=CARTESIAN_POINT('Ctrl Pts',(0.26611697357661,-5.13161026139412,10.276230647042));
#10808=CARTESIAN_POINT('Ctrl Pts',(0.131850023161423,-5.13681381527077,
10.2688887876281));
#10809=CARTESIAN_POINT('Ctrl Pts',(-0.319670293464739,-5.13659730232582,
10.24414915484));
#10810=CARTESIAN_POINT('Ctrl Pts',(-0.636191331126812,-5.10706286114678,
10.226769772693));
#10811=CARTESIAN_POINT('Ctrl Pts',(-1.16368883788394,-5.00801422346111,
10.1977091727481));
#10812=CARTESIAN_POINT('Ctrl Pts',(-1.37659671361609,-4.95372203897602,
10.1859381440721));
#10813=CARTESIAN_POINT('Ctrl Pts',(-1.75878345598588,-4.82971176552803,
10.1643962789253));
#10814=CARTESIAN_POINT('Ctrl Pts',(-1.92906550853401,-4.76425639343368,
10.1546368134859));
#10815=CARTESIAN_POINT('Ctrl Pts',(-2.21484103151283,-4.63656815932604,
10.1376804923676));
#10816=CARTESIAN_POINT('Ctrl Pts',(-2.3320969802161,-4.57871240481641,10.1305383988846));
#10817=CARTESIAN_POINT('Ctrl Pts',(-2.73213353207538,-4.36197227744395,
10.1056133316696));
#10818=CARTESIAN_POINT('Ctrl Pts',(-3.00199190604444,-4.18083849722328,
10.0878433831701));
#10819=CARTESIAN_POINT('Ctrl Pts',(-3.42441108922433,-3.8351897508475,10.0582948030191));
#10820=CARTESIAN_POINT('Ctrl Pts',(-3.5865992131806,-3.68396256473145,10.0464181690309));
#10821=CARTESIAN_POINT('Ctrl Pts',(-3.86831467972195,-3.38499081771354,
10.0243946730317));
#10822=CARTESIAN_POINT('Ctrl Pts',(-3.99039562212548,-3.24017923506791,
10.0142615884703));
#10823=CARTESIAN_POINT('Ctrl Pts',(-4.15204132140484,-3.02540601636154,
9.99967824203985));
#10824=CARTESIAN_POINT('Ctrl Pts',(-4.19839473964942,-2.96074484281005,
9.99534049302957));
#10825=CARTESIAN_POINT('Ctrl Pts',(-4.33817387080808,-2.7558717423584,9.98178039695737));
#10826=CARTESIAN_POINT('Ctrl Pts',(-4.42621679630225,-2.61212296408422,
9.97252916752709));
#10827=CARTESIAN_POINT('Ctrl Pts',(-4.60079611551422,-2.2928304044208,9.95260019882058));
#10828=CARTESIAN_POINT('Ctrl Pts',(-4.68469406441972,-2.11613808559128,
9.94194944602537));
#10829=CARTESIAN_POINT('Ctrl Pts',(-4.8157527953289,-1.79386956005154,9.92311509375324));
#10830=CARTESIAN_POINT('Ctrl Pts',(-4.86686984338799,-1.65015817626784,
9.91491157199256));
#10831=CARTESIAN_POINT('Ctrl Pts',(-4.98332760266446,-1.26994653246926,
9.89356600498713));
#10832=CARTESIAN_POINT('Ctrl Pts',(-5.03825652933309,-1.03067216725358,
9.88049178783821));
#10833=CARTESIAN_POINT('Ctrl Pts',(-5.08249254213491,-0.745870143370513,
9.86488239127982));
#10834=CARTESIAN_POINT('Ctrl Pts',(-5.08856307846514,-0.703262702007987,
9.86254492289813));
#10835=CARTESIAN_POINT('Ctrl Pts',(-5.12249743520096,-0.44157785562199,
9.84817827333096));
#10836=CARTESIAN_POINT('Ctrl Pts',(-5.13674435468852,-0.220969231918046,
9.8360385854582));
#10837=CARTESIAN_POINT('Ctrl Pts',(-5.13674999832263,-0.000131272438793767,
9.82394557894206));
#10838=CARTESIAN_POINT('Ctrl Pts',(-5.13658335629485,-0.000126015287452153,
9.82404150530312));
#10839=CARTESIAN_POINT('Ctrl Pts',(-5.13603076124125,0.601945860711958,
9.79139879103644));
#10840=CARTESIAN_POINT('Ctrl Pts',(-4.96092370381945,1.59840118087525,9.73739063836703));
#10841=CARTESIAN_POINT('Ctrl Pts',(-4.50810837244381,2.49298111405563,9.68338248569762));
#10842=CARTESIAN_POINT('Ctrl Pts',(-4.29147790789737,2.82223516557546,9.66201704729489));
#10843=CARTESIAN_POINT('Origin',(0.,0.,0.));
#10844=CARTESIAN_POINT('',(-4.29183622825303,2.82247096572398,7.9120163777544));
#10845=CARTESIAN_POINT('',(-4.2918361854396,2.82247103082588,8.38917442239304));
#10846=CARTESIAN_POINT('',(-4.29183622825304,2.82247096572397,0.));
#10847=CARTESIAN_POINT('Ctrl Pts',(-4.2918361854396,2.82247103082587,8.38917442239304));
#10848=CARTESIAN_POINT('Ctrl Pts',(-4.32942666324407,2.7653111269306,8.39289704544047));
#10849=CARTESIAN_POINT('Ctrl Pts',(-4.36587935814393,2.70739398876421,8.3966115467939));
#10850=CARTESIAN_POINT('Ctrl Pts',(-4.53974565731834,2.41849759257399,8.41487322461712));
#10851=CARTESIAN_POINT('Ctrl Pts',(-4.66003820603287,2.17772084036754,8.42924495813878));
#10852=CARTESIAN_POINT('Ctrl Pts',(-4.81768645716247,1.78855813720054,8.45176628056113));
#10853=CARTESIAN_POINT('Ctrl Pts',(-4.86822148280676,1.64604411757638,8.45988135237389));
#10854=CARTESIAN_POINT('Ctrl Pts',(-4.96087873692471,1.34290348903069,8.47708499786189));
#10855=CARTESIAN_POINT('Ctrl Pts',(-5.001648045299,1.18204187236612,8.48617450672251));
#10856=CARTESIAN_POINT('Ctrl Pts',(-5.0692829089734,0.848040512523393,8.50486124080666));
#10857=CARTESIAN_POINT('Ctrl Pts',(-5.09522129246755,0.674924561328445,
8.51444624124013));
#10858=CARTESIAN_POINT('Ctrl Pts',(-5.1285844725791,0.334360770111465,8.53309680238365));
#10859=CARTESIAN_POINT('Ctrl Pts',(-5.13675206408452,0.167200064917802,
8.54215599106349));
#10860=CARTESIAN_POINT('Ctrl Pts',(-5.13674781081197,-0.177400897830959,
8.56072997932663));
#10861=CARTESIAN_POINT('Ctrl Pts',(-5.12756223984905,-0.354620084305676,
8.57022652294575));
#10862=CARTESIAN_POINT('Ctrl Pts',(-5.09291255051512,-0.688009915850673,
8.58819917488626));
#10863=CARTESIAN_POINT('Ctrl Pts',(-5.06936758864144,-0.844172066190319,
8.5966641612302));
#10864=CARTESIAN_POINT('Ctrl Pts',(-5.01134173026516,-1.13683823145349,
8.61283338519319));
#10865=CARTESIAN_POINT('Ctrl Pts',(-4.97836871468566,-1.27349537275126,
8.62051834504953));
#10866=CARTESIAN_POINT('Ctrl Pts',(-4.85591195726063,-1.70293260456988,
8.64499165791791));
#10867=CARTESIAN_POINT('Ctrl Pts',(-4.74585227860605,-1.98915940995312,
8.6617540699206));
#10868=CARTESIAN_POINT('Ctrl Pts',(-4.51168988908008,-2.46608947792636,
8.69052851677994));
#10869=CARTESIAN_POINT('Ctrl Pts',(-4.39921808421094,-2.66154574572552,
8.70260723033787));
#10870=CARTESIAN_POINT('Ctrl Pts',(-4.16806657052589,-3.00833749445266,
8.72495131001155));
#10871=CARTESIAN_POINT('Ctrl Pts',(-4.05302833689728,-3.16161858676421,
8.73520293859328));
#10872=CARTESIAN_POINT('Ctrl Pts',(-3.90379168677842,-3.33889651685975,
8.74777572921798));
#10873=CARTESIAN_POINT('Ctrl Pts',(-3.87751884141328,-3.36937191105137,
8.74996448116534));
#10874=CARTESIAN_POINT('Ctrl Pts',(-3.69660354323565,-3.57430729532129,
8.764864381742));
#10875=CARTESIAN_POINT('Ctrl Pts',(-3.53059768632202,-3.73837266183361,
8.77768418346644));
#10876=CARTESIAN_POINT('Ctrl Pts',(-3.21544982334438,-4.01005700651953,
8.80044795031635));
#10877=CARTESIAN_POINT('Ctrl Pts',(-3.07058983767729,-4.1220328871384,8.81040426448793));
#10878=CARTESIAN_POINT('Ctrl Pts',(-2.85568071382351,-4.27052832946172,
8.82453325447938));
#10879=CARTESIAN_POINT('Ctrl Pts',(-2.79029039042693,-4.31353732575679,
8.82875402004098));
#10880=CARTESIAN_POINT('Ctrl Pts',(-2.55512989400085,-4.46062306936487,
8.84368368490406));
#10881=CARTESIAN_POINT('Ctrl Pts',(-2.38032081507339,-4.55630552231217,
8.85432681695324));
#10882=CARTESIAN_POINT('Ctrl Pts',(-2.12261798781973,-4.67847229921776,
8.86963794109643));
#10883=CARTESIAN_POINT('Ctrl Pts',(-2.04392250491921,-4.71338420801666,
8.87426664389985));
#10884=CARTESIAN_POINT('Ctrl Pts',(-1.86995470124771,-4.78538557809084,
8.88443906677613));
#10885=CARTESIAN_POINT('Ctrl Pts',(-1.77437882957508,-4.82164127052871,
8.8899970342641));
#10886=CARTESIAN_POINT('Ctrl Pts',(-1.5392714222834,-4.90288914249991,8.90358666416002));
#10887=CARTESIAN_POINT('Ctrl Pts',(-1.39877136566293,-4.94480705344718,
8.91163020087048));
#10888=CARTESIAN_POINT('Ctrl Pts',(-1.05825295254069,-5.03072339208759,
8.93088047800941));
#10889=CARTESIAN_POINT('Ctrl Pts',(-0.857015884089,-5.06888585489178,8.94205571851761));
#10890=CARTESIAN_POINT('Ctrl Pts',(-0.430356935771449,-5.12365597973203,
8.96538236898676));
#10891=CARTESIAN_POINT('Ctrl Pts',(-0.205026528604712,-5.1376088565812,
8.9774898008687));
#10892=CARTESIAN_POINT('Ctrl Pts',(0.222658495080942,-5.13590256001789,
9.00042215367395));
#10893=CARTESIAN_POINT('Ctrl Pts',(0.424595931256993,-5.12316183784548,
9.01123296641682));
#10894=CARTESIAN_POINT('Ctrl Pts',(0.768382873847419,-5.08100215192302,
9.0300054891934));
#10895=CARTESIAN_POINT('Ctrl Pts',(0.910708465476806,-5.05743053196932,
9.03789399559456));
#10896=CARTESIAN_POINT('Ctrl Pts',(1.3454060112074,-4.9664906699621,9.06223595442882));
#10897=CARTESIAN_POINT('Ctrl Pts',(1.63302740111484,-4.87948527626849,9.07865984223037));
#10898=CARTESIAN_POINT('Ctrl Pts',(2.11734392780056,-4.68532579871062,9.10692137379542));
#10899=CARTESIAN_POINT('Ctrl Pts',(2.31771092573,-4.58951432417861,9.11882139747107));
#10900=CARTESIAN_POINT('Ctrl Pts',(2.67299298145714,-4.39040808357771,9.1406565700454));
#10901=CARTESIAN_POINT('Ctrl Pts',(2.82970033856075,-4.29108007870171,9.15058029104005));
#10902=CARTESIAN_POINT('Ctrl Pts',(3.08870354238832,-4.10654355515846,9.16780972892288));
#10903=CARTESIAN_POINT('Ctrl Pts',(3.19369232684526,-4.02543381076006,9.17505780346289));
#10904=CARTESIAN_POINT('Ctrl Pts',(3.54125067764628,-3.73476160166513,9.19988140672701));
#10905=CARTESIAN_POINT('Ctrl Pts',(3.76730783603636,-3.50660834278117,9.21744096575631));
#10906=CARTESIAN_POINT('Ctrl Pts',(4.11209520275527,-3.0865181355885,9.24686493306114));
#10907=CARTESIAN_POINT('Ctrl Pts',(4.24218806005543,-2.90512719706977,9.25881979989336));
#10908=CARTESIAN_POINT('Ctrl Pts',(4.45998145893393,-2.55547777415373,9.28090461136454));
#10909=CARTESIAN_POINT('Ctrl Pts',(4.55095273561851,-2.38971292614888,9.29102088209895));
#10910=CARTESIAN_POINT('Ctrl Pts',(4.70763340107648,-2.06265913850851,9.31069510406448));
#10911=CARTESIAN_POINT('Ctrl Pts',(4.77468752598387,-1.90229659749899,9.32021743700051));
#10912=CARTESIAN_POINT('Ctrl Pts',(4.91655960543361,-1.50793391116183,9.34319946234509));
#10913=CARTESIAN_POINT('Ctrl Pts',(4.9829785750852,-1.27135838606004,9.35662279810002));
#10914=CARTESIAN_POINT('Ctrl Pts',(5.07717176535824,-0.811581733700417,
9.38207393788696));
#10915=CARTESIAN_POINT('Ctrl Pts',(5.10772062678173,-0.589517568411141,
9.39409681822295));
#10916=CARTESIAN_POINT('Ctrl Pts',(5.13825617788038,-0.162240924357992,
9.41706605270614));
#10917=CARTESIAN_POINT('Ctrl Pts',(5.14064202539698,0.0423692804226592,
9.42799728093886));
#10918=CARTESIAN_POINT('Ctrl Pts',(5.12382892039803,0.392227266607594,9.44698197646185));
#10919=CARTESIAN_POINT('Ctrl Pts',(5.11063011848982,0.537515763965234,9.45496008194773));
#10920=CARTESIAN_POINT('Ctrl Pts',(5.0517920130541,0.976726816741831,9.47924978230916));
#10921=CARTESIAN_POINT('Ctrl Pts',(4.98680389238003,1.2674354846541,9.49553039678682));
#10922=CARTESIAN_POINT('Ctrl Pts',(4.83044261394475,1.76115612285127,9.52358208494756));
#10923=CARTESIAN_POINT('Ctrl Pts',(4.7503775364277,1.96691700526646,9.53541360440793));
#10924=CARTESIAN_POINT('Ctrl Pts',(4.57809158669411,2.33721314615637,9.5573103080189));
#10925=CARTESIAN_POINT('Ctrl Pts',(4.48956731930333,2.50305227564106,9.56736364606978));
#10926=CARTESIAN_POINT('Ctrl Pts',(4.32257337074313,2.77841121080462,9.58481201868659));
#10927=CARTESIAN_POINT('Ctrl Pts',(4.2485169968991,2.89038253748007,9.59214713848556));
#10928=CARTESIAN_POINT('Ctrl Pts',(3.98481282681463,3.25702842951064,9.616892617349));
#10929=CARTESIAN_POINT('Ctrl Pts',(3.77596713451508,3.49700574906384,9.63428475367893));
#10930=CARTESIAN_POINT('Ctrl Pts',(3.49043469271816,3.76948679348533,9.6556548384305));
#10931=CARTESIAN_POINT('Ctrl Pts',(3.43336716062839,3.8215383215272,9.65982465083243));
#10932=CARTESIAN_POINT('Ctrl Pts',(3.23692358867472,3.99276182997105,9.67386403913218));
#10933=CARTESIAN_POINT('Ctrl Pts',(3.09234774183542,4.1057529714019,9.68367736941564));
#10934=CARTESIAN_POINT('Ctrl Pts',(2.81844129077601,4.29712968250449,9.70159814533755));
#10935=CARTESIAN_POINT('Ctrl Pts',(2.69110238561239,4.37800196239046,9.70969152151099));
#10936=CARTESIAN_POINT('Ctrl Pts',(2.29712595106992,4.60452335805537,9.73434171391499));
#10937=CARTESIAN_POINT('Ctrl Pts',(2.02095459424152,4.73224738755845,9.75107592839753));
#10938=CARTESIAN_POINT('Ctrl Pts',(1.57232861944532,4.89325030892307,9.77711683769016));
#10939=CARTESIAN_POINT('Ctrl Pts',(1.40668495195599,4.94341535015533,9.78651271782279));
#10940=CARTESIAN_POINT('Ctrl Pts',(1.16054607375624,5.00458182317777,9.800214153655));
#10941=CARTESIAN_POINT('Ctrl Pts',(1.08182020652955,5.02218793258555,9.80455916285547));
#10942=CARTESIAN_POINT('Ctrl Pts',(0.890469366146186,5.06027295078329,9.8150497012534));
#10943=CARTESIAN_POINT('Ctrl Pts',(0.777511210125311,5.078855633468,9.82118374686248));
#10944=CARTESIAN_POINT('Ctrl Pts',(0.482940025866521,5.11725698742121,9.83711018054788));
#10945=CARTESIAN_POINT('Ctrl Pts',(0.300726894008224,5.13119001399218,9.84689106824658));
#10946=CARTESIAN_POINT('Ctrl Pts',(-0.0526382873010328,5.13932081579788,
9.86606281062832));
#10947=CARTESIAN_POINT('Ctrl Pts',(-0.223527398324413,5.13472716916811,
9.87542618281519));
#10948=CARTESIAN_POINT('Ctrl Pts',(-0.642936894665256,5.10247347976002,
9.89849249545521));
#10949=CARTESIAN_POINT('Ctrl Pts',(-0.890283390993074,5.06517558887105,
9.91215918905798));
#10950=CARTESIAN_POINT('Ctrl Pts',(-1.35225273499904,4.96061658693881,9.9378450687349));
#10951=CARTESIAN_POINT('Ctrl Pts',(-1.56710881927051,4.89698654769837,9.9498639791003));
#10952=CARTESIAN_POINT('Ctrl Pts',(-1.96905247810535,4.74877613486292,9.97283494715439));
#10953=CARTESIAN_POINT('Ctrl Pts',(-2.15657176427373,4.66660878841429,9.98377182860388));
#10954=CARTESIAN_POINT('Ctrl Pts',(-2.46858797968162,4.50705672920182,10.0027664384314));
#10955=CARTESIAN_POINT('Ctrl Pts',(-2.59559676521082,4.43512827049158,10.0107487027106));
#10956=CARTESIAN_POINT('Ctrl Pts',(-2.97150424125781,4.20055825525717,10.0350360557838));
#10957=CARTESIAN_POINT('Ctrl Pts',(-3.20951645387419,4.02163389510829,10.0513101009946));
#10958=CARTESIAN_POINT('Ctrl Pts',(-3.59483444624534,3.67586540971379,10.0793522664599));
#10959=CARTESIAN_POINT('Ctrl Pts',(-3.74929573901876,3.51818208393124,10.0911807423333));
#10960=CARTESIAN_POINT('Ctrl Pts',(-4.01554928564948,3.20885776302716,10.1130624072754));
#10961=CARTESIAN_POINT('Ctrl Pts',(-4.13006583069576,3.06005849625197,10.1231038241817));
#10962=CARTESIAN_POINT('Ctrl Pts',(-4.25500336145006,2.87789057874498,10.1350716196598));
#10963=CARTESIAN_POINT('Ctrl Pts',(-4.27355524320318,2.85026894655662,10.1368783130702));
#10964=CARTESIAN_POINT('Ctrl Pts',(-4.29183622628417,2.82247096871782,10.1386883748835));
#10965=CARTESIAN_POINT('',(-5.13674999921714,8.96808918659131E-5,8.07404150530312));
#10966=CARTESIAN_POINT('Ctrl Pts',(-4.29147790789737,2.82223516557546,9.66201704729489));
#10967=CARTESIAN_POINT('Ctrl Pts',(-4.03850873296674,3.20671998828925,9.63706766016189));
#10968=CARTESIAN_POINT('Ctrl Pts',(-3.16988399740047,4.20897597709122,9.56580344749316));
#10969=CARTESIAN_POINT('Ctrl Pts',(-1.17621811440022,5.22394435702451,9.44822440928873));
#10970=CARTESIAN_POINT('Ctrl Pts',(1.466419928428,5.15001905738628,9.30927993268152));
#10971=CARTESIAN_POINT('Ctrl Pts',(3.75162135492562,3.82078799558379,9.17033545607434));
#10972=CARTESIAN_POINT('Ctrl Pts',(5.12237336835931,1.56024830493584,9.03139097946715));
#10973=CARTESIAN_POINT('Ctrl Pts',(5.24455819522407,-1.0805984614274,8.89244650285997));
#10974=CARTESIAN_POINT('Ctrl Pts',(4.08839355403644,-3.45805174126212,8.75350202625278));
#10975=CARTESIAN_POINT('Ctrl Pts',(1.93569202061813,-4.99261255248659,8.61455754964559));
#10976=CARTESIAN_POINT('Ctrl Pts',(-0.688830164370685,-5.31023508920132,
8.4756130730384));
#10977=CARTESIAN_POINT('Ctrl Pts',(-3.14545151931376,-4.33349956012211,
8.33666859643121));
#10978=CARTESIAN_POINT('Ctrl Pts',(-4.7735013873256,-2.37491963879568,8.2028114111729));
#10979=CARTESIAN_POINT('Ctrl Pts',(-5.13643863329629,-0.760120718689461,
8.11526905145029));
#10980=CARTESIAN_POINT('Ctrl Pts',(-5.13705846939083,8.94657369160089E-5,
8.07404151726341));
#10981=CARTESIAN_POINT('Ctrl Pts',(-5.13674999921714,8.96808918659132E-5,
8.07404150530312));
#10982=CARTESIAN_POINT('Ctrl Pts',(-5.13674836157881,0.0938904733295929,
8.06895421794103));
#10983=CARTESIAN_POINT('Ctrl Pts',(-5.13417692765489,0.187682302088804,
8.06386693057893));
#10984=CARTESIAN_POINT('Ctrl Pts',(-5.12904010520378,0.28133283084496,8.05877964321683));
#10985=CARTESIAN_POINT('Ctrl Pts',(-5.1208932625175,0.42985969400276,8.05071136166081));
#10986=CARTESIAN_POINT('Ctrl Pts',(-5.10628901009753,0.578059904085605,
8.0426430801048));
#10987=CARTESIAN_POINT('Ctrl Pts',(-5.08527745830825,0.725364552843592,
8.0345747985488));
#10988=CARTESIAN_POINT('Ctrl Pts',(-5.06427014698131,0.872639473201553,
8.02650814529918));
#10989=CARTESIAN_POINT('Ctrl Pts',(-5.03685816275778,1.01901886531461,8.01844149204957));
#10990=CARTESIAN_POINT('Ctrl Pts',(-5.00314326900692,1.16394071682829,8.01037483879997));
#10991=CARTESIAN_POINT('Ctrl Pts',(-4.96942715985699,1.30886779267649,8.00230789475298));
#10992=CARTESIAN_POINT('Ctrl Pts',(-4.9294077578192,1.4523368995334,7.99424095070599));
#10993=CARTESIAN_POINT('Ctrl Pts',(-4.88323769496126,1.59379740776846,7.98617400665901));
#10994=CARTESIAN_POINT('Ctrl Pts',(-4.83707042499281,1.73524935886621,7.97810755059237));
#10995=CARTESIAN_POINT('Ctrl Pts',(-4.7847533420389,1.87469263998323,7.97004109452573));
#10996=CARTESIAN_POINT('Ctrl Pts',(-4.72648858792753,2.01159294855864,7.9619746384591));
#10997=CARTESIAN_POINT('Ctrl Pts',(-4.66820929321946,2.14852742208,7.9539061693215));
#10998=CARTESIAN_POINT('Ctrl Pts',(-4.60397949050707,2.28291734996498,7.94583770018391));
#10999=CARTESIAN_POINT('Ctrl Pts',(-4.53404927007515,2.414248905774,7.93776923104631));
#11000=CARTESIAN_POINT('Ctrl Pts',(-4.48223716636189,2.51155396427908,7.93179120956743));
#11001=CARTESIAN_POINT('Ctrl Pts',(-4.42729682191331,2.60718054062894,7.92581318808856));
#11002=CARTESIAN_POINT('Ctrl Pts',(-4.3693461565897,2.70092849338793,7.91983516660969));
#11003=CARTESIAN_POINT('Ctrl Pts',(-4.3440811633814,2.74180017926973,7.91722890365792));
#11004=CARTESIAN_POINT('Ctrl Pts',(-4.31824113528876,2.78231978684708,7.91462264070616));
#11005=CARTESIAN_POINT('Ctrl Pts',(-4.29183622825303,2.82247096572398,7.9120163777544));
#11006=CARTESIAN_POINT('Origin',(0.,0.,0.));
#11007=CARTESIAN_POINT('',(-4.29183649439966,2.8224705610226,6.16186016520308));
#11008=CARTESIAN_POINT('',(-4.29183621579633,2.82247098466558,6.63882185511496));
#11009=CARTESIAN_POINT('',(-4.29183622825304,2.82247096572397,0.));
#11010=CARTESIAN_POINT('',(-5.13675014872027,-9.28711217083157E-6,6.80070473863792));
#11011=CARTESIAN_POINT('Ctrl Pts',(-4.29183621579632,2.82247098466558,6.63882185511496));
#11012=CARTESIAN_POINT('Ctrl Pts',(-4.36054432246575,2.71799375810604,6.64553053324447));
#11013=CARTESIAN_POINT('Ctrl Pts',(-4.42542236198481,2.61103060857702,6.65224907493801));
#11014=CARTESIAN_POINT('Ctrl Pts',(-4.52854727960716,2.42610201637113,6.66371519269886));
#11015=CARTESIAN_POINT('Ctrl Pts',(-4.56883348544287,2.34935554169067,6.66843578009576));
#11016=CARTESIAN_POINT('Ctrl Pts',(-4.67535713383931,2.13331169675636,6.68159938307984));
#11017=CARTESIAN_POINT('Ctrl Pts',(-4.73729251546422,1.99199459944635,6.69006542486853));
#11018=CARTESIAN_POINT('Ctrl Pts',(-4.86290062692858,1.66624949149274,6.70919725108917));
#11019=CARTESIAN_POINT('Ctrl Pts',(-4.9226188023489,1.48054602995318,6.71983565717192));
#11020=CARTESIAN_POINT('Ctrl Pts',(-5.00997839377238,1.1443576750663,6.73866897165481));
#11021=CARTESIAN_POINT('Ctrl Pts',(-5.04173063842234,0.99518408487013,6.74688367030938));
#11022=CARTESIAN_POINT('Ctrl Pts',(-5.11335581407559,0.565611415626293,
6.77028080514691));
#11023=CARTESIAN_POINT('Ctrl Pts',(-5.13675051331794,0.283040576761006,
6.78534315712252));
#11024=CARTESIAN_POINT('Ctrl Pts',(-5.13674999999155,-9.31577570951679E-6,
6.80070448240941));
#11025=CARTESIAN_POINT('Ctrl Pts',(-5.13674999999158,-9.30106097508931E-6,
6.80070448161083));
#11026=CARTESIAN_POINT('Ctrl Pts',(-5.13674950345215,-0.27423596180585,
6.81558696362695));
#11027=CARTESIAN_POINT('Ctrl Pts',(-5.11478964040234,-0.548021090301936,
6.83068431061558));
#11028=CARTESIAN_POINT('Ctrl Pts',(-5.04678958992111,-0.969196820943226,
6.85402175161803));
#11029=CARTESIAN_POINT('Ctrl Pts',(-5.01581385299244,-1.11849915175892,
6.86232311664869));
#11030=CARTESIAN_POINT('Ctrl Pts',(-4.93217527169861,-1.44733483946227,
6.88071042563993));
#11031=CARTESIAN_POINT('Ctrl Pts',(-4.87625374014481,-1.62581745964357,
6.89075940774323));
#11032=CARTESIAN_POINT('Ctrl Pts',(-4.75471855226032,-1.95048110662605,
6.90935726438368));
#11033=CARTESIAN_POINT('Ctrl Pts',(-4.69175846614595,-2.09740958552241,
6.91790335404333));
#11034=CARTESIAN_POINT('Ctrl Pts',(-4.58659378739211,-2.31429550917129,
6.93087454579517));
#11035=CARTESIAN_POINT('Ctrl Pts',(-4.54940313229822,-2.3865743567122,6.93526035462519));
#11036=CARTESIAN_POINT('Ctrl Pts',(-4.4086137130355,-2.64493403091877,6.9512287255878));
#11037=CARTESIAN_POINT('Ctrl Pts',(-4.29518531803503,-2.82540829394662,
6.96292550732711));
#11038=CARTESIAN_POINT('Ctrl Pts',(-4.07791257783295,-3.12765094233414,
6.98332890063532));
#11039=CARTESIAN_POINT('Ctrl Pts',(-3.97897322645356,-3.25259046098966,
6.9920375634287));
#11040=CARTESIAN_POINT('Ctrl Pts',(-3.76110983985535,-3.50285857226653,
7.01008565733192));
#11041=CARTESIAN_POINT('Ctrl Pts',(-3.64134660308096,-3.62719756988625,
7.01940526766324));
#11042=CARTESIAN_POINT('Ctrl Pts',(-3.29319917853703,-3.95399069951888,
7.04508999435205));
#11043=CARTESIAN_POINT('Ctrl Pts',(-3.05270619465187,-4.14248481942735,
7.0612956912011));
#11044=CARTESIAN_POINT('Ctrl Pts',(-2.66938000634769,-4.3913248169919,7.08608277178135));
#11045=CARTESIAN_POINT('Ctrl Pts',(-2.53822428951772,-4.46841575447014,
7.09440807688176));
#11046=CARTESIAN_POINT('Ctrl Pts',(-2.24217403483129,-4.62518352009839,
7.11277421305259));
#11047=CARTESIAN_POINT('Ctrl Pts',(-2.07604374735069,-4.70209640571389,
7.12280514878522));
#11048=CARTESIAN_POINT('Ctrl Pts',(-1.83446541981166,-4.79863510057314,
7.13699356723012));
#11049=CARTESIAN_POINT('Ctrl Pts',(-1.76212929828872,-4.82566707517999,
7.14119411453483));
#11050=CARTESIAN_POINT('Ctrl Pts',(-1.39095217583523,-4.95491648113349,
7.16252117329537));
#11051=CARTESIAN_POINT('Ctrl Pts',(-1.08374941351432,-5.03104724260106,
7.17938545784351));
#11052=CARTESIAN_POINT('Ctrl Pts',(-0.637978411693939,-5.09876691955784,
7.20358407265057));
#11053=CARTESIAN_POINT('Ctrl Pts',(-0.503709634645125,-5.11377710239055,
7.21084638396267));
#11054=CARTESIAN_POINT('Ctrl Pts',(-0.180344330600151,-5.13706672041347,
7.22845003050856));
#11055=CARTESIAN_POINT('Ctrl Pts',(0.00892203440674387,-5.1402234677049,
7.23882968510254));
#11056=CARTESIAN_POINT('Ctrl Pts',(0.417628408824725,-5.12446359669769,
7.26125584076046));
#11057=CARTESIAN_POINT('Ctrl Pts',(0.636562282602356,-5.10189499334267,
7.27327272826308));
#11058=CARTESIAN_POINT('Ctrl Pts',(1.14514014747377,-5.01621327712766,7.30124785130825));
#11059=CARTESIAN_POINT('Ctrl Pts',(1.4321114669278,-4.94194316041895,7.3170641337704));
#11060=CARTESIAN_POINT('Ctrl Pts',(1.84945646942886,-4.7945015518509,7.34080839480143));
#11061=CARTESIAN_POINT('Ctrl Pts',(1.98565890163175,-4.73971432203543,7.34869052454216));
#11062=CARTESIAN_POINT('Ctrl Pts',(2.30675754579164,-4.59427981672183,7.36782354348952));
#11063=CARTESIAN_POINT('Ctrl Pts',(2.48891569475288,-4.49820343995965,7.37912180059713));
#11064=CARTESIAN_POINT('Ctrl Pts',(2.85545396747633,-4.27578152793372,7.40262550403596));
#11065=CARTESIAN_POINT('Ctrl Pts',(3.03835895787385,-4.14780708862957,7.41480043167686));
#11066=CARTESIAN_POINT('Ctrl Pts',(3.41066832135115,-3.84943105993617,7.44065023755202));
#11067=CARTESIAN_POINT('Ctrl Pts',(3.5969012665231,-3.67601444936041,7.45425755686874));
#11068=CARTESIAN_POINT('Ctrl Pts',(3.88120336409985,-3.36889917276742,7.47669736174359));
#11069=CARTESIAN_POINT('Ctrl Pts',(3.98701407184942,-3.24298289477458,7.48551136401496));
#11070=CARTESIAN_POINT('Ctrl Pts',(4.20211610597592,-2.96053545335588,7.50476328492376));
#11071=CARTESIAN_POINT('Ctrl Pts',(4.30909291233613,-2.80254634427599,7.51522171498177));
#11072=CARTESIAN_POINT('Ctrl Pts',(4.52076144299933,-2.4490646034915,7.53781399444568));
#11073=CARTESIAN_POINT('Ctrl Pts',(4.62209166797824,-2.25199321670785,7.54991916621719));
#11074=CARTESIAN_POINT('Ctrl Pts',(4.83862930088939,-1.75419992452382,7.579379020834));
#11075=CARTESIAN_POINT('Ctrl Pts',(4.93890802903207,-1.44801318948668,7.59654013623497));
#11076=CARTESIAN_POINT('Ctrl Pts',(5.03908604070774,-1.00561689752975,7.62088785368799));
#11077=CARTESIAN_POINT('Ctrl Pts',(5.06328068884328,-0.875694757219264,
7.62799393891609));
#11078=CARTESIAN_POINT('Ctrl Pts',(5.10921062119309,-0.562351432419921,
7.64519180436847));
#11079=CARTESIAN_POINT('Ctrl Pts',(5.12611713371375,-0.37840961972383,7.65531921411957));
#11080=CARTESIAN_POINT('Ctrl Pts',(5.14130917804655,0.0236422561292717,
7.67738033787116));
#11081=CARTESIAN_POINT('Ctrl Pts',(5.13568644781166,0.241551216386984,7.68928568880778));
#11082=CARTESIAN_POINT('Ctrl Pts',(5.08795681011533,0.774211612571511,7.71830557852863));
#11083=CARTESIAN_POINT('Ctrl Pts',(5.03049090999706,1.08667988858655,7.73523311872986));
#11084=CARTESIAN_POINT('Ctrl Pts',(4.9182480240667,1.48542448513362,7.75746574893529));
#11085=CARTESIAN_POINT('Ctrl Pts',(4.88925868754023,1.57822641515211,7.76269079107157));
#11086=CARTESIAN_POINT('Ctrl Pts',(4.82378547465927,1.76865629021999,7.77357480614793));
#11087=CARTESIAN_POINT('Ctrl Pts',(4.78692917595042,1.86610809546057,7.77924340018738));
#11088=CARTESIAN_POINT('Ctrl Pts',(4.62425516613131,2.2596300912493,7.80251582822976));
#11089=CARTESIAN_POINT('Ctrl Pts',(4.47372032211606,2.54469994475272,7.82019763137673));
#11090=CARTESIAN_POINT('Ctrl Pts',(4.19690789804165,2.96747326399253,7.84764644609172));
#11091=CARTESIAN_POINT('Ctrl Pts',(4.08812953926978,3.11562713685656,7.8575471454494));
#11092=CARTESIAN_POINT('Ctrl Pts',(3.82404402320297,3.43759499336962,7.8799145038888));
#11093=CARTESIAN_POINT('Ctrl Pts',(3.66438115743665,3.6073092984431,7.89232976661486));
#11094=CARTESIAN_POINT('Ctrl Pts',(3.46445092934173,3.79280625070061,7.90705158945612));
#11095=CARTESIAN_POINT('Ctrl Pts',(3.43482142564496,3.8196598313788,7.90921427837658));
#11096=CARTESIAN_POINT('Ctrl Pts',(3.26450702536935,3.97043350904541,7.92155006128397));
#11097=CARTESIAN_POINT('Ctrl Pts',(3.11743648472242,4.08692256940132,7.93183294366476));
#11098=CARTESIAN_POINT('Ctrl Pts',(2.78054770698615,4.32497351435593,7.95445273793627));
#11099=CARTESIAN_POINT('Ctrl Pts',(2.5884261283377,4.44262255558441,7.96675956819401));
#11100=CARTESIAN_POINT('Ctrl Pts',(2.10820033422106,4.69493937488908,7.9961965505212));
#11101=CARTESIAN_POINT('Ctrl Pts',(1.81411126625045,4.81621932101812,8.01314528483233));
#11102=CARTESIAN_POINT('Ctrl Pts',(1.38244396156637,4.94904631125324,8.03738545033428));
#11103=CARTESIAN_POINT('Ctrl Pts',(1.25268244173541,4.98347233519436,8.04460249167849));
#11104=CARTESIAN_POINT('Ctrl Pts',(0.938400275493735,5.05380009908791,8.06209008455252));
#11105=CARTESIAN_POINT('Ctrl Pts',(0.752967681060348,5.08473485470611,8.07239820350146));
#11106=CARTESIAN_POINT('Ctrl Pts',(0.347051752675588,5.12975626699935,8.0947914169983));
#11107=CARTESIAN_POINT('Ctrl Pts',(0.126500503417814,5.13992658941099,8.10684658735286));
#11108=CARTESIAN_POINT('Ctrl Pts',(-0.391286155929265,5.13044738554987,
8.13493782728548));
#11109=CARTESIAN_POINT('Ctrl Pts',(-0.687516963178789,5.09920773431871,
8.1508297683649));
#11110=CARTESIAN_POINT('Ctrl Pts',(-1.1225351821779,5.01471647054983,8.17460282635074));
#11111=CARTESIAN_POINT('Ctrl Pts',(-1.26443690610858,4.98082971179623,8.18243641530185));
#11112=CARTESIAN_POINT('Ctrl Pts',(-1.6013561040864,4.88504425765085,8.20144892022648));
#11113=CARTESIAN_POINT('Ctrl Pts',(-1.7944939123785,4.81744626305338,8.21267449240564));
#11114=CARTESIAN_POINT('Ctrl Pts',(-2.18963931515588,4.65207662813501,8.23615723463917));
#11115=CARTESIAN_POINT('Ctrl Pts',(-2.39032342437481,4.55221869165,8.24838315455969));
#11116=CARTESIAN_POINT('Ctrl Pts',(-2.79869236062219,4.31454651966576,8.27398290723136));
#11117=CARTESIAN_POINT('Ctrl Pts',(-3.00417370239928,4.17407881933512,8.28729817806015));
#11118=CARTESIAN_POINT('Ctrl Pts',(-3.32947334607747,3.91519475790035,8.30958846485193));
#11119=CARTESIAN_POINT('Ctrl Pts',(-3.45510707732345,3.80478329143979,8.31854826171555));
#11120=CARTESIAN_POINT('Ctrl Pts',(-3.74476813162638,3.52402104508847,8.3404146004508));
#11121=CARTESIAN_POINT('Ctrl Pts',(-3.90285678186919,3.34809175122058,8.35340004403069));
#11122=CARTESIAN_POINT('Ctrl Pts',(-4.13404672687069,3.05209360572302,8.3739803016593));
#11123=CARTESIAN_POINT('Ctrl Pts',(-4.21529978690164,2.93885191876446,8.38159494541361));
#11124=CARTESIAN_POINT('Ctrl Pts',(-4.2918361854396,2.82247103082588,8.38917442239304));
#11125=CARTESIAN_POINT('',(-5.13674999998633,-1.18511375680025E-5,6.32404150530312));
#11126=CARTESIAN_POINT('Ctrl Pts',(-4.29183622825303,2.82247096572398,7.9120163777544));
#11127=CARTESIAN_POINT('Ctrl Pts',(-4.21009995288661,2.946758766038,7.90394870207524));
#11128=CARTESIAN_POINT('Ctrl Pts',(-4.12294775268111,3.06751403657549,7.89588102639609));
#11129=CARTESIAN_POINT('Ctrl Pts',(-4.0307097059894,3.18427069021194,7.88781335071693));
#11130=CARTESIAN_POINT('Ctrl Pts',(-3.938487576668,3.3010071953418,7.8797470672635));
#11131=CARTESIAN_POINT('Ctrl Pts',(-3.8411815570887,3.41374620077307,7.87168078381006));
#11132=CARTESIAN_POINT('Ctrl Pts',(-3.73916284912825,3.52205362682045,7.86361450035663));
#11133=CARTESIAN_POINT('Ctrl Pts',(-3.63713879186065,3.63036673192122,7.85554779395108));
#11134=CARTESIAN_POINT('Ctrl Pts',(-3.53040177689899,3.73424755003897,7.84748108754553));
#11135=CARTESIAN_POINT('Ctrl Pts',(-3.41936117223181,3.83329750167313,7.83941438113999));
#11136=CARTESIAN_POINT('Ctrl Pts',(-3.30832402994983,3.93234436480569,7.83134792626445));
#11137=CARTESIAN_POINT('Ctrl Pts',(-3.19298381480945,4.02656044402617,7.82328147138892));
#11138=CARTESIAN_POINT('Ctrl Pts',(-3.07378440728717,4.11558622555988,7.81521501651338));
#11139=CARTESIAN_POINT('Ctrl Pts',(-2.95455811294958,4.20463208789598,7.80714674215496));
#11140=CARTESIAN_POINT('Ctrl Pts',(-2.83147115284758,4.28848511611201,7.79907846779654));
#11141=CARTESIAN_POINT('Ctrl Pts',(-2.70499840189602,4.36682770535316,7.79101019343812));
#11142=CARTESIAN_POINT('Ctrl Pts',(-2.65212293018557,4.39958101648127,7.78763702562623));
#11143=CARTESIAN_POINT('Ctrl Pts',(-2.59865600441084,4.43137168571285,7.78426385781434));
#11144=CARTESIAN_POINT('Ctrl Pts',(-2.54463373986122,4.46217880552314,7.78089069000245));
#11145=CARTESIAN_POINT('Ctrl Pts',(-2.41541786179681,4.53586636879189,7.77282240844658));
#11146=CARTESIAN_POINT('Ctrl Pts',(-2.28297517347506,4.60395102761205,7.76475412689072));
#11147=CARTESIAN_POINT('Ctrl Pts',(-2.14781086612749,4.66616641857582,7.75668584533485));
#11148=CARTESIAN_POINT('Ctrl Pts',(-2.01267383706738,4.72836925349316,7.74861919208537));
#11149=CARTESIAN_POINT('Ctrl Pts',(-1.87481658528843,4.78470504536419,7.74055253883589));
#11150=CARTESIAN_POINT('Ctrl Pts',(-1.73476651462124,4.83495457085678,7.7324858855864));
#11151=CARTESIAN_POINT('Ctrl Pts',(-1.59471139524434,4.88520590781056,7.72441894153956));
#11152=CARTESIAN_POINT('Ctrl Pts',(-1.45246360907001,4.92937042399138,7.71635199749271));
#11153=CARTESIAN_POINT('Ctrl Pts',(-1.30856857724477,4.96727780994254,7.70828505344587));
#11154=CARTESIAN_POINT('Ctrl Pts',(-1.16468224982467,5.00518290282465,7.70021859737939));
#11155=CARTESIAN_POINT('Ctrl Pts',(-1.01914919641765,5.03683153917223,7.69215214131291));
#11156=CARTESIAN_POINT('Ctrl Pts',(-0.87252796420602,5.06210386244479,7.68408568524642));
#11157=CARTESIAN_POINT('Ctrl Pts',(-0.725870141087082,5.08738249269776,
7.67601721610897));
#11158=CARTESIAN_POINT('Ctrl Pts',(-0.578123922775169,5.10628157328747,
7.66794874697151));
#11159=CARTESIAN_POINT('Ctrl Pts',(-0.429856649723374,5.11873263837726,
7.65988027783406));
#11160=CARTESIAN_POINT('Ctrl Pts',(-0.320003723731571,5.12795777554795,
7.65390225635447));
#11161=CARTESIAN_POINT('Ctrl Pts',(-0.209864963383611,5.1336443408075,7.64792423487488));
#11162=CARTESIAN_POINT('Ctrl Pts',(-0.099672473439093,5.13578289655419,
7.64194621339529));
#11163=CARTESIAN_POINT('Ctrl Pts',(0.0490496476247377,5.13866921436787,
7.63387793183946));
#11164=CARTESIAN_POINT('Ctrl Pts',(0.197924721660986,5.13509167512214,7.62580965028363));
#11165=CARTESIAN_POINT('Ctrl Pts',(0.346381691016817,5.12505807641517,7.61774136872781));
#11166=CARTESIAN_POINT('Ctrl Pts',(0.494808699416362,5.11502650264655,7.60967471547836));
#11167=CARTESIAN_POINT('Ctrl Pts',(0.642817441416092,5.09854149111461,7.60160806222892));
#11168=CARTESIAN_POINT('Ctrl Pts',(0.789839907090891,5.07566286150554,7.59354140897947));
#11169=CARTESIAN_POINT('Ctrl Pts',(0.936867672825632,5.05278340713744,7.58547446493266));
#11170=CARTESIAN_POINT('Ctrl Pts',(1.08290876344197,5.02350992062861,7.57740752088585));
#11171=CARTESIAN_POINT('Ctrl Pts',(1.22740274936792,4.98795379422706,7.56934057683904));
#11172=CARTESIAN_POINT('Ctrl Pts',(1.3718879946571,4.95239981866371,7.56127412077259));
#11173=CARTESIAN_POINT('Ctrl Pts',(1.51482600124082,4.91056404341939,7.55320766470614));
#11174=CARTESIAN_POINT('Ctrl Pts',(1.65566895138303,4.86260844464431,7.54514120863969));
#11175=CARTESIAN_POINT('Ctrl Pts',(1.79654705040012,4.81464087803316,7.53707273950227));
#11176=CARTESIAN_POINT('Ctrl Pts',(1.9353287345135,4.76055054223209,7.52900427036485));
#11177=CARTESIAN_POINT('Ctrl Pts',(2.07148305120219,4.70054874786785,7.52093580122742));
#11178=CARTESIAN_POINT('Ctrl Pts',(2.17236134866681,4.65609272908348,7.51495777974765));
#11179=CARTESIAN_POINT('Ctrl Pts',(2.27179768844976,4.60839264641327,7.50897975826787));
#11180=CARTESIAN_POINT('Ctrl Pts',(2.36958373807782,4.55755125815795,7.5030017367881));
#11181=CARTESIAN_POINT('Ctrl Pts',(2.50156141385262,4.48893279692935,7.49493345523226));
#11182=CARTESIAN_POINT('Ctrl Pts',(2.63058090336597,4.41456507690165,7.48686517367642));
#11183=CARTESIAN_POINT('Ctrl Pts',(2.75614447658439,4.33472815603163,7.47879689212058));
#11184=CARTESIAN_POINT('Ctrl Pts',(2.88168270909485,4.25490734751047,7.47073023887112));
#11185=CARTESIAN_POINT('Ctrl Pts',(3.0037661375973,4.16961971769966,7.46266358562165));
#11186=CARTESIAN_POINT('Ctrl Pts',(3.12192459723588,4.07918954838747,7.45459693237219));
#11187=CARTESIAN_POINT('Ctrl Pts',(3.24008731640648,3.98875611912925,7.44652998832537));
#11188=CARTESIAN_POINT('Ctrl Pts',(3.35432451842213,3.89317997756405,7.43846304427855));
#11189=CARTESIAN_POINT('Ctrl Pts',(3.46419736875478,3.79282706603035,7.43039610023173));
#11190=CARTESIAN_POINT('Ctrl Pts',(3.57406357272995,3.69248022498015,7.42232964416527));
#11191=CARTESIAN_POINT('Ctrl Pts',(3.67956570932188,3.58735741589004,7.41426318809882));
#11192=CARTESIAN_POINT('Ctrl Pts',(3.78030021960309,3.47786296627237,7.40619673203236));
#11193=CARTESIAN_POINT('Ctrl Pts',(3.88105986926614,3.36834119113567,7.39812826289493));
#11194=CARTESIAN_POINT('Ctrl Pts',(3.97704929042786,3.25444583873924,7.3900597937575));
#11195=CARTESIAN_POINT('Ctrl Pts',(4.06790333700283,3.13661648967501,7.38199132462007));
#11196=CARTESIAN_POINT('Ctrl Pts',(4.13521814390037,3.04931537125343,7.37601330314035));
#11197=CARTESIAN_POINT('Ctrl Pts',(4.1997146750762,2.95985543037342,7.37003528166063));
#11198=CARTESIAN_POINT('Ctrl Pts',(4.26125915092337,2.86842657412943,7.3640572601809));
#11199=CARTESIAN_POINT('Ctrl Pts',(4.34432311464882,2.7450289321157,7.35598897862506));
#11200=CARTESIAN_POINT('Ctrl Pts',(4.42203880424172,2.6179979986879,7.34792069706922));
#11201=CARTESIAN_POINT('Ctrl Pts',(4.49410313788345,2.48781782865349,7.33985241551337));
#11202=CARTESIAN_POINT('Ctrl Pts',(4.56615292780693,2.35766393102898,7.3317857622639));
#11203=CARTESIAN_POINT('Ctrl Pts',(4.63255347695501,2.22436235419458,7.32371910901443));
#11204=CARTESIAN_POINT('Ctrl Pts',(4.6930470671855,2.08842279907149,7.31565245576496));
#11205=CARTESIAN_POINT('Ctrl Pts',(4.75354283816872,1.95247834341999,7.30758551171813));
#11206=CARTESIAN_POINT('Ctrl Pts',(4.80813108609039,1.81389602005319,7.2995185676713));
#11207=CARTESIAN_POINT('Ctrl Pts',(4.85660153641266,1.67320712376387,7.29145162362447));
#11208=CARTESIAN_POINT('Ctrl Pts',(4.90506905469177,1.53252673793637,7.28338516755801));
#11209=CARTESIAN_POINT('Ctrl Pts',(4.94741940868861,1.38974034736346,7.27531871149155));
#11210=CARTESIAN_POINT('Ctrl Pts',(4.9834916648809,1.24539607698216,7.26725225542509));
#11211=CARTESIAN_POINT('Ctrl Pts',(5.01957292329318,1.10101578393377,7.25918378628765));
#11212=CARTESIAN_POINT('Ctrl Pts',(5.04937287226009,0.955077155346015,7.25111531715021));
#11213=CARTESIAN_POINT('Ctrl Pts',(5.07278117568299,0.808140894978314,7.24304684801278));
#11214=CARTESIAN_POINT('Ctrl Pts',(5.09012465661863,0.699274131573728,7.23706882653309));
#11215=CARTESIAN_POINT('Ctrl Pts',(5.10396049227048,0.589859995340661,7.23109080505341));
#11216=CARTESIAN_POINT('Ctrl Pts',(5.11426206438136,0.480129252732794,7.22511278357372));
#11217=CARTESIAN_POINT('Ctrl Pts',(5.12816565849535,0.3320303324295,7.21704450201789));
#11218=CARTESIAN_POINT('Ctrl Pts',(5.13563452060422,0.183299694848691,7.20897622046205));
#11219=CARTESIAN_POINT('Ctrl Pts',(5.13663409262762,0.0345074043590885,
7.20090793890621));
#11220=CARTESIAN_POINT('Ctrl Pts',(5.13763346292164,-0.114254857501211,
7.19284128565676));
#11221=CARTESIAN_POINT('Ctrl Pts',(5.13216614562539,-0.263078416641545,
7.1847746324073));
#11222=CARTESIAN_POINT('Ctrl Pts',(5.12024968753788,-0.411392391480728,
7.17670797915785));
#11223=CARTESIAN_POINT('Ctrl Pts',(5.10833279987017,-0.559711712937808,
7.16864103511103));
#11224=CARTESIAN_POINT('Ctrl Pts',(5.08996632892319,-0.707521083093384,
7.16057409106421));
#11225=CARTESIAN_POINT('Ctrl Pts',(5.06521981410316,-0.854253356631802,
7.15250714701739));
#11226=CARTESIAN_POINT('Ctrl Pts',(5.04047479623331,-1.00097675413638,7.14444069095094));
#11227=CARTESIAN_POINT('Ctrl Pts',(5.00935056245525,-1.14662285909008,7.13637423488449));
#11228=CARTESIAN_POINT('Ctrl Pts',(4.97196803184221,-1.29063335337309,7.12830777881803));
#11229=CARTESIAN_POINT('Ctrl Pts',(4.93457617201611,-1.43467978702572,7.1202393096806));
#11230=CARTESIAN_POINT('Ctrl Pts',(4.89092297709436,-1.57708947365403,7.11217084054318));
#11231=CARTESIAN_POINT('Ctrl Pts',(4.84117981514528,-1.71731725663313,7.10410237140575));
#11232=CARTESIAN_POINT('Ctrl Pts',(4.80432453497542,-1.82121363207028,7.09812434992601));
#11233=CARTESIAN_POINT('Ctrl Pts',(4.76412722074456,-1.92391250978888,7.09214632844627));
#11234=CARTESIAN_POINT('Ctrl Pts',(4.72067490368666,-2.02519851278904,7.08616830696653));
#11235=CARTESIAN_POINT('Ctrl Pts',(4.66202915785498,-2.16189992690095,7.07810002541068));
#11236=CARTESIAN_POINT('Ctrl Pts',(4.59743067384917,-2.2960775044637,7.07003174385483));
#11237=CARTESIAN_POINT('Ctrl Pts',(4.52712184078284,-2.42721412347716,7.06196346229899));
#11238=CARTESIAN_POINT('Ctrl Pts',(4.45682719714717,-2.55832427705406,7.05389680904952));
#11239=CARTESIAN_POINT('Ctrl Pts',(4.38082465991316,-2.6863944049046,7.04583015580006));
#11240=CARTESIAN_POINT('Ctrl Pts',(4.29940276382755,-2.81093159591122,7.0377635025506));
#11241=CARTESIAN_POINT('Ctrl Pts',(4.21797793253794,-2.93547327639891,7.02969655850377));
#11242=CARTESIAN_POINT('Ctrl Pts',(4.13113352942016,-3.05648148607089,7.02162961445694));
#11243=CARTESIAN_POINT('Ctrl Pts',(4.03920195774788,-3.17349146950574,7.01356267041011));
#11244=CARTESIAN_POINT('Ctrl Pts',(3.94727594714088,-3.29049437484822,7.00549621434365));
#11245=CARTESIAN_POINT('Ctrl Pts',(3.85026358877736,-3.40349927802166,6.99742975827719));
#11246=CARTESIAN_POINT('Ctrl Pts',(3.74853818056925,-3.51207375653112,6.98936330221073));
#11247=CARTESIAN_POINT('Ctrl Pts',(3.64678738569001,-3.62067533097094,6.98129483307329));
#11248=CARTESIAN_POINT('Ctrl Pts',(3.54032141665499,-3.72484402929224,6.97322636393585));
#11249=CARTESIAN_POINT('Ctrl Pts',(3.42955157511154,-3.82418312272699,6.9651578947984));
#11250=CARTESIAN_POINT('Ctrl Pts',(3.34748092691687,-3.89778459832415,6.95917987331872));
#11251=CARTESIAN_POINT('Ctrl Pts',(3.2630484692996,-3.96873559307783,6.95320185183903));
#11252=CARTESIAN_POINT('Ctrl Pts',(3.17643366931386,-4.03688861710962,6.94722383035934));
#11253=CARTESIAN_POINT('Ctrl Pts',(3.05953335445872,-4.12887185749071,6.93915554880351));
#11254=CARTESIAN_POINT('Ctrl Pts',(2.93861326203309,-4.21579088707642,6.93108726724769));
#11255=CARTESIAN_POINT('Ctrl Pts',(2.81413364653386,-4.29730757357977,6.92301898569186));
#11256=CARTESIAN_POINT('Ctrl Pts',(2.68967915298276,-4.37880780873113,6.91495233244241));
#11257=CARTESIAN_POINT('Ctrl Pts',(2.56166684627373,-4.4549076947012,6.90688567919295));
#11258=CARTESIAN_POINT('Ctrl Pts',(2.43058591939444,-4.52531243683146,6.89881902594349));
#11259=CARTESIAN_POINT('Ctrl Pts',(2.29950026713706,-4.5957197170047,6.89075208189668));
#11260=CARTESIAN_POINT('Ctrl Pts',(2.16534606315687,-4.66043128254934,6.88268513784987));
#11261=CARTESIAN_POINT('Ctrl Pts',(2.02863755203179,-4.71919805104495,6.87461819380306));
#11262=CARTESIAN_POINT('Ctrl Pts',(1.8919373105896,-4.77796126465919,6.86655173773661));
#11263=CARTESIAN_POINT('Ctrl Pts',(1.75268337556592,-4.83078027067817,6.85848528167017));
#11264=CARTESIAN_POINT('Ctrl Pts',(1.61141043317042,-4.87745394425919,6.85041882560372));
#11265=CARTESIAN_POINT('Ctrl Pts',(1.47010223459086,-4.92413926575805,6.8423503564663));
#11266=CARTESIAN_POINT('Ctrl Pts',(1.32677433607392,-4.96467608580011,6.83428188732888));
#11267=CARTESIAN_POINT('Ctrl Pts',(1.1819777189786,-4.99891280523457,6.82621341819146));
#11268=CARTESIAN_POINT('Ctrl Pts',(1.07469624185444,-5.02427918399739,6.8202353967117));
#11269=CARTESIAN_POINT('Ctrl Pts',(0.966608865772434,-5.04618814763894,
6.81425737523193));
#11270=CARTESIAN_POINT('Ctrl Pts',(0.857943748909188,-5.06459604373415,
6.80827935375217));
#11271=CARTESIAN_POINT('Ctrl Pts',(0.711283058391623,-5.08944039885225,
6.80021107219632));
#11272=CARTESIAN_POINT('Ctrl Pts',(0.563515362805088,-5.10791455911667,
6.79214279064048));
#11273=CARTESIAN_POINT('Ctrl Pts',(0.415206596013435,-5.11994180095115,
6.78407450908464));
#11274=CARTESIAN_POINT('Ctrl Pts',(0.26692776026831,-5.13196661549868,6.77600785583518));
#11275=CARTESIAN_POINT('Ctrl Pts',(0.118108400899065,-5.13754708058652,
6.76794120258571));
#11276=CARTESIAN_POINT('Ctrl Pts',(-0.0306808705751501,-5.13665837356162,
6.75987454933624));
#11277=CARTESIAN_POINT('Ctrl Pts',(-0.179475505801333,-5.13576963449945,
6.75180760528942));
#11278=CARTESIAN_POINT('Ctrl Pts',(-0.328239719944949,-5.12841125484726,
6.74374066124259));
#11279=CARTESIAN_POINT('Ctrl Pts',(-0.476402773103094,-5.11461053847502,
6.73567371719577));
#11280=CARTESIAN_POINT('Ctrl Pts',(-0.62455686367748,-5.1008106569268,6.72760726112931));
#11281=CARTESIAN_POINT('Ctrl Pts',(-0.772109536492282,-5.08056924981998,
6.71954080506286));
#11282=CARTESIAN_POINT('Ctrl Pts',(-0.91849504562186,-5.05396551369992,
6.71147434899641));
#11283=CARTESIAN_POINT('Ctrl Pts',(-1.06491708683173,-5.02735513833101,
6.70340587985897));
#11284=CARTESIAN_POINT('Ctrl Pts',(-1.21017105636499,-4.99437931980706,
6.69533741072153));
#11285=CARTESIAN_POINT('Ctrl Pts',(-1.35370059363943,-4.95516854055241,
6.6872689415841));
#11286=CARTESIAN_POINT('Ctrl Pts',(-1.46004327676605,-4.92611682372389,
6.68129092010439));
#11287=CARTESIAN_POINT('Ctrl Pts',(-1.565439512296,-4.89364349479034,6.67531289862468));
#11288=CARTESIAN_POINT('Ctrl Pts',(-1.66966806398151,-4.85781937896215,
6.66933487714497));
#11289=CARTESIAN_POINT('Ctrl Pts',(-1.81034091101133,-4.80946909217047,
6.66126659558913));
#11290=CARTESIAN_POINT('Ctrl Pts',(-1.94893816056983,-4.75499534738238,
6.65319831403329));
#11291=CARTESIAN_POINT('Ctrl Pts',(-2.08492614455465,-4.69460153093449,
6.64513003247745));
#11292=CARTESIAN_POINT('Ctrl Pts',(-2.22088668402104,-4.63421990291061,
6.63706337922799));
#11293=CARTESIAN_POINT('Ctrl Pts',(-2.35423870613906,-4.56792072108554,
6.62899672597853));
#11294=CARTESIAN_POINT('Ctrl Pts',(-2.48446926615469,-4.49595518527851,
6.62093007272907));
#11295=CARTESIAN_POINT('Ctrl Pts',(-2.61470452089347,-4.42398705516285,
6.61286312868224));
#11296=CARTESIAN_POINT('Ctrl Pts',(-2.74181779681594,-4.34635231908976,
6.60479618463541));
#11297=CARTESIAN_POINT('Ctrl Pts',(-2.86532097528403,-4.26334801196165,
6.59672924058859));
#11298=CARTESIAN_POINT('Ctrl Pts',(-2.98881668287759,-4.1803487258765,6.58866278452213));
#11299=CARTESIAN_POINT('Ctrl Pts',(-3.10870245562007,-4.09198070388662,
6.58059632845568));
#11300=CARTESIAN_POINT('Ctrl Pts',(-3.22451938718877,-3.99858415994258,
6.57252987238922));
#11301=CARTESIAN_POINT('Ctrl Pts',(-3.34036522212005,-3.90516430788517,
6.56446140325178));
#11302=CARTESIAN_POINT('Ctrl Pts',(-3.4521399286501,-3.80671363367402,6.55639293411435));
#11303=CARTESIAN_POINT('Ctrl Pts',(-3.5594173786357,-3.70361289650608,6.54832446497691));
#11304=CARTESIAN_POINT('Ctrl Pts',(-3.6389004738026,-3.62722437585056,6.5423464434972));
#11305=CARTESIAN_POINT('Ctrl Pts',(-3.71591546932809,-3.548284056494,6.53636842201749));
#11306=CARTESIAN_POINT('Ctrl Pts',(-3.79030197673961,-3.46695997779378,
6.53039040053778));
#11307=CARTESIAN_POINT('Ctrl Pts',(-3.89069828474704,-3.35720032462925,
6.52232211898194));
#11308=CARTESIAN_POINT('Ctrl Pts',(-3.98634231503882,-3.24305652967757,
6.5142538374261));
#11309=CARTESIAN_POINT('Ctrl Pts',(-4.07686274569445,-3.12496251421817,
6.50618555587026));
#11310=CARTESIAN_POINT('Ctrl Pts',(-4.16736490790042,-3.00689233199244,
6.4981189026208));
#11311=CARTESIAN_POINT('Ctrl Pts',(-4.25274533212363,-2.88487378228349,
6.49005224937135));
#11312=CARTESIAN_POINT('Ctrl Pts',(-4.33267376952517,-2.75937285798214,
6.4819855961219));
#11313=CARTESIAN_POINT('Ctrl Pts',(-4.41260508829257,-2.63386740945775,
6.47391865207507));
#11314=CARTESIAN_POINT('Ctrl Pts',(-4.48708384594589,-2.50487961228577,
6.46585170802825));
#11315=CARTESIAN_POINT('Ctrl Pts',(-4.55582352295105,-2.37290383080013,
6.45778476398143));
#11316=CARTESIAN_POINT('Ctrl Pts',(-4.62455904179996,-2.2409360327084,6.44971830791498));
#11317=CARTESIAN_POINT('Ctrl Pts',(-4.68755602234724,-2.10598090587611,
6.44165185184854));
#11318=CARTESIAN_POINT('Ctrl Pts',(-4.74457425527497,-1.96855675526055,
6.4335853957821));
#11319=CARTESIAN_POINT('Ctrl Pts',(-4.80160671771683,-1.83109830896811,
6.42551692664467));
#11320=CARTESIAN_POINT('Ctrl Pts',(-4.85265732358227,-1.69116991330361,
6.41744845750724));
#11321=CARTESIAN_POINT('Ctrl Pts',(-4.89753404496007,-1.54930979502393,
6.40937998836981));
#11322=CARTESIAN_POINT('Ctrl Pts',(-4.9307837234018,-1.44420400360935,6.40340196689007));
#11323=CARTESIAN_POINT('Ctrl Pts',(-4.96064524398971,-1.33803822219086,
6.39742394541034));
#11324=CARTESIAN_POINT('Ctrl Pts',(-4.98705816036214,-1.23103674505086,
6.3914459239306));
#11325=CARTESIAN_POINT('Ctrl Pts',(-5.02320823666945,-1.0845890181484,6.38326409616073));
#11326=CARTESIAN_POINT('Ctrl Pts',(-5.05290817629628,-0.936528220354522,
6.37508226839086));
#11327=CARTESIAN_POINT('Ctrl Pts',(-5.07603746558229,-0.787428860599461,
6.36690044062098));
#11328=CARTESIAN_POINT('Ctrl Pts',(-5.09916160595338,-0.638362692522116,
6.35872043424451));
#11329=CARTESIAN_POINT('Ctrl Pts',(-5.11571796687674,-0.488258730911634,
6.35054042786805));
#11330=CARTESIAN_POINT('Ctrl Pts',(-5.12563745358772,-0.33769995096059,
6.34236042149158));
#11331=CARTESIAN_POINT('Ctrl Pts',(-5.13304226630334,-0.225309098418272,
6.33625411609542));
#11332=CARTESIAN_POINT('Ctrl Pts',(-5.13674974008113,-0.112665007672855,
6.33014781069927));
#11333=CARTESIAN_POINT('Ctrl Pts',(-5.13674999998633,-1.18511375680025E-5,
6.32404150530312));
#11334=CARTESIAN_POINT('Ctrl Pts',(-5.13674999993655,-2.55313104141619E-5,
6.32378934850487));
#11335=CARTESIAN_POINT('Ctrl Pts',(-5.13675175881838,0.353851183330079,
6.30459076071832));
#11336=CARTESIAN_POINT('Ctrl Pts',(-5.10018553184707,0.706781009868396,
6.28575565506401));
#11337=CARTESIAN_POINT('Ctrl Pts',(-5.01097029336203,1.13268802209302,6.26235343972258));
#11338=CARTESIAN_POINT('Ctrl Pts',(-4.99242291290921,1.21182448726008,6.25797201038631));
#11339=CARTESIAN_POINT('Ctrl Pts',(-4.90528205000358,1.54756212131146,6.23917043738623));
#11340=CARTESIAN_POINT('Ctrl Pts',(-4.81872142881228,1.7990722902529,6.22455421264983));
#11341=CARTESIAN_POINT('Ctrl Pts',(-4.65257091141745,2.18241944463084,6.20168245279317));
#11342=CARTESIAN_POINT('Ctrl Pts',(-4.58585904589532,2.31932507128563,6.1933810177971));
#11343=CARTESIAN_POINT('Ctrl Pts',(-4.44454904821096,2.57930788189307,6.17732565126477));
#11344=CARTESIAN_POINT('Ctrl Pts',(-4.37070278764835,2.7025468175416,6.16957809495441));
#11345=CARTESIAN_POINT('Ctrl Pts',(-4.29183649439967,2.8224705610226,6.16186016520308));
#11346=CARTESIAN_POINT('Origin',(0.,0.,0.));
#11347=CARTESIAN_POINT('',(-4.29183634723918,2.82247078479419,4.41198748894216));
#11348=CARTESIAN_POINT('',(-4.29183618112783,2.82247103738233,4.88896334675683));
#11349=CARTESIAN_POINT('',(-4.29183622825304,2.82247096572397,0.));
#11350=CARTESIAN_POINT('Ctrl Pts',(-4.29183618112783,2.82247103738234,4.88896334675683));
#11351=CARTESIAN_POINT('Ctrl Pts',(-4.35076667494944,2.73286160571572,4.89484305890014));
#11352=CARTESIAN_POINT('Ctrl Pts',(-4.40688922721175,2.64140882838337,4.90071687591498));
#11353=CARTESIAN_POINT('Ctrl Pts',(-4.49902899138872,2.4801393544412,4.91085775786024));
#11354=CARTESIAN_POINT('Ctrl Pts',(-4.53637581793597,2.41115070099564,4.91513024842132));
#11355=CARTESIAN_POINT('Ctrl Pts',(-4.65490048988083,2.17969711237887,4.92925757696788));
#11356=CARTESIAN_POINT('Ctrl Pts',(-4.72904407135895,2.01378308427835,4.93904982177472));
#11357=CARTESIAN_POINT('Ctrl Pts',(-4.86203773616973,1.66806482258989,4.95895017141693));
#11358=CARTESIAN_POINT('Ctrl Pts',(-4.92006091600445,1.48823766118503,4.96904016528542));
#11359=CARTESIAN_POINT('Ctrl Pts',(-4.98148356785063,1.25451763246555,4.98203334701867));
#11360=CARTESIAN_POINT('Ctrl Pts',(-4.99412551682467,1.20320541802812,4.98487908351888));
#11361=CARTESIAN_POINT('Ctrl Pts',(-5.02848941190195,1.05384047643724,4.99315588135523));
#11362=CARTESIAN_POINT('Ctrl Pts',(-5.04812996977751,0.955336836620863,
4.9986127844951));
#11363=CARTESIAN_POINT('Ctrl Pts',(-5.09815841771197,0.659434726490387,
5.01499992341947));
#11364=CARTESIAN_POINT('Ctrl Pts',(-5.11993756290548,0.460773957801797,
5.02597188807525));
#11365=CARTESIAN_POINT('Ctrl Pts',(-5.13453025535386,0.174331876064929,
5.04167125775976));
#11366=CARTESIAN_POINT('Ctrl Pts',(-5.13674863816779,0.0872134508755163,
5.04643134595567));
#11367=CARTESIAN_POINT('Ctrl Pts',(-5.13675261505373,-0.167352117693572,
5.06030159264728));
#11368=CARTESIAN_POINT('Ctrl Pts',(-5.12856906637668,-0.334686869971494,
5.06936667163545));
#11369=CARTESIAN_POINT('Ctrl Pts',(-5.09454248799109,-0.681670387724374,
5.08815307217164));
#11370=CARTESIAN_POINT('Ctrl Pts',(-5.06732638629499,-0.860953938580389,
5.09785328912853));
#11371=CARTESIAN_POINT('Ctrl Pts',(-4.99886041106813,-1.1926403364,5.11601577130758));
#11372=CARTESIAN_POINT('Ctrl Pts',(-4.9599536683695,-1.34530826903399,5.12446531774806));
#11373=CARTESIAN_POINT('Ctrl Pts',(-4.82548190008043,-1.78704071595509,
5.14951732576378));
#11374=CARTESIAN_POINT('Ctrl Pts',(-4.71117701145238,-2.06968627579925,
5.16628477743318));
#11375=CARTESIAN_POINT('Ctrl Pts',(-4.4940214701316,-2.49392446646106,5.19231923691255));
#11376=CARTESIAN_POINT('Ctrl Pts',(-4.40784445491978,-2.64325508881694,
5.20167777347038));
#11377=CARTESIAN_POINT('Ctrl Pts',(-4.2703745437973,-2.8559865329779,5.21535912339026));
#11378=CARTESIAN_POINT('Ctrl Pts',(-4.22482191454289,-2.92295018554061,
5.21972072900632));
#11379=CARTESIAN_POINT('Ctrl Pts',(-4.11009496461746,-3.08331349243077,
5.23032162209334));
#11380=CARTESIAN_POINT('Ctrl Pts',(-4.03929751456115,-3.17549657449616,
5.23654896067303));
#11381=CARTESIAN_POINT('Ctrl Pts',(-3.85270804337653,-3.40210090516477,
5.25228662469231));
#11382=CARTESIAN_POINT('Ctrl Pts',(-3.7329695374097,-3.5330703291436,5.26178746264883));
#11383=CARTESIAN_POINT('Ctrl Pts',(-3.48367786934961,-3.7788940600989,5.28077396470312));
#11384=CARTESIAN_POINT('Ctrl Pts',(-3.35461436601722,-3.89391993255668,
5.29024323451936));
#11385=CARTESIAN_POINT('Ctrl Pts',(-3.02579250576841,-4.15847485742709,
5.31338563258738));
#11386=CARTESIAN_POINT('Ctrl Pts',(-2.82046177660664,-4.30038760683045,
5.32702240745528));
#11387=CARTESIAN_POINT('Ctrl Pts',(-2.41269658561049,-4.54039858685244,
5.35268131936462));
#11388=CARTESIAN_POINT('Ctrl Pts',(-2.2125347411642,-4.64123012568271,5.36470256018284));
#11389=CARTESIAN_POINT('Ctrl Pts',(-1.81818606140417,-4.80855655972018,
5.38767251058753));
#11390=CARTESIAN_POINT('Ctrl Pts',(-1.62534268444444,-4.87711747043902,
5.39860607350409));
#11391=CARTESIAN_POINT('Ctrl Pts',(-1.28883363923448,-4.97457354426541,
5.41759486411576));
#11392=CARTESIAN_POINT('Ctrl Pts',(-1.14707417045461,-5.00916093916427,
5.42557468777306));
#11393=CARTESIAN_POINT('Ctrl Pts',(-0.712504788672453,-5.09577329946574,
5.44986341754238));
#11394=CARTESIAN_POINT('Ctrl Pts',(-0.416469418077995,-5.12846270969461,
5.4661413171253));
#11395=CARTESIAN_POINT('Ctrl Pts',(0.101206793825572,-5.14048571251202,
5.49418906878275));
#11396=CARTESIAN_POINT('Ctrl Pts',(0.32178524065613,-5.13140262919381,5.50601932938985));
#11397=CARTESIAN_POINT('Ctrl Pts',(0.727947503460507,-5.08837864068416,
5.52791716391643));
#11398=CARTESIAN_POINT('Ctrl Pts',(0.913566335216109,-5.05834941959818,
5.53797288310535));
#11399=CARTESIAN_POINT('Ctrl Pts',(1.22824756609194,-4.98955160405469,5.55542530478754));
#11400=CARTESIAN_POINT('Ctrl Pts',(1.35819995898229,-4.95575510375443,5.56276205078095));
#11401=CARTESIAN_POINT('Ctrl Pts',(1.79047535739138,-4.82505233274795,5.58750611267025));
#11402=CARTESIAN_POINT('Ctrl Pts',(2.08511671918455,-4.70523430195556,5.60489516509617));
#11403=CARTESIAN_POINT('Ctrl Pts',(2.56115582484357,-4.45809705594016,5.63393677711287));
#11404=CARTESIAN_POINT('Ctrl Pts',(2.74884884910895,-4.34487984782121,5.64568003104302));
#11405=CARTESIAN_POINT('Ctrl Pts',(3.07900775626645,-4.11574606299812,5.66722605964057));
#11406=CARTESIAN_POINT('Ctrl Pts',(3.22359050743026,-4.0035130040499,5.67701737438513));
#11407=CARTESIAN_POINT('Ctrl Pts',(3.46097767781925,-3.79802763496036,5.6940262473911));
#11408=CARTESIAN_POINT('Ctrl Pts',(3.55675720378763,-3.70848447643342,5.70118848483755));
#11409=CARTESIAN_POINT('Ctrl Pts',(3.87672233774735,-3.38554336959448,5.72609369491122));
#11410=CARTESIAN_POINT('Ctrl Pts',(4.08222306912352,-3.13470012865412,5.74382306491193));
#11411=CARTESIAN_POINT('Ctrl Pts',(4.38607728400062,-2.68279145605713,5.77330449563059));
#11412=CARTESIAN_POINT('Ctrl Pts',(4.49742990286746,-2.4916200684532,5.78515406010949));
#11413=CARTESIAN_POINT('Ctrl Pts',(4.68108485635258,-2.12363886161213,5.80720310961879));
#11414=CARTESIAN_POINT('Ctrl Pts',(4.75652051110564,-1.94882207014414,5.81738869919237));
#11415=CARTESIAN_POINT('Ctrl Pts',(4.88407969953336,-1.60135214897491,5.83747048028227));
#11416=CARTESIAN_POINT('Ctrl Pts',(4.93714988064486,-1.42933474119038,5.84733204546999));
#11417=CARTESIAN_POINT('Ctrl Pts',(5.03972250490122,-1.02224261884155,5.87035297090975));
#11418=CARTESIAN_POINT('Ctrl Pts',(5.08201819096381,-0.785489198455414,
5.88349119731374));
#11419=CARTESIAN_POINT('Ctrl Pts',(5.1321025676287,-0.31752263634635,5.90901139921348));
#11420=CARTESIAN_POINT('Ctrl Pts',(5.14117978245887,-0.0870107790218277,
5.92137820564444));
#11421=CARTESIAN_POINT('Ctrl Pts',(5.1293031738,0.338454165328436,5.94419891307366));
#11422=CARTESIAN_POINT('Ctrl Pts',(5.11273914575662,0.533102216108032,5.95464119155864));
#11423=CARTESIAN_POINT('Ctrl Pts',(5.0654556216585,0.864140570948428,5.97276249389672));
#11424=CARTESIAN_POINT('Ctrl Pts',(5.04017813134208,1.00109061540283,5.98037479488938));
#11425=CARTESIAN_POINT('Ctrl Pts',(4.94113634553711,1.43750759598957,6.00489954169758));
#11426=CARTESIAN_POINT('Ctrl Pts',(4.84596944145801,1.73142872882405,6.02178748625493));
#11427=CARTESIAN_POINT('Ctrl Pts',(4.63611254522064,2.22351698621223,6.0507585970176));
#11428=CARTESIAN_POINT('Ctrl Pts',(4.53350467082986,2.42588236888161,6.06290992577457));
#11429=CARTESIAN_POINT('Ctrl Pts',(4.32150440810181,2.78324843096805,6.08518690693516));
#11430=CARTESIAN_POINT('Ctrl Pts',(4.21625801619962,2.94024453447699,6.09529909828665));
#11431=CARTESIAN_POINT('Ctrl Pts',(4.0008265096165,3.22617363943583,6.11472131811095));
#11432=CARTESIAN_POINT('Ctrl Pts',(3.89243590534358,3.35615110775703,6.12399112259118));
#11433=CARTESIAN_POINT('Ctrl Pts',(3.60845866095431,3.66438429088189,6.14697293205562));
#11434=CARTESIAN_POINT('Ctrl Pts',(3.42588686792987,3.83562121634691,6.16064877382191));
#11435=CARTESIAN_POINT('Ctrl Pts',(3.0575908520117,4.1336951366118,6.18634277346802));
#11436=CARTESIAN_POINT('Ctrl Pts',(2.87459021028,4.26298385421086,6.19836084857391));
#11437=CARTESIAN_POINT('Ctrl Pts',(2.50930445417532,4.48680764122961,6.2213321813699));
#11438=CARTESIAN_POINT('Ctrl Pts',(2.3286441985642,4.58317191110622,6.23227025220367));
#11439=CARTESIAN_POINT('Ctrl Pts',(2.01011045436244,4.72937073494544,6.25126694722387));
#11440=CARTESIAN_POINT('Ctrl Pts',(1.87496621935885,4.78455762145455,6.25925008577663));
#11441=CARTESIAN_POINT('Ctrl Pts',(1.45800616493269,4.93444325976642,6.28353694626568));
#11442=CARTESIAN_POINT('Ctrl Pts',(1.17014907750794,5.01051607499201,6.29980961136405));
#11443=CARTESIAN_POINT('Ctrl Pts',(0.660080505383652,5.0989321998958,6.32784977733062));
#11444=CARTESIAN_POINT('Ctrl Pts',(0.440630106783252,5.12256414988613,6.33967761486079));
#11445=CARTESIAN_POINT('Ctrl Pts',(0.0325309836741374,5.14008550698156,
6.3615776261939));
#11446=CARTESIAN_POINT('Ctrl Pts',(-0.155574449815248,5.13783333831406,
6.37163792855709));
#11447=CARTESIAN_POINT('Ctrl Pts',(-0.477111820295809,5.11630695044312,
6.38909814649617));
#11448=CARTESIAN_POINT('Ctrl Pts',(-0.610688937314607,5.10208682847716,
6.39643802524681));
#11449=CARTESIAN_POINT('Ctrl Pts',(-1.05748535164622,5.03672399017357,6.42117936172845));
#11450=CARTESIAN_POINT('Ctrl Pts',(-1.36649822918216,4.96180974567678,6.43856247765311));
#11451=CARTESIAN_POINT('Ctrl Pts',(-1.8727932559441,4.78814713298114,6.46754369058711));
#11452=CARTESIAN_POINT('Ctrl Pts',(-2.07425500578036,4.70437839353973,6.47923352004727));
#11453=CARTESIAN_POINT('Ctrl Pts',(-2.43505842376461,4.52665798603239,6.5007967269021));
#11454=CARTESIAN_POINT('Ctrl Pts',(-2.59582700116256,4.43641994168349,6.51065843586246));
#11455=CARTESIAN_POINT('Ctrl Pts',(-2.8627716029435,4.26709903664984,6.52778417868107));
#11456=CARTESIAN_POINT('Ctrl Pts',(-2.9713817741071,4.19219325645766,6.53499165756809));
#11457=CARTESIAN_POINT('Ctrl Pts',(-3.33219938525618,3.92227378166827,6.55967855836324));
#11458=CARTESIAN_POINT('Ctrl Pts',(-3.56909740785504,3.70800992819532,6.57714451091868));
#11459=CARTESIAN_POINT('Ctrl Pts',(-3.93920150163499,3.3047190286957,6.60678579541625));
#11460=CARTESIAN_POINT('Ctrl Pts',(-4.08237593636468,3.12612949197814,6.6190420456666));
#11461=CARTESIAN_POINT('Ctrl Pts',(-4.23992760663097,2.90024154009261,6.63380724808002));
#11462=CARTESIAN_POINT('Ctrl Pts',(-4.26614956753193,2.86152998221862,6.63631380382691));
#11463=CARTESIAN_POINT('Ctrl Pts',(-4.29183621579633,2.82247098466558,6.63882185511496));
#11464=CARTESIAN_POINT('Ctrl Pts',(-4.29183649439966,2.8224705610226,6.16186016520308));
#11465=CARTESIAN_POINT('Ctrl Pts',(-4.19725390933125,2.96629242968514,6.15260422432914));
#11466=CARTESIAN_POINT('Ctrl Pts',(-4.09545108415786,3.10534617699547,6.14339199955404));
#11467=CARTESIAN_POINT('Ctrl Pts',(-3.90218522766283,3.34322503928577,6.12694209094475));
#11468=CARTESIAN_POINT('Ctrl Pts',(-3.81353312405755,3.4440045650993,6.11972652822776));
#11469=CARTESIAN_POINT('Ctrl Pts',(-3.5915626956095,3.67724782599031,6.10224279270102));
#11470=CARTESIAN_POINT('Ctrl Pts',(-3.45472490639275,3.80609358067502,6.09193707841706));
#11471=CARTESIAN_POINT('Ctrl Pts',(-3.14250599113566,4.06933786739302,6.06954496239244));
#11472=CARTESIAN_POINT('Ctrl Pts',(-2.96488438196448,4.20051409112443,6.05748849496811));
#11473=CARTESIAN_POINT('Ctrl Pts',(-2.52930807527318,4.48076149686582,6.02939343924952));
#11474=CARTESIAN_POINT('Ctrl Pts',(-2.26573715376429,4.61963872422158,6.01349904927813));
#11475=CARTESIAN_POINT('Ctrl Pts',(-1.85723845235867,4.79146358774224,5.98972503912635));
#11476=CARTESIAN_POINT('Ctrl Pts',(-1.72050094412173,4.84224465263094,5.98189300166352));
#11477=CARTESIAN_POINT('Ctrl Pts',(-1.38731964776934,4.9500833824721,5.96288438992435));
#11478=CARTESIAN_POINT('Ctrl Pts',(-1.18926746821426,5.00136204605316,5.95166118322735));
#11479=CARTESIAN_POINT('Ctrl Pts',(-0.768935238839542,5.08380658744256,
5.92817911252273));
#11480=CARTESIAN_POINT('Ctrl Pts',(-0.546592339084737,5.11249366174593,
5.91595152211607));
#11481=CARTESIAN_POINT('Ctrl Pts',(-0.0759509131320661,5.14215418998918,
5.89040169538602));
#11482=CARTESIAN_POINT('Ctrl Pts',(0.171987736413737,5.13983866357537,5.87713661866262));
#11483=CARTESIAN_POINT('Ctrl Pts',(0.591263223056248,5.10554142019864,5.85458192794348));
#11484=CARTESIAN_POINT('Ctrl Pts',(0.762906708664317,5.08272727259404,5.84530766423137));
#11485=CARTESIAN_POINT('Ctrl Pts',(1.11226441971272,5.01819446413918,5.82603773727903));
#11486=CARTESIAN_POINT('Ctrl Pts',(1.28957095845087,4.97558272649148,5.81604448562454));
#11487=CARTESIAN_POINT('Ctrl Pts',(1.70149904446022,4.85307871146888,5.79247841485924));
#11488=CARTESIAN_POINT('Ctrl Pts',(1.93333421223393,4.76546796703958,5.7789475584529));
#11489=CARTESIAN_POINT('Ctrl Pts',(2.33117697936211,4.58129370685745,5.75518820385545));
#11490=CARTESIAN_POINT('Ctrl Pts',(2.49979930575679,4.49150793975523,5.74492616201104));
#11491=CARTESIAN_POINT('Ctrl Pts',(2.84107775545857,4.2846036322245,5.72351690090885));
#11492=CARTESIAN_POINT('Ctrl Pts',(3.01239072911943,4.16593935513081,5.71239424761735));
#11493=CARTESIAN_POINT('Ctrl Pts',(3.25970275563985,3.97138181260307,5.69538040988315));
#11494=CARTESIAN_POINT('Ctrl Pts',(3.34131024906505,3.90297070011646,5.68958316397548));
#11495=CARTESIAN_POINT('Ctrl Pts',(3.65899377046751,3.61938805472154,5.66630084388965));
#11496=CARTESIAN_POINT('Ctrl Pts',(3.87690797328752,3.38493682553852,5.64874946335737));
#11497=CARTESIAN_POINT('Ctrl Pts',(4.18533277008768,2.98395166433981,5.62127715473111));
#11498=CARTESIAN_POINT('Ctrl Pts',(4.29089743734252,2.83004934223808,5.6112282659875));
#11499=CARTESIAN_POINT('Ctrl Pts',(4.51526997353433,2.46141991961872,5.58805398293149));
#11500=CARTESIAN_POINT('Ctrl Pts',(4.62753520096295,2.24324883224769,5.57498893735118));
#11501=CARTESIAN_POINT('Ctrl Pts',(4.76659109010211,1.91772694692146,5.5558434368822));
#11502=CARTESIAN_POINT('Ctrl Pts',(4.80618591328844,1.81621669319552,5.54990852336167));
#11503=CARTESIAN_POINT('Ctrl Pts',(4.9073630203892,1.53028454583526,5.53332027145507));
#11504=CARTESIAN_POINT('Ctrl Pts',(4.96175024495561,1.34350938206039,5.52264265023909));
#11505=CARTESIAN_POINT('Ctrl Pts',(5.02416708917492,1.07280310674512,5.50744749504817));
#11506=CARTESIAN_POINT('Ctrl Pts',(5.04092883804701,0.991059076741259,5.50289366739454));
#11507=CARTESIAN_POINT('Ctrl Pts',(5.08561676379312,0.742497274432245,5.48914553749949));
#11508=CARTESIAN_POINT('Ctrl Pts',(5.10730382298176,0.574673438170269,5.47999985348081));
#11509=CARTESIAN_POINT('Ctrl Pts',(5.14612836540326,0.0850996471055538,
5.4535602820455));
#11510=CARTESIAN_POINT('Ctrl Pts',(5.14134576107469,-0.237559152087237,
5.43646659019121));
#11511=CARTESIAN_POINT('Ctrl Pts',(5.08679226888453,-0.737118438938526,
5.40920716678854));
#11512=CARTESIAN_POINT('Ctrl Pts',(5.05774296952375,-0.915441678129262,
5.39930679155705));
#11513=CARTESIAN_POINT('Ctrl Pts',(4.97043138119144,-1.31681923342578,5.37678220263966));
#11514=CARTESIAN_POINT('Ctrl Pts',(4.90642772221416,-1.53823657711337,5.36418932725019));
#11515=CARTESIAN_POINT('Ctrl Pts',(4.71934063016897,-2.05300270962597,5.33446833855216));
#11516=CARTESIAN_POINT('Ctrl Pts',(4.58346448588307,-2.3406950393242,5.31751698212112));
#11517=CARTESIAN_POINT('Ctrl Pts',(4.35362020290054,-2.72950449897037,5.29327550687882));
#11518=CARTESIAN_POINT('Ctrl Pts',(4.28084272351437,-2.84228576605228,5.28605985193424));
#11519=CARTESIAN_POINT('Ctrl Pts',(4.09579651057626,-3.10578912897284,5.26857587871268));
#11520=CARTESIAN_POINT('Ctrl Pts',(3.97951192525345,-3.25345329763332,5.25827001740642));
#11521=CARTESIAN_POINT('Ctrl Pts',(3.70964632072762,-3.55996883882456,5.23587783364701));
#11522=CARTESIAN_POINT('Ctrl Pts',(3.55337336087219,-3.71596490313294,5.22382144489708));
#11523=CARTESIAN_POINT('Ctrl Pts',(3.16402459396092,-4.05753244874945,5.19572662495801));
#11524=CARTESIAN_POINT('Ctrl Pts',(2.92388723522484,-4.23385267815995,5.17983238770126));
#11525=CARTESIAN_POINT('Ctrl Pts',(2.54528540766308,-4.46418869564088,5.15605843637834));
#11526=CARTESIAN_POINT('Ctrl Pts',(2.41755766957114,-4.53463032937321,5.14822630160392));
#11527=CARTESIAN_POINT('Ctrl Pts',(2.10397938392896,-4.69054934057154,5.12921744965009));
#11528=CARTESIAN_POINT('Ctrl Pts',(1.91568358977597,-4.77054890723372,5.11799409864902));
#11529=CARTESIAN_POINT('Ctrl Pts',(1.51216057300273,-4.91423650237626,5.09451198629455));
#11530=CARTESIAN_POINT('Ctrl Pts',(1.29650486924802,-4.97548278363567,5.08228449711849));
#11531=CARTESIAN_POINT('Ctrl Pts',(0.83651342401759,-5.07417114992291,5.05679515098435));
#11532=CARTESIAN_POINT('Ctrl Pts',(0.592076705526503,-5.10846510642551,
5.04358885557984));
#11533=CARTESIAN_POINT('Ctrl Pts',(0.173335422487548,-5.1367447373362,5.02108693358169));
#11534=CARTESIAN_POINT('Ctrl Pts',(7.31257870932242E-5,-5.13966822455429,
5.01180611869767));
#11535=CARTESIAN_POINT('Ctrl Pts',(-0.403813977630477,-5.12605790564199,
4.9898895015897));
#11536=CARTESIAN_POINT('Ctrl Pts',(-0.633836265327348,-5.10272325256985,
4.97719683718441));
#11537=CARTESIAN_POINT('Ctrl Pts',(-1.01563570440475,-5.03777024302909,
4.95597468649871));
#11538=CARTESIAN_POINT('Ctrl Pts',(-1.16849236970092,-5.00452512410979,
4.94743231178558));
#11539=CARTESIAN_POINT('Ctrl Pts',(-1.49044311109576,-4.91894612871971,
4.92932428038163));
#11540=CARTESIAN_POINT('Ctrl Pts',(-1.65883428994811,-4.86474279428754,
4.91978387849841));
#11541=CARTESIAN_POINT('Ctrl Pts',(-2.04932212205834,-4.7164101820224,4.8973300927706));
#11542=CARTESIAN_POINT('Ctrl Pts',(-2.26824587812907,-4.61511697808785,
4.88448311157));
#11543=CARTESIAN_POINT('Ctrl Pts',(-2.51600913742638,-4.47857793172112,
4.86922614022122));
#11544=CARTESIAN_POINT('Ctrl Pts',(-2.55251948563139,-4.45787017510926,
4.86695819402372));
#11545=CARTESIAN_POINT('Ctrl Pts',(-2.6955856090148,-4.37439279926031,4.8579837487011));
#11546=CARTESIAN_POINT('Ctrl Pts',(-2.80011183965857,-4.30823241737501,
4.85122853323049));
#11547=CARTESIAN_POINT('Ctrl Pts',(-3.06787887433788,-4.1248836774479,4.83345404965342));
#11548=CARTESIAN_POINT('Ctrl Pts',(-3.22681415472045,-4.00177681714965,
4.82242681106416));
#11549=CARTESIAN_POINT('Ctrl Pts',(-3.43719081487231,-3.81812334439494,
4.80717991422066));
#11550=CARTESIAN_POINT('Ctrl Pts',(-3.49506181699057,-3.76522106227782,
4.80290980517107));
#11551=CARTESIAN_POINT('Ctrl Pts',(-3.68310624358796,-3.58524943597255,
4.78876912574235));
#11552=CARTESIAN_POINT('Ctrl Pts',(-3.80774178924914,-3.45259173071376,
4.77896144642471));
#11553=CARTESIAN_POINT('Ctrl Pts',(-4.07586696421642,-3.13498779893074,
4.75663172151737));
#11554=CARTESIAN_POINT('Ctrl Pts',(-4.2142848997596,-2.94629267526063,4.74416361301676));
#11555=CARTESIAN_POINT('Ctrl Pts',(-4.36111019268017,-2.7145108210406,4.7293575864247));
#11556=CARTESIAN_POINT('Ctrl Pts',(-4.38244282748342,-2.67993394120567,
4.7271609838702));
#11557=CARTESIAN_POINT('Ctrl Pts',(-4.52411871659907,-2.44408331484917,
4.71224489691283));
#11558=CARTESIAN_POINT('Ctrl Pts',(-4.63096519517049,-2.23502836797372,
4.6993555257995));
#11559=CARTESIAN_POINT('Ctrl Pts',(-4.78454635710325,-1.87582081026763,
4.67794880073465));
#11560=CARTESIAN_POINT('Ctrl Pts',(-4.83935972053827,-1.72950463456054,
4.66941687705839));
#11561=CARTESIAN_POINT('Ctrl Pts',(-4.94194684680734,-1.41235545454078,
4.65129897979436));
#11562=CARTESIAN_POINT('Ctrl Pts',(-4.98771496044528,-1.24108340528471,
4.64173870813363));
#11563=CARTESIAN_POINT('Ctrl Pts',(-5.07794139622615,-0.816516849869994,
4.61840797605637));
#11564=CARTESIAN_POINT('Ctrl Pts',(-5.11241548553482,-0.561598795219459,
4.6047210912281));
#11565=CARTESIAN_POINT('Ctrl Pts',(-5.1337232019056,-0.203580757021962,
4.5853456424715));
#11566=CARTESIAN_POINT('Ctrl Pts',(-5.13674886148609,-0.101829509366764,
4.57981171115969));
#11567=CARTESIAN_POINT('Ctrl Pts',(-5.13675161298497,0.144194971788234,
4.56637234854805));
#11568=CARTESIAN_POINT('Ctrl Pts',(-5.13067679167021,0.288382805314253,
4.55845572529731));
#11569=CARTESIAN_POINT('Ctrl Pts',(-5.1010468084383,0.639353262164002,4.53914770184875));
#11570=CARTESIAN_POINT('Ctrl Pts',(-5.07098266694131,0.845333617713159,
4.52778891312207));
#11571=CARTESIAN_POINT('Ctrl Pts',(-4.98278422769968,1.2681536796937,4.50436622563596));
#11572=CARTESIAN_POINT('Ctrl Pts',(-4.92276642765659,1.48415835872673,4.49234165092297));
#11573=CARTESIAN_POINT('Ctrl Pts',(-4.78137394854056,1.88850291919869,4.46937314064419));
#11574=CARTESIAN_POINT('Ctrl Pts',(-4.70244963657659,2.0772444369788,4.45844430968834));
#11575=CARTESIAN_POINT('Ctrl Pts',(-4.54832674288316,2.3916897379459,4.43946377574975));
#11576=CARTESIAN_POINT('Ctrl Pts',(-4.47861778415142,2.51980893655661,4.43148739053182));
#11577=CARTESIAN_POINT('Ctrl Pts',(-4.36751796376614,2.70478953924705,4.41965977358021));
#11578=CARTESIAN_POINT('Ctrl Pts',(-4.33026961532294,2.76402933066338,4.41582199283889));
#11579=CARTESIAN_POINT('Ctrl Pts',(-4.29183634723918,2.82247078479419,4.41198748894216));
#11580=CARTESIAN_POINT('Origin',(0.,0.,0.));
#11581=CARTESIAN_POINT('',(-4.29199677360937,2.82257643420045,2.66202500160396));
#11582=CARTESIAN_POINT('',(-4.29183621895492,2.82247097986264,3.13909688836532));
#11583=CARTESIAN_POINT('',(-4.29183622825304,2.82247096572397,0.));
#11584=CARTESIAN_POINT('',(-5.13675004007553,-0.000129368701075719,3.30088737635801));
#11585=CARTESIAN_POINT('Ctrl Pts',(-4.29183621895492,2.82247097986264,3.13909688836532));
#11586=CARTESIAN_POINT('Ctrl Pts',(-4.31434163625608,2.78824934719221,3.14129950131095));
#11587=CARTESIAN_POINT('Ctrl Pts',(-4.33643920649416,2.75375631830031,3.14350002919566));
#11588=CARTESIAN_POINT('Ctrl Pts',(-4.47026145774089,2.53926049515073,3.15707221045047));
#11589=CARTESIAN_POINT('Ctrl Pts',(-4.57117114657727,2.352758786316,3.16838340061208));
#11590=CARTESIAN_POINT('Ctrl Pts',(-4.69788620924262,2.07943778774776,3.18463611438416));
#11591=CARTESIAN_POINT('Ctrl Pts',(-4.73337101716958,1.99734691669373,3.18948360463754));
#11592=CARTESIAN_POINT('Ctrl Pts',(-4.89764401713157,1.58831497354132,3.21350853176904));
#11593=CARTESIAN_POINT('Ctrl Pts',(-4.99479460385032,1.24967860481255,3.23285629740859));
#11594=CARTESIAN_POINT('Ctrl Pts',(-5.07504813350195,0.800661998792021,
3.25763833275876));
#11595=CARTESIAN_POINT('Ctrl Pts',(-5.0903199759671,0.697005156173732,3.26330725016343));
#11596=CARTESIAN_POINT('Ctrl Pts',(-5.12528966797252,0.396087887183829,
3.27965022342625));
#11597=CARTESIAN_POINT('Ctrl Pts',(-5.13675498680471,0.198063051843214,
3.29025921997661));
#11598=CARTESIAN_POINT('Ctrl Pts',(-5.13674999837291,-0.00012929019744156,
3.3008872998628));
#11599=CARTESIAN_POINT('Ctrl Pts',(-5.13674999837083,-0.000129372565223704,
3.30088730427978));
#11600=CARTESIAN_POINT('Ctrl Pts',(-5.13674612579616,-0.153890318034086,
3.3091327470438));
#11601=CARTESIAN_POINT('Ctrl Pts',(-5.12983834509799,-0.307571136377627,
3.31738214574149));
#11602=CARTESIAN_POINT('Ctrl Pts',(-5.10272874859786,-0.608616870674754,
3.3337678624906));
#11603=CARTESIAN_POINT('Ctrl Pts',(-5.08300150008219,-0.755876525193646,
3.34189484704342));
#11604=CARTESIAN_POINT('Ctrl Pts',(-5.00935481136442,-1.16873260684651,
3.36488401408925));
#11605=CARTESIAN_POINT('Ctrl Pts',(-4.94076786556144,-1.43121980420412,
3.37972203588897));
#11606=CARTESIAN_POINT('Ctrl Pts',(-4.78716696880529,-1.87295550571598,
3.40509359150357));
#11607=CARTESIAN_POINT('Ctrl Pts',(-4.71190277537752,-2.05497067164751,
3.41568078862056));
#11608=CARTESIAN_POINT('Ctrl Pts',(-4.55526944016961,-2.37960048042415,
3.43502067681698));
#11609=CARTESIAN_POINT('Ctrl Pts',(-4.47715742144368,-2.52349736779438,
3.44377263470832));
#11610=CARTESIAN_POINT('Ctrl Pts',(-4.35145585254996,-2.7307949740682,3.45681705808139));
#11611=CARTESIAN_POINT('Ctrl Pts',(-4.30905599440955,-2.79722100846318,
3.4610678026599));
#11612=CARTESIAN_POINT('Ctrl Pts',(-4.16534636182157,-3.01133857811476,
3.47505487145739));
#11613=CARTESIAN_POINT('Ctrl Pts',(-4.05784101596219,-3.15470994959003,
3.48487359093311));
#11614=CARTESIAN_POINT('Ctrl Pts',(-3.86868100961065,-3.38126898125076,
3.50105814060987));
#11615=CARTESIAN_POINT('Ctrl Pts',(-3.79129258578506,-3.46781970266228,
3.50741994673028));
#11616=CARTESIAN_POINT('Ctrl Pts',(-3.65506526521694,-3.61015954435536,
3.51818893400671));
#11617=CARTESIAN_POINT('Ctrl Pts',(-3.59771693372384,-3.66731333308679,
3.5226038915113));
#11618=CARTESIAN_POINT('Ctrl Pts',(-3.41412528901304,-3.84182932458607,
3.53638211105508));
#11619=CARTESIAN_POINT('Ctrl Pts',(-3.28331062935476,-3.95421006601779,
3.54569255021215));
#11620=CARTESIAN_POINT('Ctrl Pts',(-2.90644726189053,-4.24634830595016,
3.57134267597798));
#11621=CARTESIAN_POINT('Ctrl Pts',(-2.64969765551798,-4.41112280617052,
3.58752328436325));
#11622=CARTESIAN_POINT('Ctrl Pts',(-2.21216641867224,-4.63986366384214,
3.61429693512724));
#11623=CARTESIAN_POINT('Ctrl Pts',(-2.03974086582732,-4.7182062431308,3.62467758210589));
#11624=CARTESIAN_POINT('Ctrl Pts',(-1.65695218080982,-4.8672152455183,3.6472018832576));
#11625=CARTESIAN_POINT('Ctrl Pts',(-1.44552884790294,-4.93413867833424,
3.65931690279207));
#11626=CARTESIAN_POINT('Ctrl Pts',(-0.915591744015469,-5.06488482932643,
3.68894017476201));
#11627=CARTESIAN_POINT('Ctrl Pts',(-0.594089770907524,-5.11257544983285,
3.70624874556336));
#11628=CARTESIAN_POINT('Ctrl Pts',(-0.139719207230433,-5.13651263367917,
3.73067366122826));
#11629=CARTESIAN_POINT('Ctrl Pts',(-0.00898646934228279,-5.13840461067615,
3.73770509894011));
#11630=CARTESIAN_POINT('Ctrl Pts',(0.303919311190788,-5.1309906513171,3.7547031982634));
#11631=CARTESIAN_POINT('Ctrl Pts',(0.485801915032334,-5.11697439419366,
3.76470410231091));
#11632=CARTESIAN_POINT('Ctrl Pts',(0.884280653854546,-5.06482637645206,
3.78674019785601));
#11633=CARTESIAN_POINT('Ctrl Pts',(1.099962664156,-5.0224002196701,3.79874631966172));
#11634=CARTESIAN_POINT('Ctrl Pts',(1.61867843600075,-4.88533747872523,3.82785970059415));
#11635=CARTESIAN_POINT('Ctrl Pts',(1.9169385478368,-4.77619017812944,3.84478178084446));
#11636=CARTESIAN_POINT('Ctrl Pts',(2.32470922134776,-4.58257676006919,3.86900875663399));
#11637=CARTESIAN_POINT('Ctrl Pts',(2.44386770315813,-4.52015403342131,3.87624001468175));
#11638=CARTESIAN_POINT('Ctrl Pts',(2.72364881707301,-4.35928680110357,3.89376417740104));
#11639=CARTESIAN_POINT('Ctrl Pts',(2.88157436339059,-4.25654458778638,3.90409488791843));
#11640=CARTESIAN_POINT('Ctrl Pts',(3.21131227268516,-4.01524865699555,3.92649850801113));
#11641=CARTESIAN_POINT('Ctrl Pts',(3.38057046033108,-3.87382176793148,3.93854158899194));
#11642=CARTESIAN_POINT('Ctrl Pts',(3.75532550756194,-3.51736530069845,3.96659644484515));
#11643=CARTESIAN_POINT('Ctrl Pts',(3.9522858323587,-3.29450586352294,3.98246477019735));
#11644=CARTESIAN_POINT('Ctrl Pts',(4.21581890141645,-2.93843845624901,4.00622876913822));
#11645=CARTESIAN_POINT('Ctrl Pts',(4.29769016924388,-2.81734051255778,4.0140774425482));
#11646=CARTESIAN_POINT('Ctrl Pts',(4.4816796101353,-2.51847425437161,4.03312725249025));
#11647=CARTESIAN_POINT('Ctrl Pts',(4.57853956172384,-2.33776352584395,4.04437526366578));
#11648=CARTESIAN_POINT('Ctrl Pts',(4.75802507450122,-1.94869372409275,4.06786448074228));
#11649=CARTESIAN_POINT('Ctrl Pts',(4.83834280068921,-1.73972773045446,4.08007465942468));
#11650=CARTESIAN_POINT('Ctrl Pts',(4.97947792775408,-1.28615536694663,4.10581117586804));
#11651=CARTESIAN_POINT('Ctrl Pts',(5.03644746675353,-1.04095918568242,4.11927458788016));
#11652=CARTESIAN_POINT('Ctrl Pts',(5.10135403330102,-0.625332205992982,
4.1418294226555));
#11653=CARTESIAN_POINT('Ctrl Pts',(5.11918857432193,-0.456902156318874,
4.15090378545258));
#11654=CARTESIAN_POINT('Ctrl Pts',(5.13890002952896,-0.105764388778069,
4.16997982012417));
#11655=CARTESIAN_POINT('Ctrl Pts',(5.13941451232527,0.0767872595261164,
4.17998369442522));
#11656=CARTESIAN_POINT('Ctrl Pts',(5.11883901954797,0.484380370928735,4.20236278399278));
#11657=CARTESIAN_POINT('Ctrl Pts',(5.09261737623013,0.708794066694097,4.21470836249437));
#11658=CARTESIAN_POINT('Ctrl Pts',(4.99242249082055,1.2526056342636,4.24472100931902));
#11659=CARTESIAN_POINT('Ctrl Pts',(4.90250149117385,1.56805169444472,4.26218541645775));
#11660=CARTESIAN_POINT('Ctrl Pts',(4.73605830076253,1.99315295393288,4.2866941209861));
#11661=CARTESIAN_POINT('Ctrl Pts',(4.68440939389031,2.11168529819525,4.29364875186226));
#11662=CARTESIAN_POINT('Ctrl Pts',(4.55033203215963,2.39019358739317,4.31043659600053));
#11663=CARTESIAN_POINT('Ctrl Pts',(4.46386291414731,2.54803323190023,4.32030254736569));
#11664=CARTESIAN_POINT('Ctrl Pts',(4.2529073903596,2.88928594904022,4.34230145153023));
#11665=CARTESIAN_POINT('Ctrl Pts',(4.1244693497047,3.06984536201229,4.35440475484275));
#11666=CARTESIAN_POINT('Ctrl Pts',(3.7844839417774,3.48778272489964,4.38364002470495));
#11667=CARTESIAN_POINT('Ctrl Pts',(3.56179286452425,3.71491352300689,4.40058732566539));
#11668=CARTESIAN_POINT('Ctrl Pts',(3.21713929916307,4.00677292704103,4.42482678011335));
#11669=CARTESIAN_POINT('Ctrl Pts',(3.11135622352853,4.0894591484327,4.43204458430779));
#11670=CARTESIAN_POINT('Ctrl Pts',(2.85001470505729,4.27772310499848,4.4495341424321));
#11671=CARTESIAN_POINT('Ctrl Pts',(2.69166398992563,4.37909146968617,4.45984347662887));
#11672=CARTESIAN_POINT('Ctrl Pts',(2.33613725497451,4.58009845287954,4.48223724998594));
#11673=CARTESIAN_POINT('Ctrl Pts',(2.13736082214875,4.67616630069395,4.49429177003673));
#11674=CARTESIAN_POINT('Ctrl Pts',(1.6575879654358,4.87103511302511,4.52238105932679));
#11675=CARTESIAN_POINT('Ctrl Pts',(1.37295873461636,4.95878706027175,4.53827173640728));
#11676=CARTESIAN_POINT('Ctrl Pts',(0.939768756184492,5.05215851226198,4.56204430790658));
#11677=CARTESIAN_POINT('Ctrl Pts',(0.795957974736394,5.07680220634383,4.56987870270247));
#11678=CARTESIAN_POINT('Ctrl Pts',(0.448477893813733,5.12121813481024,4.58889319764682));
#11679=CARTESIAN_POINT('Ctrl Pts',(0.24429572456553,5.13500976941002,4.60011996561718));
#11680=CARTESIAN_POINT('Ctrl Pts',(-0.184051653057268,5.13833197426969,
4.62360305296982));
#11681=CARTESIAN_POINT('Ctrl Pts',(-0.407820268856465,5.12542846225274,
4.63582813403276));
#11682=CARTESIAN_POINT('Ctrl Pts',(-0.877026503496012,5.06744131284838,
4.66144299802282));
#11683=CARTESIAN_POINT('Ctrl Pts',(-1.12147490047326,5.01900727455947,4.67477377875648));
#11684=CARTESIAN_POINT('Ctrl Pts',(-1.52637072166629,4.90771296889318,4.69728779832826));
#11685=CARTESIAN_POINT('Ctrl Pts',(-1.68892084205195,4.85417329852926,4.70645525547616));
#11686=CARTESIAN_POINT('Ctrl Pts',(-2.06368333503849,4.70962916299031,4.72823993300734));
#11687=CARTESIAN_POINT('Ctrl Pts',(-2.27303626942172,4.61223368350821,4.74091588948176));
#11688=CARTESIAN_POINT('Ctrl Pts',(-2.61214544964475,4.42575936469761,4.76212237131582));
#11689=CARTESIAN_POINT('Ctrl Pts',(-2.74564892399965,4.34419877776501,4.77066563807934));
#11690=CARTESIAN_POINT('Ctrl Pts',(-3.02169087439151,4.15774272360441,4.78877284425884));
#11691=CARTESIAN_POINT('Ctrl Pts',(-3.16295473596736,4.0513157868866,4.79831156670103));
#11692=CARTESIAN_POINT('Ctrl Pts',(-3.48314291991241,3.78311500025063,4.82076344299472));
#11693=CARTESIAN_POINT('Ctrl Pts',(-3.65671817672521,3.6156125077955,4.83361016214211));
#11694=CARTESIAN_POINT('Ctrl Pts',(-3.84598987714552,3.40533786809132,4.84886791552904));
#11695=CARTESIAN_POINT('Ctrl Pts',(-3.87370096498165,3.37378199019494,4.85113703712899));
#11696=CARTESIAN_POINT('Ctrl Pts',(-3.98090387010537,3.24864296469522,4.86006480280909));
#11697=CARTESIAN_POINT('Ctrl Pts',(-4.05741527366864,3.15256352653649,4.86677141894919));
#11698=CARTESIAN_POINT('Ctrl Pts',(-4.18633789524806,2.97819171682413,4.87864837273494));
#11699=CARTESIAN_POINT('Ctrl Pts',(-4.24016636135774,2.90103992224406,4.8838080587719));
#11700=CARTESIAN_POINT('Ctrl Pts',(-4.29183618112783,2.82247103738233,4.88896334675683));
#11701=CARTESIAN_POINT('',(-5.13651484023392,0.000115948992882031,2.82404150530312));
#11702=CARTESIAN_POINT('Ctrl Pts',(-4.29183634723918,2.82247078479419,4.41198748894216));
#11703=CARTESIAN_POINT('Ctrl Pts',(-4.16698587373161,3.01231785178831,4.39953110282041));
#11704=CARTESIAN_POINT('Ctrl Pts',(-4.02963071635437,3.19374075290447,4.38712197081976));
#11705=CARTESIAN_POINT('Ctrl Pts',(-3.73612956550945,3.53216556002768,4.36285766398529));
#11706=CARTESIAN_POINT('Ctrl Pts',(-3.58102114042954,3.68932890567501,4.35102484059281));
#11707=CARTESIAN_POINT('Ctrl Pts',(-3.27604092772345,3.9609375593332,4.32912928924372));
#11708=CARTESIAN_POINT('Ctrl Pts',(-3.12905114971264,4.07805185788519,4.31907839854511));
#11709=CARTESIAN_POINT('Ctrl Pts',(-2.86662554369391,4.26458197742617,4.30163415571333));
#11710=CARTESIAN_POINT('Ctrl Pts',(-2.75426752523295,4.33799611961743,4.29430067500792));
#11711=CARTESIAN_POINT('Ctrl Pts',(-2.36678203900346,4.57004881472384,4.26955374984683));
#11712=CARTESIAN_POINT('Ctrl Pts',(-2.0798511784439,4.70757177577128,4.25215848700385));
#11713=CARTESIAN_POINT('Ctrl Pts',(-1.70962682491867,4.84451661825589,4.230785323076));
#11714=CARTESIAN_POINT('Ctrl Pts',(-1.63659713314603,4.86967300144542,4.22661547558092));
#11715=CARTESIAN_POINT('Ctrl Pts',(-1.38834792646372,4.94897130409852,4.21257524180766));
#11716=CARTESIAN_POINT('Ctrl Pts',(-1.21080523780386,4.99537568940815,4.20276111010223));
#11717=CARTESIAN_POINT('Ctrl Pts',(-0.879696229489418,5.06322427581663,
4.18463390673299));
#11718=CARTESIAN_POINT('Ctrl Pts',(-0.726909371012189,5.08740668869004,
4.17633464143379));
#11719=CARTESIAN_POINT('Ctrl Pts',(-0.413174559980931,5.12263998239836,
4.15920153610614));
#11720=CARTESIAN_POINT('Ctrl Pts',(-0.252326397011973,5.13307739963098,
4.1503748936816));
#11721=CARTESIAN_POINT('Ctrl Pts',(0.159466251844732,5.1403942378555,4.12779133029774));
#11722=CARTESIAN_POINT('Ctrl Pts',(0.410184079607603,5.12648380152769,4.11406728356203));
#11723=CARTESIAN_POINT('Ctrl Pts',(0.865980866247116,5.0675323422528,4.08913561064054));
#11724=CARTESIAN_POINT('Ctrl Pts',(1.07125366947234,5.02814330520748,4.07790960016148));
#11725=CARTESIAN_POINT('Ctrl Pts',(1.49674222504323,4.91925150846555,4.0543512741899));
#11726=CARTESIAN_POINT('Ctrl Pts',(1.71582365701268,4.84718657241992,4.04205190831842));
#11727=CARTESIAN_POINT('Ctrl Pts',(1.96623131618516,4.74570553105891,4.02739561684172));
#11728=CARTESIAN_POINT('Ctrl Pts',(2.0029648951508,4.7303190338737,4.02522967903795));
#11729=CARTESIAN_POINT('Ctrl Pts',(2.25290352949564,4.62219452969925,4.01038947628906));
#11730=CARTESIAN_POINT('Ctrl Pts',(2.45977724820779,4.51550131852102,3.99760448772146));
#11731=CARTESIAN_POINT('Ctrl Pts',(2.81626101730516,4.29985809873201,3.97480838910817));
#11732=CARTESIAN_POINT('Ctrl Pts',(2.96857560114251,4.19614907219953,3.96478664594098));
#11733=CARTESIAN_POINT('Ctrl Pts',(3.25390099252848,3.97854826481852,3.94537614251492));
#11734=CARTESIAN_POINT('Ctrl Pts',(3.38731432460225,3.86559452496691,3.93599324912956));
#11735=CARTESIAN_POINT('Ctrl Pts',(3.67449138419474,3.59615281646616,3.91487387141684));
#11736=CARTESIAN_POINT('Ctrl Pts',(3.82451057584409,3.43617770224084,3.90316984683769));
#11737=CARTESIAN_POINT('Ctrl Pts',(4.0637518660067,3.14591651354651,3.88277721021179));
#11738=CARTESIAN_POINT('Ctrl Pts',(4.15803636699966,3.02019896117357,3.87417745955817));
#11739=CARTESIAN_POINT('Ctrl Pts',(4.3997437315395,2.66509164186776,3.8506260579924));
#11740=CARTESIAN_POINT('Ctrl Pts',(4.53491116777309,2.42797140819965,3.83570852024841));
#11741=CARTESIAN_POINT('Ctrl Pts',(4.75000089237087,1.96937922115244,3.80824994901112));
#11742=CARTESIAN_POINT('Ctrl Pts',(4.83477841364186,1.75096650678446,3.79569685530856));
#11743=CARTESIAN_POINT('Ctrl Pts',(4.95958572779056,1.35025425526063,3.77319528924216));
#11744=CARTESIAN_POINT('Ctrl Pts',(5.00514791860923,1.17011498450273,3.76325692924003));
#11745=CARTESIAN_POINT('Ctrl Pts',(5.06639688980398,0.857588889998009,3.74600288246298));
#11746=CARTESIAN_POINT('Ctrl Pts',(5.08687320653975,0.726330247355653,3.73874509430522));
#11747=CARTESIAN_POINT('Ctrl Pts',(5.13928545762581,0.276453311367826,3.71393041820706));
#11748=CARTESIAN_POINT('Ctrl Pts',(5.14652589683625,-0.0442993161981663,
3.69638975855686));
#11749=CARTESIAN_POINT('Ctrl Pts',(5.108016425025,-0.58691963264991,3.66693741023549));
#11750=CARTESIAN_POINT('Ctrl Pts',(5.07759223039183,-0.808928934359862,
3.65493683317251));
#11751=CARTESIAN_POINT('Ctrl Pts',(4.99516043005286,-1.21239359879457,3.63285918260659));
#11752=CARTESIAN_POINT('Ctrl Pts',(4.94745981875735,-1.39433307262257,3.62279567306552));
#11753=CARTESIAN_POINT('Ctrl Pts',(4.83782946207367,-1.73508183596097,3.60337688120331));
#11754=CARTESIAN_POINT('Ctrl Pts',(4.77775958408615,-1.89423194031333,3.59405930115639));
#11755=CARTESIAN_POINT('Ctrl Pts',(4.61039790601261,-2.27872810951186,3.57106458514552));
#11756=CARTESIAN_POINT('Ctrl Pts',(4.49436913243882,-2.49980429798838,3.5574236828366));
#11757=CARTESIAN_POINT('Ctrl Pts',(4.2445622392266,-2.90172598993572,3.53176094077151));
#11758=CARTESIAN_POINT('Ctrl Pts',(4.11407563818438,-3.0839433985168,3.51973991424205));
#11759=CARTESIAN_POINT('Ctrl Pts',(3.8424509966675,-3.41519978376224,3.49676985460789));
#11760=CARTESIAN_POINT('Ctrl Pts',(3.70346093812589,-3.56544432361029,3.48583597099365));
#11761=CARTESIAN_POINT('Ctrl Pts',(3.45062776303413,-3.80797106325528,3.4668465739468));
#11762=CARTESIAN_POINT('Ctrl Pts',(3.34111544225883,-3.90441052517542,3.4588664696661));
#11763=CARTESIAN_POINT('Ctrl Pts',(2.99640171948637,-4.18283883486137,3.43457788345979));
#11764=CARTESIAN_POINT('Ctrl Pts',(2.74936951454945,-4.34919983472328,3.41830041235499));
#11765=CARTESIAN_POINT('Ctrl Pts',(2.29643071437254,-4.60013486452377,3.39025324662284));
#11766=CARTESIAN_POINT('Ctrl Pts',(2.09684128391969,-4.69447483070205,3.37842315012932));
#11767=CARTESIAN_POINT('Ctrl Pts',(1.71711198229436,-4.84489768070246,3.35652514904728));
#11768=CARTESIAN_POINT('Ctrl Pts',(1.53875640268628,-4.90446055851283,3.34646910037956));
#11769=CARTESIAN_POINT('Ctrl Pts',(1.22808443090893,-4.98959188421171,3.32901608696968));
#11770=CARTESIAN_POINT('Ctrl Pts',(1.09728773392296,-5.01997775425295,3.32167908404949));
#11771=CARTESIAN_POINT('Ctrl Pts',(0.653736807702905,-5.10485600200475,
3.29693522931891));
#11772=CARTESIAN_POINT('Ctrl Pts',(0.337151974305867,-5.13549069809148,
3.27954664739659));
#11773=CARTESIAN_POINT('Ctrl Pts',(-0.199632914229041,-5.13755619757714,
3.25048221337806));
#11774=CARTESIAN_POINT('Ctrl Pts',(-0.418862162275425,-5.12434326013654,
3.23871619197176));
#11775=CARTESIAN_POINT('Ctrl Pts',(-0.817528766906801,-5.07455433896842,
3.2171764094075));
#11776=CARTESIAN_POINT('Ctrl Pts',(-0.997146294888052,-5.04233596897738,
3.20741403073825));
#11777=CARTESIAN_POINT('Ctrl Pts',(-1.30194277429408,-4.97073825333411,
3.19045290852861));
#11778=CARTESIAN_POINT('Ctrl Pts',(-1.42802884969813,-4.93599289859468,
3.18330897824713));
#11779=CARTESIAN_POINT('Ctrl Pts',(-1.86169327647025,-4.79848000757839,
3.15838573140533));
#11780=CARTESIAN_POINT('Ctrl Pts',(-2.16077584673093,-4.67144197549698,
3.14061949307602));
#11781=CARTESIAN_POINT('Ctrl Pts',(-2.64063244514378,-4.41161041848959,
3.11107762533365));
#11782=CARTESIAN_POINT('Ctrl Pts',(-2.82835650920064,-4.29367535017223,
3.09920402644515));
#11783=CARTESIAN_POINT('Ctrl Pts',(-3.16139176043437,-4.05310536390033,
3.07717800486347));
#11784=CARTESIAN_POINT('Ctrl Pts',(-3.30864704724423,-3.93381660329622,
3.06703937154162));
#11785=CARTESIAN_POINT('Ctrl Pts',(-3.57475728552765,-3.6927116017888,3.04755782221915));
#11786=CARTESIAN_POINT('Ctrl Pts',(-3.69481074735828,-3.57258737928862,
3.03825541100929));
#11787=CARTESIAN_POINT('Ctrl Pts',(-3.98081182979747,-3.2565525159005,3.01488278264972));
#11788=CARTESIAN_POINT('Ctrl Pts',(-4.13844413358835,-3.05373256130016,
3.00085247389584));
#11789=CARTESIAN_POINT('Ctrl Pts',(-4.36438680493656,-2.71320434173564,
2.97870184272605));
#11790=CARTESIAN_POINT('Ctrl Pts',(-4.44283307788045,-2.58274764502386,
2.97050522314688));
#11791=CARTESIAN_POINT('Ctrl Pts',(-4.64062278389246,-2.21807044518969,
2.94822104182528));
#11792=CARTESIAN_POINT('Ctrl Pts',(-4.74796938175079,-1.97787719972954,
2.93422696338568));
#11793=CARTESIAN_POINT('Ctrl Pts',(-4.8654627302989,-1.64950862658489,2.91533902401815));
#11794=CARTESIAN_POINT('Ctrl Pts',(-4.89241326820209,-1.56776852310285,
2.91065129160068));
#11795=CARTESIAN_POINT('Ctrl Pts',(-5.01082735890465,-1.17576598720495,
2.88827250409072));
#11796=CARTESIAN_POINT('Ctrl Pts',(-5.07490678563656,-0.857988966175358,
2.87049172435325));
#11797=CARTESIAN_POINT('Ctrl Pts',(-5.12738307900252,-0.358112429451637,
2.84319159551417));
#11798=CARTESIAN_POINT('Ctrl Pts',(-5.13675378971372,-0.179064674554883,
2.83353163990953));
#11799=CARTESIAN_POINT('Ctrl Pts',(-5.13674999885029,0.000108680878606257,
2.82390612103021));
#11800=CARTESIAN_POINT('Ctrl Pts',(-5.13651484023392,0.000115948992882031,
2.82404150530312));
#11801=CARTESIAN_POINT('Ctrl Pts',(-5.13674462019434,0.2777253544017,2.80899084758333));
#11802=CARTESIAN_POINT('Ctrl Pts',(-5.05737420441865,1.27372684428605,2.75498534635027));
#11803=CARTESIAN_POINT('Ctrl Pts',(-4.68610612556516,2.22198890685184,2.70097984511722));
#11804=CARTESIAN_POINT('Ctrl Pts',(-4.29199677360937,2.82257643420045,2.66202500160396));
#11805=CARTESIAN_POINT('Origin',(0.,0.,0.));
#11806=CARTESIAN_POINT('',(-4.29183622825303,2.82247096572397,0.912017191992546));
#11807=CARTESIAN_POINT('',(-4.29183622715607,2.82247096739201,1.38870419915418));
#11808=CARTESIAN_POINT('',(-4.29183622825304,2.82247096572397,0.));
#11809=CARTESIAN_POINT('',(3.87994761181451,-3.36633437021263,0.));
#11810=CARTESIAN_POINT('Ctrl Pts',(-4.29183622825303,2.82247096572397,0.912017191992546));
#11811=CARTESIAN_POINT('Ctrl Pts',(-4.21008100390854,2.94678757976597,0.903950966471187));
#11812=CARTESIAN_POINT('Ctrl Pts',(-4.12291891447378,3.06755243451359,0.895884740949828));
#11813=CARTESIAN_POINT('Ctrl Pts',(-4.03068457529414,3.18430250086042,0.887818515428468));
#11814=CARTESIAN_POINT('Ctrl Pts',(-3.93845155802828,3.30105089393108,0.879752405513235));
#11815=CARTESIAN_POINT('Ctrl Pts',(-3.84114664385558,3.41378435569289,0.871686295598001));
#11816=CARTESIAN_POINT('Ctrl Pts',(-3.73914516075628,3.52207240545859,0.863620185682768));
#11817=CARTESIAN_POINT('Ctrl Pts',(-3.63712168518292,3.63038380314095,0.855552336638772));
#11818=CARTESIAN_POINT('Ctrl Pts',(-3.53039984594936,3.73424763421122,0.847484487594775));
#11819=CARTESIAN_POINT('Ctrl Pts',(-3.41939267200455,3.83326940315204,0.839416638550779));
#11820=CARTESIAN_POINT('Ctrl Pts',(-3.39302187999351,3.85679295014912,0.837500045581558));
#11821=CARTESIAN_POINT('Ctrl Pts',(-3.36640940475421,3.88004340779256,0.835583452612338));
#11822=CARTESIAN_POINT('Ctrl Pts',(-3.33956107133174,3.90301581003019,0.833666859643117));
#11823=CARTESIAN_POINT('Ctrl Pts',(-3.22653862334114,3.99972189216443,0.825598648265736));
#11824=CARTESIAN_POINT('Ctrl Pts',(-3.10929183836299,4.09153327460306,0.817530436888356));
#11825=CARTESIAN_POINT('Ctrl Pts',(-2.9882666781965,4.17809320413995,0.809462225510975));
#11826=CARTESIAN_POINT('Ctrl Pts',(-2.86726598957703,4.2646356310734,0.801395645543243));
#11827=CARTESIAN_POINT('Ctrl Pts',(-2.74248871904446,4.34592853107688,0.793329065575511));
#11828=CARTESIAN_POINT('Ctrl Pts',(-2.61441152346859,4.42165726266234,0.785262485607779));
#11829=CARTESIAN_POINT('Ctrl Pts',(-2.4863297736047,4.49738868708047,0.777195618801096));
#11830=CARTESIAN_POINT('Ctrl Pts',(-2.35494814688641,4.56755537541207,0.769128751994412));
#11831=CARTESIAN_POINT('Ctrl Pts',(-2.22077020889626,4.63188733042794,0.761061885187729));
#11832=CARTESIAN_POINT('Ctrl Pts',(-2.08660042131369,4.69621537771008,0.752995508388966));
#11833=CARTESIAN_POINT('Ctrl Pts',(-1.94963496112967,4.75470925833884,0.744929131590202));
#11834=CARTESIAN_POINT('Ctrl Pts',(-1.81039978902733,4.8071460521176,0.736862754791439));
#11835=CARTESIAN_POINT('Ctrl Pts',(-1.6711299114841,4.85959591617177,0.728794367386024));
#11836=CARTESIAN_POINT('Ctrl Pts',(-1.52958950126482,4.90598555920214,0.720725979980609));
#11837=CARTESIAN_POINT('Ctrl Pts',(-1.38632283533957,4.9461408753407,0.712657592575194));
#11838=CARTESIAN_POINT('Ctrl Pts',(-1.2801670636738,4.9758946114498,0.706679189395441));
#11839=CARTESIAN_POINT('Ctrl Pts',(-1.17306391967465,5.00222651706419,0.700700786215688));
#11840=CARTESIAN_POINT('Ctrl Pts',(-1.06523962154578,5.02508359245784,0.694722383035935));
#11841=CARTESIAN_POINT('Ctrl Pts',(-0.919691791466988,5.0559374703242,0.686652368899518));
#11842=CARTESIAN_POINT('Ctrl Pts',(-0.772775968558962,5.0804692105179,0.678582354763101));
#11843=CARTESIAN_POINT('Ctrl Pts',(-0.625054704343801,5.0985789372214,0.670512340626684));
#11844=CARTESIAN_POINT('Ctrl Pts',(-0.477363046062251,5.11668503441787,
0.662443943862715));
#11845=CARTESIAN_POINT('Ctrl Pts',(-0.328866596591976,5.12837164570133,
0.654375547098746));
#11846=CARTESIAN_POINT('Ctrl Pts',(-0.180134706237769,5.13359056120652,
0.646307150334778));
#11847=CARTESIAN_POINT('Ctrl Pts',(-0.0313974666155599,5.1388096644144,
0.638238463384108));
#11848=CARTESIAN_POINT('Ctrl Pts',(0.11757490046023,5.13756059100852,0.630169776433437));
#11849=CARTESIAN_POINT('Ctrl Pts',(0.266210780156402,5.12984720854613,0.622101089482767));
#11850=CARTESIAN_POINT('Ctrl Pts',(0.414837591449361,5.12213429668385,0.614032894809647));
#11851=CARTESIAN_POINT('Ctrl Pts',(0.563127626181557,5.10795788272256,0.605964700136526));
#11852=CARTESIAN_POINT('Ctrl Pts',(0.710512129098562,5.08737388805893,0.597896505463406));
#11853=CARTESIAN_POINT('Ctrl Pts',(0.857932985422962,5.0667848162106,0.589826320714246));
#11854=CARTESIAN_POINT('Ctrl Pts',(1.0044475358245,5.0397850506676,0.581756135965086));
#11855=CARTESIAN_POINT('Ctrl Pts',(1.14949429669496,5.00648214062187,0.573685951215926));
#11856=CARTESIAN_POINT('Ctrl Pts',(1.25678237706487,4.98184866884977,0.567716602953532));
#11857=CARTESIAN_POINT('Ctrl Pts',(1.36326752836467,4.95376766217731,0.561747254691139));
#11858=CARTESIAN_POINT('Ctrl Pts',(1.46872680677471,4.92230049159551,0.555777906428746));
#11859=CARTESIAN_POINT('Ctrl Pts',(1.61116648069071,4.87979902956858,0.54771534396098));
#11860=CARTESIAN_POINT('Ctrl Pts',(1.751787269433,4.83110249295492,0.539652781493215));
#11861=CARTESIAN_POINT('Ctrl Pts',(1.89004827637476,4.77639174225406,0.531590219025449));
#11862=CARTESIAN_POINT('Ctrl Pts',(2.0282809272638,4.72169221222174,0.523529310114616));
#11863=CARTESIAN_POINT('Ctrl Pts',(2.16415445337024,4.66098105087857,0.515468401203782));
#11864=CARTESIAN_POINT('Ctrl Pts',(2.29714668271859,4.59448774952932,0.507407492292949));
#11865=CARTESIAN_POINT('Ctrl Pts',(2.43014400301256,4.52799190281495,0.499346274810335));
#11866=CARTESIAN_POINT('Ctrl Pts',(2.56025950722101,4.45571361820597,0.491285057327722));
#11867=CARTESIAN_POINT('Ctrl Pts',(2.68699393420941,4.37792920911495,0.483223839845109));
#11868=CARTESIAN_POINT('Ctrl Pts',(2.81372104560421,4.30014929003614,0.475163087686658));
#11869=CARTESIAN_POINT('Ctrl Pts',(2.93706718779034,4.21686405679972,0.467102335528207));
#11870=CARTESIAN_POINT('Ctrl Pts',(3.05656051392089,4.1283941656823,0.459041583369756));
#11871=CARTESIAN_POINT('Ctrl Pts',(3.17608499704292,4.03990120670215,0.450978729430441));
#11872=CARTESIAN_POINT('Ctrl Pts',(3.29175438943587,3.94622108570467,0.442915875491126));
#11873=CARTESIAN_POINT('Ctrl Pts',(3.40312793024007,3.84771631658571,0.434853021551811));
#11874=CARTESIAN_POINT('Ctrl Pts',(3.48609713485625,3.77433387506786,0.428846490975061));
#11875=CARTESIAN_POINT('Ctrl Pts',(3.56668289912837,3.69827477537264,0.42283996039831));
#11876=CARTESIAN_POINT('Ctrl Pts',(3.6447156174895,3.61970283726829,0.41683342982156));
#11877=CARTESIAN_POINT('Ctrl Pts',(3.74970717869758,3.51398576599388,0.408751755417004));
#11878=CARTESIAN_POINT('Ctrl Pts',(3.85011415322258,3.40367942648003,0.400670081012447));
#11879=CARTESIAN_POINT('Ctrl Pts',(3.94554677348586,3.28920373658053,0.392588406607891));
#11880=CARTESIAN_POINT('Ctrl Pts',(4.04096069636049,3.17475047503371,0.384508315584434));
#11881=CARTESIAN_POINT('Ctrl Pts',(4.13140199903371,3.0561297452835,0.376428224560978));
#11882=CARTESIAN_POINT('Ctrl Pts',(4.2165206596561,2.93379516824084,0.368348133537521));
#11883=CARTESIAN_POINT('Ctrl Pts',(4.30164168937171,2.81145718628068,0.360267817622264));
#11884=CARTESIAN_POINT('Ctrl Pts',(4.38143958971418,2.68540541788936,0.352187501707008));
#11885=CARTESIAN_POINT('Ctrl Pts',(4.45560688104378,2.55612360501118,0.344107185791751));
#11886=CARTESIAN_POINT('Ctrl Pts',(4.52976906939097,2.42685068719719,0.336027425831946));
#11887=CARTESIAN_POINT('Ctrl Pts',(4.59830126053746,2.29434845491385,0.327947665872142));
#11888=CARTESIAN_POINT('Ctrl Pts',(4.6609412589197,2.15912647693462,0.319867905912338));
#11889=CARTESIAN_POINT('Ctrl Pts',(4.7235950620254,2.02387469847547,0.311786365319474));
#11890=CARTESIAN_POINT('Ctrl Pts',(4.78035393865719,1.88590227475489,0.30370482472661));
#11891=CARTESIAN_POINT('Ctrl Pts',(4.83100301207731,1.74574066224051,0.295623284133747));
#11892=CARTESIAN_POINT('Ctrl Pts',(4.86805153512688,1.64321596867247,0.289711840493955));
#11893=CARTESIAN_POINT('Ctrl Pts',(4.90183195686734,1.53952040512254,0.283800396854164));
#11894=CARTESIAN_POINT('Ctrl Pts',(4.9322768395638,1.43486784771369,0.277888953214373));
#11895=CARTESIAN_POINT('Ctrl Pts',(4.97370082733191,1.29247523936544,0.269845710891254));
#11896=CARTESIAN_POINT('Ctrl Pts',(5.00896290811795,1.14825843281626,0.261802468568135));
#11897=CARTESIAN_POINT('Ctrl Pts',(5.03792200991058,1.0027673631299,0.253759226245016));
#11898=CARTESIAN_POINT('Ctrl Pts',(5.06687513239429,0.857306333603579,0.245717644644352));
#11899=CARTESIAN_POINT('Ctrl Pts',(5.08952780654059,0.71057189423708,0.237676063043689));
#11900=CARTESIAN_POINT('Ctrl Pts',(5.10578996746797,0.563124649259317,0.229634481443026));
#11901=CARTESIAN_POINT('Ctrl Pts',(5.12205310316367,0.415668566163129,0.221592417822841));
#11902=CARTESIAN_POINT('Ctrl Pts',(5.13192491885463,0.267499924669364,0.213550354202656));
#11903=CARTESIAN_POINT('Ctrl Pts',(5.13536711260807,0.119185490909914,0.205508290582471));
#11904=CARTESIAN_POINT('Ctrl Pts',(5.13880916577307,-0.0291228852895836,
0.197466555421771));
#11905=CARTESIAN_POINT('Ctrl Pts',(5.13582211635772,-0.177576706738936,
0.189424820261071));
#11906=CARTESIAN_POINT('Ctrl Pts',(5.12641978813453,-0.325608228278663,
0.181383085100371));
#11907=CARTESIAN_POINT('Ctrl Pts',(5.1170145447799,-0.473685646040024,0.17333885665138));
#11908=CARTESIAN_POINT('Ctrl Pts',(5.10119006912052,-0.621340167588099,
0.16529462820239));
#11909=CARTESIAN_POINT('Ctrl Pts',(5.07901221185679,-0.76800749625874,0.1572503997534));
#11910=CARTESIAN_POINT('Ctrl Pts',(5.06218912960214,-0.879262452269773,
0.151148425371328));
#11911=CARTESIAN_POINT('Ctrl Pts',(5.04171136380057,-0.989949420781112,
0.145046450989256));
#11912=CARTESIAN_POINT('Ctrl Pts',(5.01762739212586,-1.0998254026382,0.138944476607185));
#11913=CARTESIAN_POINT('Ctrl Pts',(4.98558682514019,-1.24600099212803,0.130826599640121));
#11914=CARTESIAN_POINT('Ctrl Pts',(4.94714925029851,-1.3907987628262,0.122708722673057));
#11915=CARTESIAN_POINT('Ctrl Pts',(4.902457660558,-1.53365884372509,0.114590845705993));
#11916=CARTESIAN_POINT('Ctrl Pts',(4.85777553300864,-1.67648867800708,0.106474687471783));
#11917=CARTESIAN_POINT('Ctrl Pts',(4.80684212893725,-1.81738133333755,0.0983585292375734));
#11918=CARTESIAN_POINT('Ctrl Pts',(4.74985030595653,-1.95579207317768,0.0902423710033638));
#11919=CARTESIAN_POINT('Ctrl Pts',(4.6928610457974,-2.09419658893137,0.0821265777384509));
#11920=CARTESIAN_POINT('Ctrl Pts',(4.62981402997828,-2.23011911229002,0.074010784473538));
#11921=CARTESIAN_POINT('Ctrl Pts',(4.56095048152956,-2.36303433481937,0.0658949912086251));
#11922=CARTESIAN_POINT('Ctrl Pts',(4.49209525369898,-2.49593349751974,0.0577801785556347));
#11923=CARTESIAN_POINT('Ctrl Pts',(4.41742504594519,-2.62582579900045,0.0496653659026443));
#11924=CARTESIAN_POINT('Ctrl Pts',(4.33722738088866,-2.75220987734761,0.0415505532496539));
#11925=CARTESIAN_POINT('Ctrl Pts',(4.2570221515381,-2.87860587632023,0.0334349752024494));
#11926=CARTESIAN_POINT('Ctrl Pts',(4.17128859463849,-3.0014927176085,0.025319397155245));
#11927=CARTESIAN_POINT('Ctrl Pts',(4.08035831595364,-3.12039686192766,0.0172038191080405));
#11928=CARTESIAN_POINT('Ctrl Pts',(4.01610542450468,-3.20441656568607,0.0114692127386931));
#11929=CARTESIAN_POINT('Ctrl Pts',(3.94925869462562,-3.28644825652029,0.00573460636934572));
#11930=CARTESIAN_POINT('Ctrl Pts',(3.87994761181449,-3.36633437021265,-1.66533453693773E-15));
#11931=CARTESIAN_POINT('',(-3.87712761685009,-3.36958187393604,0.));
#11932=CARTESIAN_POINT('Origin',(0.,0.,0.));
#11933=CARTESIAN_POINT('Ctrl Pts',(-3.87712761685009,-3.36958187393604,
4.49727061146987E-15));
#11934=CARTESIAN_POINT('Ctrl Pts',(-3.67794676588939,-3.59876448676431,
0.0165613539089372));
#11935=CARTESIAN_POINT('Ctrl Pts',(-3.45883402269643,-3.80983897824898,
0.0332733431119535));
#11936=CARTESIAN_POINT('Ctrl Pts',(-3.09258329567885,-4.10486285593889,
0.0588935811804499));
#11937=CARTESIAN_POINT('Ctrl Pts',(-2.95779534839617,-4.2030249769505,0.0679145294576286));
#11938=CARTESIAN_POINT('Ctrl Pts',(-2.60936178549079,-4.43170327237994,
0.0903703299745524));
#11939=CARTESIAN_POINT('Ctrl Pts',(-2.39050720159611,-4.55348631775,0.103712854959601));
#11940=CARTESIAN_POINT('Ctrl Pts',(-2.09063362584706,-4.69275331719403,
0.121499195248639));
#11941=CARTESIAN_POINT('Ctrl Pts',(-2.01682637619907,-4.72494377940485,
0.125841126992301));
#11942=CARTESIAN_POINT('Ctrl Pts',(-1.70233581227173,-4.85339458642629,
0.144261136625014));
#11943=CARTESIAN_POINT('Ctrl Pts',(-1.45530622128663,-4.93309916368872,
0.15852273649863));
#11944=CARTESIAN_POINT('Ctrl Pts',(-1.05527656046196,-5.02949121427313,
0.181051295485889));
#11945=CARTESIAN_POINT('Ctrl Pts',(-0.905716505943988,-5.05856396129082,
0.18935829443773));
#11946=CARTESIAN_POINT('Ctrl Pts',(-0.432678787318127,-5.12886250479386,
0.215312816039704));
#11947=CARTESIAN_POINT('Ctrl Pts',(-0.106443458305649,-5.14598048110269,
0.23270696890385));
#11948=CARTESIAN_POINT('Ctrl Pts',(0.34892233957708,-5.12652994874249,0.257173627398254));
#11949=CARTESIAN_POINT('Ctrl Pts',(0.478373500791217,-5.11607409352535,
0.264158391034179));
#11950=CARTESIAN_POINT('Ctrl Pts',(0.78908104089943,-5.07908146218344,0.281151389956572));
#11951=CARTESIAN_POINT('Ctrl Pts',(0.96958390305285,-5.04773442969581,0.291195520648721));
#11952=CARTESIAN_POINT('Ctrl Pts',(1.36146745708136,-4.95787856096829,0.3132413220559));
#11953=CARTESIAN_POINT('Ctrl Pts',(1.57156576091593,-4.89533837737919,0.32521413130658));
#11954=CARTESIAN_POINT('Ctrl Pts',(2.0737784553686,-4.7101669225529,0.35425942983852));
#11955=CARTESIAN_POINT('Ctrl Pts',(2.35978606958852,-4.57358099099414,0.371147635061239));
#11956=CARTESIAN_POINT('Ctrl Pts',(2.74718951566983,-4.34250195081651,0.39535775583837));
#11957=CARTESIAN_POINT('Ctrl Pts',(2.86019893378217,-4.26891491972748,0.402607010498784));
#11958=CARTESIAN_POINT('Ctrl Pts',(3.12348935838074,-4.08231830347208,0.420129907503093));
#11959=CARTESIAN_POINT('Ctrl Pts',(3.27071744966058,-3.9653391051075,0.430440616113486));
#11960=CARTESIAN_POINT('Ctrl Pts',(3.5761028785873,-3.69409428874524,0.452836388923162));
#11961=CARTESIAN_POINT('Ctrl Pts',(3.73140140671969,-3.53715866168108,0.464891535223208));
#11962=CARTESIAN_POINT('Ctrl Pts',(4.07122465605871,-3.1463822001139,0.492982350425229));
#11963=CARTESIAN_POINT('Ctrl Pts',(4.24647224751272,-2.90552378445464,0.508873916678694));
#11964=CARTESIAN_POINT('Ctrl Pts',(4.47517449491686,-2.52592336704837,0.532648208012569));
#11965=CARTESIAN_POINT('Ctrl Pts',(4.5450895460534,-2.3978397412183,0.540483436976261));
#11966=CARTESIAN_POINT('Ctrl Pts',(4.69981111166034,-2.08324053907106,0.559513082360392));
#11967=CARTESIAN_POINT('Ctrl Pts',(4.7790983621461,-1.89428947067627,0.570754490415751));
#11968=CARTESIAN_POINT('Ctrl Pts',(4.92097365448571,-1.49005160546221,0.594240358157978));
#11969=CARTESIAN_POINT('Ctrl Pts',(4.98118627467262,-1.27437144825174,0.60645373847293));
#11970=CARTESIAN_POINT('Ctrl Pts',(5.07824358872919,-0.812084167476704,
0.632046342522596));
#11971=CARTESIAN_POINT('Ctrl Pts',(5.11159934270931,-0.565326300837397,
0.645366656085126));
#11972=CARTESIAN_POINT('Ctrl Pts',(5.13765208327986,-0.144128238859615,
0.667992630281884));
#11973=CARTESIAN_POINT('Ctrl Pts',(5.13958963906823,0.0292932019941339,
0.677282382789924));
#11974=CARTESIAN_POINT('Ctrl Pts',(5.12576156181907,0.37983320139103,0.696314066716988));
#11975=CARTESIAN_POINT('Ctrl Pts',(5.10957748483041,0.556705551840665,0.706045732276116));
#11976=CARTESIAN_POINT('Ctrl Pts',(5.06771091843579,0.84734760871232,0.722147861276686));
#11977=CARTESIAN_POINT('Ctrl Pts',(5.04725554703136,0.961719111476853,0.728514237713954));
#11978=CARTESIAN_POINT('Ctrl Pts',(5.00598998697943,1.15447891712609,0.739288911459822));
#11979=CARTESIAN_POINT('Ctrl Pts',(4.98716938784524,1.2332473419332,0.743704999132241));
#11980=CARTESIAN_POINT('Ctrl Pts',(4.92248900032307,1.47817709710584,0.757484618818292));
#11981=CARTESIAN_POINT('Ctrl Pts',(4.87012408715872,1.64249771726079,0.766795339539799));
#11982=CARTESIAN_POINT('Ctrl Pts',(4.70270011315783,2.08889280222995,0.792441569914432));
#11983=CARTESIAN_POINT('Ctrl Pts',(4.57068198165357,2.36383590570105,0.808618117485238));
#11984=CARTESIAN_POINT('Ctrl Pts',(4.31814811777889,2.78850886561886,0.835411388137797));
#11985=CARTESIAN_POINT('Ctrl Pts',(4.21223646506265,2.94605612110679,0.845816787543465));
#11986=CARTESIAN_POINT('Ctrl Pts',(3.96318555833698,3.27555214221487,0.868465063416418));
#11987=CARTESIAN_POINT('Ctrl Pts',(3.81703550485156,3.44475326201248,0.880678412879389));
#11988=CARTESIAN_POINT('Ctrl Pts',(3.43755738543845,3.83017319014098,0.910028833770194));
#11989=CARTESIAN_POINT('Ctrl Pts',(3.19427763230978,4.03529697831146,0.926982737569991));
#11990=CARTESIAN_POINT('Ctrl Pts',(2.82350049240882,4.29325522727336,0.951225207217467));
#11991=CARTESIAN_POINT('Ctrl Pts',(2.71042732998981,4.36552153642016,0.958439225669647));
#11992=CARTESIAN_POINT('Ctrl Pts',(2.43253339794523,4.52816395244855,0.975923313940613));
#11993=CARTESIAN_POINT('Ctrl Pts',(2.26532985933429,4.61408349444963,0.986230991954779));
#11994=CARTESIAN_POINT('Ctrl Pts',(1.89239357250138,4.78055372433496,1.00862415092931));
#11995=CARTESIAN_POINT('Ctrl Pts',(1.68540303190607,4.85739306715182,1.02067970430198));
#11996=CARTESIAN_POINT('Ctrl Pts',(1.18934426571286,5.00599954024447,1.04876913223415));
#11997=CARTESIAN_POINT('Ctrl Pts',(0.89770629447462,5.06642856938913,1.06465896497858));
#11998=CARTESIAN_POINT('Ctrl Pts',(0.457631110645011,5.11840288465141,1.08843129162848));
#11999=CARTESIAN_POINT('Ctrl Pts',(0.312122433197049,5.129332578545,1.09626630778173));
#12000=CARTESIAN_POINT('Ctrl Pts',(-0.0379702776302637,5.14067588196109,
1.1152791392755));
#12001=CARTESIAN_POINT('Ctrl Pts',(-0.242499004021474,5.13509324416503,
1.12650355857268));
#12002=CARTESIAN_POINT('Ctrl Pts',(-0.6692274883726,5.09788958232329,1.14998594167575));
#12003=CARTESIAN_POINT('Ctrl Pts',(-0.890801469099042,5.06387402817349,
1.16221264436448));
#12004=CARTESIAN_POINT('Ctrl Pts',(-1.35077562034394,4.96212585850705,1.18773635945147));
#12005=CARTESIAN_POINT('Ctrl Pts',(-1.58793497065248,4.89139584885384,1.20097686756525));
#12006=CARTESIAN_POINT('Ctrl Pts',(-1.98173820068383,4.74227423996327,1.22355376393861));
#12007=CARTESIAN_POINT('Ctrl Pts',(-2.14115816562501,4.67246088888614,1.23287493450321));
#12008=CARTESIAN_POINT('Ctrl Pts',(-2.45881379811487,4.51367612881655,1.25213847658075));
#12009=CARTESIAN_POINT('Ctrl Pts',(-2.61649813803016,4.42413476899977,1.26207510876547));
#12010=CARTESIAN_POINT('Ctrl Pts',(-2.97860362880383,4.19237199858659,1.28565029941015));
#12011=CARTESIAN_POINT('Ctrl Pts',(-3.17808721282558,4.04324546800822,1.29924846941561));
#12012=CARTESIAN_POINT('Ctrl Pts',(-3.51169963555394,3.75384835361944,1.32318227012894));
#12013=CARTESIAN_POINT('Ctrl Pts',(-3.65018170213261,3.61933521208265,1.33355114534632));
#12014=CARTESIAN_POINT('Ctrl Pts',(-3.92026463845979,3.32568584159246,1.35495200457925));
#12015=CARTESIAN_POINT('Ctrl Pts',(-4.05050341498609,3.16576701487549,1.36596134553038));
#12016=CARTESIAN_POINT('Ctrl Pts',(-4.21235227040537,2.94063944829266,1.38095379298858));
#12017=CARTESIAN_POINT('Ctrl Pts',(-4.25271201107483,2.88196306841854,1.38482184364391));
#12018=CARTESIAN_POINT('Ctrl Pts',(-4.29183622715607,2.82247096739201,1.38870419915418));
#12019=CARTESIAN_POINT('Origin',(0.,0.,0.));
#12020=CARTESIAN_POINT('Ctrl Pts',(-4.29183622715607,2.82247096739201,1.38870419915418));
#12021=CARTESIAN_POINT('Ctrl Pts',(-4.31141166714452,2.79270464438086,1.39064669985879));
#12022=CARTESIAN_POINT('Ctrl Pts',(-4.33067781498162,2.7627340977274,1.39259244493516));
#12023=CARTESIAN_POINT('Ctrl Pts',(-4.51934871643038,2.46241218084559,1.41198450141167));
#12024=CARTESIAN_POINT('Ctrl Pts',(-4.66353332528833,2.17702800889423,1.42951622892346));
#12025=CARTESIAN_POINT('Ctrl Pts',(-4.84874005285254,1.70612859728417,1.45699470652792));
#12026=CARTESIAN_POINT('Ctrl Pts',(-4.90762112400106,1.52853261964258,1.46706850157614));
#12027=CARTESIAN_POINT('Ctrl Pts',(-5.01939924697197,1.11755322245494,1.4899392981333));
#12028=CARTESIAN_POINT('Ctrl Pts',(-5.06594377540955,0.882895526417692,
1.50268213900738));
#12029=CARTESIAN_POINT('Ctrl Pts',(-5.10916066820828,0.541902040532461,
1.52126208035794));
#12030=CARTESIAN_POINT('Ctrl Pts',(-5.11915130749457,0.437572172905712,
1.52696533204475));
#12031=CARTESIAN_POINT('Ctrl Pts',(-5.14036681225492,0.111008979525595,
1.54485261825289));
#12032=CARTESIAN_POINT('Ctrl Pts',(-5.14035198390431,-0.111696981736819,
1.55707921641052));
#12033=CARTESIAN_POINT('Ctrl Pts',(-5.12068037764657,-0.413868710161159,
1.57362677475726));
#12034=CARTESIAN_POINT('Ctrl Pts',(-5.113581257039,-0.493904600531326,1.57800711312869));
#12035=CARTESIAN_POINT('Ctrl Pts',(-5.08520518934513,-0.746367912630681,
1.59182285114144));
#12036=CARTESIAN_POINT('Ctrl Pts',(-5.05705804447842,-0.917901261478106,
1.60120387894329));
#12037=CARTESIAN_POINT('Ctrl Pts',(-4.96805251722242,-1.32871300747945,
1.62380954986378));
#12038=CARTESIAN_POINT('Ctrl Pts',(-4.89854093047065,-1.56566882709781,
1.63695767537244));
#12039=CARTESIAN_POINT('Ctrl Pts',(-4.77768946535749,-1.8893552738304,1.65558489834132));
#12040=CARTESIAN_POINT('Ctrl Pts',(-4.74043272869375,-1.98097878584997,
1.66094358692037));
#12041=CARTESIAN_POINT('Ctrl Pts',(-4.60508239316641,-2.28811419298573,
1.67924125183664));
#12042=CARTESIAN_POINT('Ctrl Pts',(-4.49474713708642,-2.49789882629554,
1.69226091047833));
#12043=CARTESIAN_POINT('Ctrl Pts',(-4.27545647508133,-2.85294114281389,
1.71508529103285));
#12044=CARTESIAN_POINT('Ctrl Pts',(-4.17254040925077,-3.00145131639488,
1.7249075314345));
#12045=CARTESIAN_POINT('Ctrl Pts',(-4.01390746121736,-3.20638813345496,
1.73892180881287));
#12046=CARTESIAN_POINT('Ctrl Pts',(-3.96437763307514,-3.26742836552705,
1.74315998107736));
#12047=CARTESIAN_POINT('Ctrl Pts',(-3.78178821157069,-3.48218379783606,
1.75832959751573));
#12048=CARTESIAN_POINT('Ctrl Pts',(-3.64103255844747,-3.62910568764466,
1.76919264782912));
#12049=CARTESIAN_POINT('Ctrl Pts',(-3.43642165873281,-3.81876125601511,
1.78417592482309));
#12050=CARTESIAN_POINT('Ctrl Pts',(-3.37977137045612,-3.86898909760957,
1.78824820687431));
#12051=CARTESIAN_POINT('Ctrl Pts',(-3.24490383790619,-3.98334347723956,
1.79779907114967));
#12052=CARTESIAN_POINT('Ctrl Pts',(-3.16586326002202,-4.0464472197234,1.80329583339986));
#12053=CARTESIAN_POINT('Ctrl Pts',(-2.97262834866866,-4.19159129141606,
1.81649532033844));
#12054=CARTESIAN_POINT('Ctrl Pts',(-2.85682665152495,-4.27135786086577,
1.82420808002789));
#12055=CARTESIAN_POINT('Ctrl Pts',(-2.55720146267498,-4.46010432807095,
1.843622205695));
#12056=CARTESIAN_POINT('Ctrl Pts',(-2.36957635092301,-4.5625564177526,1.85528941963915));
#12057=CARTESIAN_POINT('Ctrl Pts',(-1.97469236155925,-4.74723460680782,
1.8789303816139));
#12058=CARTESIAN_POINT('Ctrl Pts',(-1.76736133874764,-4.82825880858382,
1.89087141787454));
#12059=CARTESIAN_POINT('Ctrl Pts',(-1.35848056167132,-4.95816861655219,
1.91387638233383));
#12060=CARTESIAN_POINT('Ctrl Pts',(-1.15793765458368,-5.0088005241963,1.92492410092325));
#12061=CARTESIAN_POINT('Ctrl Pts',(-0.810115838898992,-5.07460583021643,
1.94411172691831));
#12062=CARTESIAN_POINT('Ctrl Pts',(-0.664227260001339,-5.09575436093513,
1.95217413987132));
#12063=CARTESIAN_POINT('Ctrl Pts',(-0.224205717253499,-5.14032258787291,
1.97641757494));
#12064=CARTESIAN_POINT('Ctrl Pts',(0.0712459142612628,-5.14471732046345,
1.99256637832505));
#12065=CARTESIAN_POINT('Ctrl Pts',(0.584314172565213,-5.10812354573329,
2.02042862672598));
#12066=CARTESIAN_POINT('Ctrl Pts',(0.801963171469988,-5.07850438433339,
2.0322006848874));
#12067=CARTESIAN_POINT('Ctrl Pts',(1.2032638579666,-4.99744394827057,2.05415079295371));
#12068=CARTESIAN_POINT('Ctrl Pts',(1.38724179637618,-4.94953003756478,2.06431655169254));
#12069=CARTESIAN_POINT('Ctrl Pts',(1.69726933951955,-4.85014079745769,2.08195713025871));
#12070=CARTESIAN_POINT('Ctrl Pts',(1.82470738519257,-4.80364761347787,2.08937006591804));
#12071=CARTESIAN_POINT('Ctrl Pts',(2.24138331453824,-4.63265576006546,2.11404942497428));
#12072=CARTESIAN_POINT('Ctrl Pts',(2.52101923036853,-4.48662121468314,2.13129573017535));
#12073=CARTESIAN_POINT('Ctrl Pts',(2.97281583180695,-4.19502751127474,2.1604123509012));
#12074=CARTESIAN_POINT('Ctrl Pts',(3.15204066944918,-4.06208466874455,2.17236480419372));
#12075=CARTESIAN_POINT('Ctrl Pts',(3.46799012604106,-3.79418624669297,2.19457327312554));
#12076=CARTESIAN_POINT('Ctrl Pts',(3.6068868057623,-3.66239945016972,2.20481540706834));
#12077=CARTESIAN_POINT('Ctrl Pts',(3.85823291506199,-3.39572008051004,2.22469796506014));
#12078=CARTESIAN_POINT('Ctrl Pts',(3.97176141901386,-3.26220564490393,2.23430001569753));
#12079=CARTESIAN_POINT('Ctrl Pts',(4.2262139065245,-2.92993919161391,2.25724918189883));
#12080=CARTESIAN_POINT('Ctrl Pts',(4.36026584482773,-2.72644712183987,2.27056003177417));
#12081=CARTESIAN_POINT('Ctrl Pts',(4.58891772585733,-2.31907561490368,2.29589345796691));
#12082=CARTESIAN_POINT('Ctrl Pts',(4.68558031649715,-2.11698314038772,2.30790920922863));
#12083=CARTESIAN_POINT('Ctrl Pts',(4.84481696450797,-1.71925154252139,2.33088155637874));
#12084=CARTESIAN_POINT('Ctrl Pts',(4.90945504653299,-1.52490174988738,2.34182293582193));
#12085=CARTESIAN_POINT('Ctrl Pts',(5.00003926780489,-1.18621740950124,2.36082543105876));
#12086=CARTESIAN_POINT('Ctrl Pts',(5.03172400004837,-1.04367446005091,2.3688110013006));
#12087=CARTESIAN_POINT('Ctrl Pts',(5.10934922604341,-0.607471373211402,
2.39309649364469));
#12088=CARTESIAN_POINT('Ctrl Pts',(5.13592870127669,-0.310990825811056,
2.40936532209319));
#12089=CARTESIAN_POINT('Ctrl Pts',(5.1373267443539,0.206579087863292,2.43739993271944));
#12090=CARTESIAN_POINT('Ctrl Pts',(5.1237297641605,0.426845181964274,2.44922599880147));
#12091=CARTESIAN_POINT('Ctrl Pts',(5.07239118242162,0.832111030281952,2.47112760193419));
#12092=CARTESIAN_POINT('Ctrl Pts',(5.03853323482339,1.01722241977832,2.48119125524799));
#12093=CARTESIAN_POINT('Ctrl Pts',(4.96322250420805,1.33066374794971,2.49865717613434));
#12094=CARTESIAN_POINT('Ctrl Pts',(4.92673108004532,1.45998732328115,2.50599934816381));
#12095=CARTESIAN_POINT('Ctrl Pts',(4.78717135690065,1.8893925886892,2.53073869295086));
#12096=CARTESIAN_POINT('Ctrl Pts',(4.66139430778449,2.18133596579021,2.54811746667217));
#12097=CARTESIAN_POINT('Ctrl Pts',(4.40405758253498,2.65310297354305,2.57721447167864));
#12098=CARTESIAN_POINT('Ctrl Pts',(4.28630290147522,2.83941691267552,2.58902167958839));
#12099=CARTESIAN_POINT('Ctrl Pts',(4.05037228469111,3.16442773986515,2.61055349693758));
#12100=CARTESIAN_POINT('Ctrl Pts',(3.936086367198,3.30550154142237,2.62026684610574));
#12101=CARTESIAN_POINT('Ctrl Pts',(3.72739054895614,3.53690662520179,2.63714733539855));
#12102=CARTESIAN_POINT('Ctrl Pts',(3.63655980579654,3.63023140921971,2.6442605209355));
#12103=CARTESIAN_POINT('Ctrl Pts',(3.30667633459527,3.94435512283217,2.66921451597319));
#12104=CARTESIAN_POINT('Ctrl Pts',(3.0502789600889,4.14582371024468,2.68704314377013));
#12105=CARTESIAN_POINT('Ctrl Pts',(2.5892076168806,4.44204776925775,2.71671100842295));
#12106=CARTESIAN_POINT('Ctrl Pts',(2.39423586960612,4.55010125589898,2.72864847294603));
#12107=CARTESIAN_POINT('Ctrl Pts',(2.0235080441058,4.72511270438161,2.75062757006997));
#12108=CARTESIAN_POINT('Ctrl Pts',(1.84990692018692,4.79573943034203,2.7606556209678));
#12109=CARTESIAN_POINT('Ctrl Pts',(1.50756783501789,4.9136540143316,2.78029786142779));
#12110=CARTESIAN_POINT('Ctrl Pts',(1.33949838561722,4.96210630219023,2.78988054898158));
#12111=CARTESIAN_POINT('Ctrl Pts',(0.931010247072214,5.05759826221133,2.8128842813617));
#12112=CARTESIAN_POINT('Ctrl Pts',(0.689050509106018,5.09620390254759,2.82626898240154));
#12113=CARTESIAN_POINT('Ctrl Pts',(0.222224703879941,5.13682174297132,2.85168019626704));
#12114=CARTESIAN_POINT('Ctrl Pts',(-0.00184217065915739,5.14162629554737,
2.86370111824652));
#12115=CARTESIAN_POINT('Ctrl Pts',(-0.429811238103686,5.12281978570965,
2.88667120785942));
#12116=CARTESIAN_POINT('Ctrl Pts',(-0.633390554240987,5.10165008435015,
2.89760522478219));
#12117=CARTESIAN_POINT('Ctrl Pts',(-0.979080582536843,5.04468800522704,
2.91659481129789));
#12118=CARTESIAN_POINT('Ctrl Pts',(-1.12192229200466,5.01485439448364,2.92457496863274));
#12119=CARTESIAN_POINT('Ctrl Pts',(-1.55142586968957,4.9058781773376,2.94886351004635));
#12120=CARTESIAN_POINT('Ctrl Pts',(-1.83267253594294,4.80789790270234,2.96514088252546));
#12121=CARTESIAN_POINT('Ctrl Pts',(-2.30505156043652,4.59582108344528,2.99318787011608));
#12122=CARTESIAN_POINT('Ctrl Pts',(-2.50021299084452,4.4926352663032,3.00501788652547));
#12123=CARTESIAN_POINT('Ctrl Pts',(-2.84825957756841,4.2788930127771,3.02691594043159));
#12124=CARTESIAN_POINT('Ctrl Pts',(-3.00286004790986,4.17185056170326,3.03697212151953));
#12125=CARTESIAN_POINT('Ctrl Pts',(-3.25725051026099,3.97423425812866,3.05442532884527));
#12126=CARTESIAN_POINT('Ctrl Pts',(-3.35998524110482,3.88776497340196,3.06176239048907));
#12127=CARTESIAN_POINT('Ctrl Pts',(-3.69383167968171,3.58364795508103,3.0865061775217));
#12128=CARTESIAN_POINT('Ctrl Pts',(-3.90814534258248,3.34863176145679,3.10389463153942));
#12129=CARTESIAN_POINT('Ctrl Pts',(-4.16649034429435,3.00648554434302,3.12710801500211));
#12130=CARTESIAN_POINT('Ctrl Pts',(-4.23066960584482,2.91548064671473,3.13311049086494));
#12131=CARTESIAN_POINT('Ctrl Pts',(-4.29183621895492,2.82247097986264,3.13909688836532));
#12132=CARTESIAN_POINT('',(-5.13674999831709,-0.000131489181014188,1.07404150530312));
#12133=CARTESIAN_POINT('Ctrl Pts',(-4.29199677360937,2.82257643420045,2.66202500160396));
#12134=CARTESIAN_POINT('Ctrl Pts',(-4.21753523086708,2.93604918894789,2.65466501958149));
#12135=CARTESIAN_POINT('Ctrl Pts',(-3.64162075244998,3.74186919945967,2.60099021202329));
#12136=CARTESIAN_POINT('Ctrl Pts',(-2.13912211940093,4.90889399862105,2.50100057892936));
#12137=CARTESIAN_POINT('Ctrl Pts',(0.470139480393059,5.33404654130231,2.36205610232219));
#12138=CARTESIAN_POINT('Ctrl Pts',(2.96480561398902,4.45903705461135,2.22311162571499));
#12139=CARTESIAN_POINT('Ctrl Pts',(4.73680694601427,2.49714709212602,2.0841671491078));
#12140=CARTESIAN_POINT('Ctrl Pts',(5.35422202774455,-0.0734168574314198,
1.94522267250061));
#12141=CARTESIAN_POINT('Ctrl Pts',(4.66655737753191,-2.6260858009926,1.80627819589344));
#12142=CARTESIAN_POINT('Ctrl Pts',(2.84142957722535,-4.53865176071962,1.66733371928624));
#12143=CARTESIAN_POINT('Ctrl Pts',(0.323709801564174,-5.34493211998566,
1.52838924267905));
#12144=CARTESIAN_POINT('Ctrl Pts',(-2.27291392243804,-4.84839564767857,
1.38944476607187));
#12145=CARTESIAN_POINT('Ctrl Pts',(-4.31551911731205,-3.17007628077776,
1.25050028946468));
#12146=CARTESIAN_POINT('Ctrl Pts',(-5.06515352982256,-1.31547226615614,
1.14536587063201));
#12147=CARTESIAN_POINT('Ctrl Pts',(-5.13687131111266,-0.230764757637239,
1.08654627733508));
#12148=CARTESIAN_POINT('Ctrl Pts',(-5.13664618448387,-0.00013156529178269,
1.07404150957387));
#12149=CARTESIAN_POINT('Ctrl Pts',(-5.13674999831709,-0.000131489181014244,
1.07404150530312));
#12150=CARTESIAN_POINT('Ctrl Pts',(-5.13675398895607,0.15576662052808,1.06558899121539));
#12151=CARTESIAN_POINT('Ctrl Pts',(-5.12965553311713,0.311682248976567,
1.05713647712765));
#12152=CARTESIAN_POINT('Ctrl Pts',(-5.11548157266034,0.466957002594934,
1.04868396303992));
#12153=CARTESIAN_POINT('Ctrl Pts',(-5.10198818049961,0.614776177738121,
1.0406372997465));
#12154=CARTESIAN_POINT('Ctrl Pts',(-5.08208291523897,0.762014223800285,
1.03259063645309));
#12155=CARTESIAN_POINT('Ctrl Pts',(-5.0558422630955,0.908107688106076,1.02454397315967));
#12156=CARTESIAN_POINT('Ctrl Pts',(-5.029601885012,1.05419962659724,1.01649739390641));
#12157=CARTESIAN_POINT('Ctrl Pts',(-4.99702631447217,1.19914667878811,1.00845081465314));
#12158=CARTESIAN_POINT('Ctrl Pts',(-4.95824328173864,1.34239492013103,1.00040423539987));
#12159=CARTESIAN_POINT('Ctrl Pts',(-4.91945171273043,1.48567469088904,0.992355885067712));
#12160=CARTESIAN_POINT('Ctrl Pts',(-4.87445004172093,1.62725458178626,0.98430753473555));
#12161=CARTESIAN_POINT('Ctrl Pts',(-4.82341619095162,1.76659469357456,0.976259184403386));
#12162=CARTESIAN_POINT('Ctrl Pts',(-4.81570596750665,1.7876462775828,0.975043235019029));
#12163=CARTESIAN_POINT('Ctrl Pts',(-4.80785814898297,1.80864676985546,0.973827285634671));
#12164=CARTESIAN_POINT('Ctrl Pts',(-4.79987344606763,1.82959434417437,0.972611336250314));
#12165=CARTESIAN_POINT('Ctrl Pts',(-4.7468948658969,1.96858170002269,0.96454350046158));
#12166=CARTESIAN_POINT('Ctrl Pts',(-4.68786554548279,2.10529213254811,0.956475664672847));
#12167=CARTESIAN_POINT('Ctrl Pts',(-4.62300639714695,2.2391990564571,0.948407828884113));
#12168=CARTESIAN_POINT('Ctrl Pts',(-4.5581579010614,2.37308398793935,0.940341318129831));
#12169=CARTESIAN_POINT('Ctrl Pts',(-4.48748163017484,2.50416603095612,0.932274807375549));
#12170=CARTESIAN_POINT('Ctrl Pts',(-4.41124562792507,2.63194083759721,0.924208296621267));
#12171=CARTESIAN_POINT('Ctrl Pts',(-4.37283988231778,2.69631051300072,0.92014459507836));
#12172=CARTESIAN_POINT('Ctrl Pts',(-4.33302387301076,2.75984122459489,0.916080893535454));
#12173=CARTESIAN_POINT('Ctrl Pts',(-4.29183622825303,2.82247096572397,0.912017191992546));
#12174=CARTESIAN_POINT('Origin',(0.,0.,-3.86474103256053));
#12175=CARTESIAN_POINT('',(-6.11324999844244,0.000137998184040776,2.26025896739919));
#12176=CARTESIAN_POINT('Ctrl Pts',(3.72292453512039,-4.84888218750453,1.13013653271955));
#12177=CARTESIAN_POINT('Ctrl Pts',(3.8573754093748,-4.74565211525817,1.13785962463316));
#12178=CARTESIAN_POINT('Ctrl Pts',(3.98754469999778,-4.63681523196678,1.14558271654677));
#12179=CARTESIAN_POINT('Ctrl Pts',(4.1129725893008,-4.52275160075813,1.15330580846038));
#12180=CARTESIAN_POINT('Ctrl Pts',(4.23840615502252,-4.40868280743656,1.16102924989358));
#12181=CARTESIAN_POINT('Ctrl Pts',(4.35909765329052,-4.28938700356551,1.16875269132677));
#12182=CARTESIAN_POINT('Ctrl Pts',(4.47462201540418,-4.16528310943689,1.17647613275996));
#12183=CARTESIAN_POINT('Ctrl Pts',(4.59014003349401,-4.04118603047735,1.18419915006014));
#12184=CARTESIAN_POINT('Ctrl Pts',(4.70049126774584,-3.91228162202903,1.19192216736031));
#12185=CARTESIAN_POINT('Ctrl Pts',(4.80528891848427,-3.77902420902437,1.19964518466048));
#12186=CARTESIAN_POINT('Ctrl Pts',(4.91011305231619,-3.64573312094682,1.20737015362072));
#12187=CARTESIAN_POINT('Ctrl Pts',(5.00938060121277,-3.50808707864231,1.21509512258095));
#12188=CARTESIAN_POINT('Ctrl Pts',(5.10274576734098,-3.36657261861135,1.22282009154118));
#12189=CARTESIAN_POINT('Ctrl Pts',(5.18201307759727,-3.24642641126009,1.22937861370404));
#12190=CARTESIAN_POINT('Ctrl Pts',(5.25702655387851,-3.12349244938812,1.2359371358669));
#12191=CARTESIAN_POINT('Ctrl Pts',(5.32759941172684,-2.99808440019087,1.24249565802976));
#12192=CARTESIAN_POINT('Ctrl Pts',(5.41072151689508,-2.85037632413816,1.25022041490642));
#12193=CARTESIAN_POINT('Ctrl Pts',(5.48771173147153,-2.69918311039753,1.25794517178308));
#12194=CARTESIAN_POINT('Ctrl Pts',(5.55829382787376,-2.54503345469572,1.26566992865974));
#12195=CARTESIAN_POINT('Ctrl Pts',(5.62886215520052,-2.39091387033428,1.27339317859957));
#12196=CARTESIAN_POINT('Ctrl Pts',(5.69302472686585,-2.23383928279505,1.2811164285394));
#12197=CARTESIAN_POINT('Ctrl Pts',(5.7505524945068,-2.07436052084049,1.28883967847924));
#12198=CARTESIAN_POINT('Ctrl Pts',(5.80808248480531,-1.91487559722365,1.29656322681653));
#12199=CARTESIAN_POINT('Ctrl Pts',(5.85897704685537,-1.75298661008816,1.30428677515382));
#12200=CARTESIAN_POINT('Ctrl Pts',(5.90305600247511,-1.58926253153549,1.31201032349112));
#12201=CARTESIAN_POINT('Ctrl Pts',(5.94713199739441,-1.42554945002085,1.31973335305221));
#12202=CARTESIAN_POINT('Ctrl Pts',(5.98439321960548,-1.26000182981357,1.32745638261331));
#12203=CARTESIAN_POINT('Ctrl Pts',(6.01470986616232,-1.09320208030794,1.33517941217441));
#12204=CARTESIAN_POINT('Ctrl Pts',(6.0450345695927,-0.926358002532552,1.34290449418785));
#12205=CARTESIAN_POINT('Ctrl Pts',(6.0684109506079,-0.758261442167187,1.3506295762013));
#12206=CARTESIAN_POINT('Ctrl Pts',(6.08476050236919,-0.589504191085879,
1.35835465821474));
#12207=CARTESIAN_POINT('Ctrl Pts',(6.10104672392827,-0.421400623420052,
1.36604981702215));
#12208=CARTESIAN_POINT('Ctrl Pts',(6.11036045856332,-0.252641788184692,
1.37374497582955));
#12209=CARTESIAN_POINT('Ctrl Pts',(6.1126753807856,-0.0838167742016235,
1.38144013463695));
#12210=CARTESIAN_POINT('Ctrl Pts',(6.11499920959529,0.085657788491336,1.38916490031574));
#12211=CARTESIAN_POINT('Ctrl Pts',(6.11027105680977,0.25525906309682,1.39688966599452));
#12212=CARTESIAN_POINT('Ctrl Pts',(6.09850130396609,0.424390631404504,1.40461443167331));
#12213=CARTESIAN_POINT('Ctrl Pts',(6.08673384695857,0.593489208503662,1.41233769054082));
#12214=CARTESIAN_POINT('Ctrl Pts',(6.06792755260796,0.762117946154579,1.42006094940833));
#12215=CARTESIAN_POINT('Ctrl Pts',(6.04214482084422,0.929683562533715,1.42778420827583));
#12216=CARTESIAN_POINT('Ctrl Pts',(6.01636109256515,1.09725565540678,1.43550776565111));
#12217=CARTESIAN_POINT('Ctrl Pts',(5.98360043158213,1.26376423095059,1.44323132302639));
#12218=CARTESIAN_POINT('Ctrl Pts',(5.94397683230493,1.42862345617108,1.45095488040167));
#12219=CARTESIAN_POINT('Ctrl Pts',(5.90435589424919,1.59347160902775,1.45867791904324));
#12220=CARTESIAN_POINT('Ctrl Pts',(5.85787301437743,1.75667032506029,1.46640095768481));
#12221=CARTESIAN_POINT('Ctrl Pts',(5.80469285169398,1.91764607266118,1.47412399632638));
#12222=CARTESIAN_POINT('Ctrl Pts',(5.75149855611477,2.07866460037678,1.48184908740432));
#12223=CARTESIAN_POINT('Ctrl Pts',(5.69160351859424,2.23745867734327,1.48957417848227));
#12224=CARTESIAN_POINT('Ctrl Pts',(5.62522193143055,2.39347107453856,1.49729926956021));
#12225=CARTESIAN_POINT('Ctrl Pts',(5.55909793773548,2.54887806628547,1.50499438345485));
#12226=CARTESIAN_POINT('Ctrl Pts',(5.48653779880018,2.70152465381282,1.51268949734949));
#12227=CARTESIAN_POINT('Ctrl Pts',(5.40780022989844,2.85088095788134,1.52038461124413));
#12228=CARTESIAN_POINT('Ctrl Pts',(5.32875931489969,3.00081267534571,1.52810937150453));
#12229=CARTESIAN_POINT('Ctrl Pts',(5.24346525628034,3.14748179386505,1.53583413176492));
#12230=CARTESIAN_POINT('Ctrl Pts',(5.1522125135047,3.29036955039788,1.54355889202531));
#12231=CARTESIAN_POINT('Ctrl Pts',(5.06097757157155,3.43322943354991,1.55128214540233));
#12232=CARTESIAN_POINT('Ctrl Pts',(4.96378643530744,3.57230915962419,1.55900539877935));
#12233=CARTESIAN_POINT('Ctrl Pts',(4.8609777423659,3.70711760681036,1.56672865215637));
#12234=CARTESIAN_POINT('Ctrl Pts',(4.75816507661087,3.84193126336939,1.57445220398136));
#12235=CARTESIAN_POINT('Ctrl Pts',(4.64973460882364,3.97247305635589,1.58217575580634));
#12236=CARTESIAN_POINT('Ctrl Pts',(4.53606671939524,4.09828308925761,1.58989930763133));
#12237=CARTESIAN_POINT('Ctrl Pts',(4.4224064645163,4.22408467207792,1.59762234070085));
#12238=CARTESIAN_POINT('Ctrl Pts',(4.30350970444383,4.34515489562437,1.60534537377038));
#12239=CARTESIAN_POINT('Ctrl Pts',(4.17979542414352,4.46106890496089,1.6130684068399));
#12240=CARTESIAN_POINT('Ctrl Pts',(4.05604826585309,4.57701371930749,1.62079349236291));
#12241=CARTESIAN_POINT('Ctrl Pts',(3.92748125894714,4.68779936281262,1.62851857788591));
#12242=CARTESIAN_POINT('Ctrl Pts',(3.79454908524854,4.79303899443135,1.63624366340891));
#12243=CARTESIAN_POINT('Ctrl Pts',(3.66213218437205,4.89787069529506,1.64393880488972));
#12244=CARTESIAN_POINT('Ctrl Pts',(3.52538416193958,4.99719913435962,1.65163394637052));
#12245=CARTESIAN_POINT('Ctrl Pts',(3.38478571790181,5.09068278390904,1.65932908785133));
#12246=CARTESIAN_POINT('Ctrl Pts',(3.24364606032508,5.18452628535551,1.66705385067526));
#12247=CARTESIAN_POINT('Ctrl Pts',(3.09857627483836,5.27251312228381,1.67477861349919));
#12248=CARTESIAN_POINT('Ctrl Pts',(2.95008312582068,5.35432863328803,1.68250337632312));
#12249=CARTESIAN_POINT('Ctrl Pts',(2.80161894301487,5.43612818473155,1.6902266322956));
#12250=CARTESIAN_POINT('Ctrl Pts',(2.64973300656674,5.51175865946843,1.69794988826809));
#12251=CARTESIAN_POINT('Ctrl Pts',(2.4949576504884,5.58095080472579,1.70567314424057));
#12252=CARTESIAN_POINT('Ctrl Pts',(2.34017631296394,5.65014562398176,1.71339669868589));
#12253=CARTESIAN_POINT('Ctrl Pts',(2.182505620068,5.71290148290529,1.72112025313121));
#12254=CARTESIAN_POINT('Ctrl Pts',(2.02249962209345,5.76899651942449,1.72884380757653));
#12255=CARTESIAN_POINT('Ctrl Pts',(1.86250437080764,5.82508778836056,1.73656684327482));
#12256=CARTESIAN_POINT('Ctrl Pts',(1.70017442743467,5.87451902529616,1.74428987897312));
#12257=CARTESIAN_POINT('Ctrl Pts',(1.5360809770284,5.91711760864287,1.75201291467141));
#12258=CARTESIAN_POINT('Ctrl Pts',(1.37194391781922,5.95972751281451,1.75973800281202));
#12259=CARTESIAN_POINT('Ctrl Pts',(1.20604272150252,5.99550105315179,1.76746309095263));
#12260=CARTESIAN_POINT('Ctrl Pts',(1.03896173250995,6.02431606747852,1.77518817909324));
#12261=CARTESIAN_POINT('Ctrl Pts',(0.872528722387847,6.05301933048904,1.78288330754833));
#12262=CARTESIAN_POINT('Ctrl Pts',(0.704925367465891,6.07481792380217,1.79057843600341));
#12263=CARTESIAN_POINT('Ctrl Pts',(0.536737176574621,6.08964192426638,1.7982735644585));
#12264=CARTESIAN_POINT('Ctrl Pts',(0.367901302971622,6.10452301107397,1.80599832639521));
#12265=CARTESIAN_POINT('Ctrl Pts',(0.198416280939758,6.11238092141685,1.81372308833193));
#12266=CARTESIAN_POINT('Ctrl Pts',(0.0288776565905395,6.11318179375109,
1.82144785026864));
#12267=CARTESIAN_POINT('Ctrl Pts',(-0.140627896034936,6.11398250986,1.82917110534405));
#12268=CARTESIAN_POINT('Ctrl Pts',(-0.310186713383548,6.10772893329223,
1.83689436041945));
#12269=CARTESIAN_POINT('Ctrl Pts',(-0.479202520794083,6.09443931027003,
1.84461761549486));
#12270=CARTESIAN_POINT('Ctrl Pts',(-0.648224859840653,6.08114917366876,
1.85234116903638));
#12271=CARTESIAN_POINT('Ctrl Pts',(-0.816703830704214,6.06082246740018,
1.86006472257791));
#12272=CARTESIAN_POINT('Ctrl Pts',(-0.984046762183985,6.03352944240228,
1.86778827611943));
#12273=CARTESIAN_POINT('Ctrl Pts',(-1.15137845415264,6.00623825052787,1.87551131091203));
#12274=CARTESIAN_POINT('Ctrl Pts',(-1.31757394660641,5.97198172727477,1.88323434570462));
#12275=CARTESIAN_POINT('Ctrl Pts',(-1.48204907994823,5.93088156070618,1.89095738049722));
#12276=CARTESIAN_POINT('Ctrl Pts',(-1.64656792365069,5.88977047149496,1.89868246773768));
#12277=CARTESIAN_POINT('Ctrl Pts',(-1.8093651864335,5.84181217944948,1.90640755497814));
#12278=CARTESIAN_POINT('Ctrl Pts',(-1.96986929436292,5.78717897819189,1.9141326422186));
#12279=CARTESIAN_POINT('Ctrl Pts',(-2.12975104209433,5.73275761905093,1.92182777516763));
#12280=CARTESIAN_POINT('Ctrl Pts',(-2.28735710178446,5.67171315417662,1.92952290811666));
#12281=CARTESIAN_POINT('Ctrl Pts',(-2.44213986854364,5.60426430720123,1.93721804106569));
#12282=CARTESIAN_POINT('Ctrl Pts',(-2.59751860636432,5.53655575714796,1.94494280313073));
#12283=CARTESIAN_POINT('Ctrl Pts',(-2.75010728523121,5.46236940070029,1.95266756519576));
#12284=CARTESIAN_POINT('Ctrl Pts',(-2.8993667401887,5.38196042984223,1.9603923272608));
#12285=CARTESIAN_POINT('Ctrl Pts',(-3.04859707926959,5.30156714427307,1.96811558246505));
#12286=CARTESIAN_POINT('Ctrl Pts',(-3.19449921143748,5.21495381655532,1.97583883766931));
#12287=CARTESIAN_POINT('Ctrl Pts',(-3.33655826185793,5.12242174442202,1.98356209287356));
#12288=CARTESIAN_POINT('Ctrl Pts',(-3.47862280215923,5.02988609638103,1.9912856465435));
#12289=CARTESIAN_POINT('Ctrl Pts',(-3.61684369580897,4.93143141587311,1.99900920021343));
#12290=CARTESIAN_POINT('Ctrl Pts',(-3.75073411284258,4.82740294332874,2.00673275388336));
#12291=CARTESIAN_POINT('Ctrl Pts',(-3.8846155371794,4.72338145781549,2.01445578880387));
#12292=CARTESIAN_POINT('Ctrl Pts',(-4.01416681666281,4.61378712389629,2.02217882372439));
#12293=CARTESIAN_POINT('Ctrl Pts',(-4.13893320461471,4.49900627808384,2.0299018586449));
#12294=CARTESIAN_POINT('Ctrl Pts',(-4.26373275003021,4.38419492852932,2.03762694601121));
#12295=CARTESIAN_POINT('Ctrl Pts',(-4.38374462803762,4.26419452592647,2.04535203337753));
#12296=CARTESIAN_POINT('Ctrl Pts',(-4.49854935493777,4.13942982350094,2.05307712074384));
#12297=CARTESIAN_POINT('Ctrl Pts',(-4.61290891119671,4.01514891285017,2.06077225305352));
#12298=CARTESIAN_POINT('Ctrl Pts',(-4.72210143974045,3.88614083667116,2.0684673853632));
#12299=CARTESIAN_POINT('Ctrl Pts',(-4.82575071829774,3.75285965196526,2.07616251767288));
#12300=CARTESIAN_POINT('Ctrl Pts',(-4.9297990952227,3.61906527214603,2.08388727985347));
#12301=CARTESIAN_POINT('Ctrl Pts',(-5.02829827631538,3.48091740713,2.09161204203406));
#12302=CARTESIAN_POINT('Ctrl Pts',(-5.1208968980597,3.3388980999639,2.09933680421466));
#12303=CARTESIAN_POINT('Ctrl Pts',(-5.21347745671865,3.19690649630808,2.10706005953655));
#12304=CARTESIAN_POINT('Ctrl Pts',(-5.30015957972249,3.05104522270951,2.11478331485844));
#12305=CARTESIAN_POINT('Ctrl Pts',(-5.38063529168392,2.90182518777156,2.12250657018033));
#12306=CARTESIAN_POINT('Ctrl Pts',(-5.46111411365661,2.75259938617462,2.13023012397006));
#12307=CARTESIAN_POINT('Ctrl Pts',(-5.53538589071419,2.60001484055764,2.13795367775978));
#12308=CARTESIAN_POINT('Ctrl Pts',(-5.60318829787371,2.44460762926715,2.1456772315495));
#12309=CARTESIAN_POINT('Ctrl Pts',(-5.67098615111975,2.28921085582132,2.15340026659074));
#12310=CARTESIAN_POINT('Ctrl Pts',(-5.73231537725609,2.13099208660288,2.16112330163198));
#12311=CARTESIAN_POINT('Ctrl Pts',(-5.78696148603909,1.9705081379178,2.16884633667322));
#12312=CARTESIAN_POINT('Ctrl Pts',(-5.84162211737673,1.80998153959186,2.17657142416066));
#12313=CARTESIAN_POINT('Ctrl Pts',(-5.88959597802767,1.64718885840498,2.1842965116481));
#12314=CARTESIAN_POINT('Ctrl Pts',(-5.93071792276978,1.48270377454071,2.19202159913554));
#12315=CARTESIAN_POINT('Ctrl Pts',(-5.97168040787764,1.3188565187626,2.19971673085038));
#12316=CARTESIAN_POINT('Ctrl Pts',(-6.00584397787393,1.15333027300864,2.20741186256523));
#12317=CARTESIAN_POINT('Ctrl Pts',(-6.03309549633831,0.986703752178132,
2.21510699428008));
#12318=CARTESIAN_POINT('Ctrl Pts',(-6.06145111302405,0.81332633981401,2.22311389508957));
#12319=CARTESIAN_POINT('Ctrl Pts',(-6.08233074226667,0.63871365318621,2.23112079589906));
#12320=CARTESIAN_POINT('Ctrl Pts',(-6.09565353383094,0.463501410995017,
2.23912769670856));
#12321=CARTESIAN_POINT('Ctrl Pts',(-6.10737373709051,0.309365314056196,
2.24617145360543));
#12322=CARTESIAN_POINT('Ctrl Pts',(-6.1132465079406,0.154765470390503,2.25321521050231));
#12323=CARTESIAN_POINT('Ctrl Pts',(-6.11324999844244,0.000137998184036704,
2.26025896739919));
#12324=CARTESIAN_POINT('Ctrl Pts',(-6.11324999844246,0.000137997300213472,
2.26025896743945));
#12325=CARTESIAN_POINT('Ctrl Pts',(-6.11325387162186,-0.171442996720229,
2.26807500939343));
#12326=CARTESIAN_POINT('Ctrl Pts',(-6.1060295174546,-0.343034351920675,
2.27589105134742));
#12327=CARTESIAN_POINT('Ctrl Pts',(-6.09160170655671,-0.514017714845873,
2.2837070933014));
#12328=CARTESIAN_POINT('Ctrl Pts',(-6.07735174577439,-0.682893383743797,
2.2914267877239));
#12329=CARTESIAN_POINT('Ctrl Pts',(-6.05607496211486,-0.851175644165355,
2.2991464821464));
#12330=CARTESIAN_POINT('Ctrl Pts',(-6.02784749187544,-1.01827313486656,
2.30686617656889));
#12331=CARTESIAN_POINT('Ctrl Pts',(-5.99909157188228,-1.18849887712782,
2.31473039228862));
#12332=CARTESIAN_POINT('Ctrl Pts',(-5.96312217325259,-1.35749471095138,
2.32259460800834));
#12333=CARTESIAN_POINT('Ctrl Pts',(-5.92007454414292,-1.52464518963953,
2.33045882372807));
#12334=CARTESIAN_POINT('Ctrl Pts',(-5.87702691503326,-1.69179566832769,
2.3383230394478));
#12335=CARTESIAN_POINT('Ctrl Pts',(-5.82690115090709,-1.85710045725307,
2.34618725516752));
#12336=CARTESIAN_POINT('Ctrl Pts',(-5.76988658228266,-2.01995900703318,
2.35405147088725));
#12337=CARTESIAN_POINT('Ctrl Pts',(-5.71388303448856,-2.17992963903727,
2.36177623302347));
#12338=CARTESIAN_POINT('Ctrl Pts',(-5.65121266928852,-2.33759810852869,
2.36950099515969));
#12339=CARTESIAN_POINT('Ctrl Pts',(-5.58209000656017,-2.49240781598058,
2.37722575729591));
#12340=CARTESIAN_POINT('Ctrl Pts',(-5.51298082750083,-2.64718732490174,
2.3849490125727));
#12341=CARTESIAN_POINT('Ctrl Pts',(-5.4374219914878,-2.7991088952909,2.3926722678495));
#12342=CARTESIAN_POINT('Ctrl Pts',(-5.35567579798097,-2.94763673294741,
2.40039552312629));
#12343=CARTESIAN_POINT('Ctrl Pts',(-5.27392644537287,-3.09617031049787,
2.40811907687014));
#12344=CARTESIAN_POINT('Ctrl Pts',(-5.18598940613194,-3.2413096133189,2.41584263061399));
#12345=CARTESIAN_POINT('Ctrl Pts',(-5.09217288055155,-3.38254355730644,
2.42356618435784));
#12346=CARTESIAN_POINT('Ctrl Pts',(-4.99836265611334,-3.52376801538351,
2.43128921935289));
#12347=CARTESIAN_POINT('Ctrl Pts',(-4.89867391096325,-3.66108737552215,
2.43901225434793));
#12348=CARTESIAN_POINT('Ctrl Pts',(-4.79345820682571,-3.7940195020473,2.44673528934298));
#12349=CARTESIAN_POINT('Ctrl Pts',(-4.68821454093948,-3.92698695613828,
2.45446037678414));
#12350=CARTESIAN_POINT('Ctrl Pts',(-4.57744117611848,-4.05556459676049,
2.46218546422531));
#12351=CARTESIAN_POINT('Ctrl Pts',(-4.46153059924172,-4.17930260624064,
2.46991055166648));
#12352=CARTESIAN_POINT('Ctrl Pts',(-4.3460694877127,-4.30256079801168,2.47760568360913));
#12353=CARTESIAN_POINT('Ctrl Pts',(-4.22551117129597,-4.42101661930306,
2.48530081555179));
#12354=CARTESIAN_POINT('Ctrl Pts',(-4.10028056703834,-4.53426122252212,
2.49299594749444));
#12355=CARTESIAN_POINT('Ctrl Pts',(-3.97456776167407,-4.64794187468716,
2.5007207095835));
#12356=CARTESIAN_POINT('Ctrl Pts',(-3.84410207183109,-4.75641133750185,
2.50844547167256));
#12357=CARTESIAN_POINT('Ctrl Pts',(-3.70933816649836,-4.85928347897697,
2.51617023376162));
#12358=CARTESIAN_POINT('Ctrl Pts',(-3.57460054939822,-4.96213555330745,
2.52389348899064));
#12359=CARTESIAN_POINT('Ctrl Pts',(-3.43556664157642,-5.05939229277082,
2.53161674421967));
#12360=CARTESIAN_POINT('Ctrl Pts',(-3.29272311464412,-5.15070869422726,
2.5393399994487));
#12361=CARTESIAN_POINT('Ctrl Pts',(-3.14987406749818,-5.24202862462238,
2.54706355314431));
#12362=CARTESIAN_POINT('Ctrl Pts',(-3.00321537152376,-5.32740758360003,
2.55478710683992));
#12363=CARTESIAN_POINT('Ctrl Pts',(-2.85326218301945,-5.40654422690235,
2.56251066053553));
#12364=CARTESIAN_POINT('Ctrl Pts',(-2.70331906605275,-5.48567555502805,
2.57023369548217));
#12365=CARTESIAN_POINT('Ctrl Pts',(-2.55008217967926,-5.55856525856189,
2.57795673042881));
#12366=CARTESIAN_POINT('Ctrl Pts',(-2.39409090722725,-5.62495815899388,
2.58567976537545));
#12367=CARTESIAN_POINT('Ctrl Pts',(-2.2380581790894,-5.69136870376698,2.5934048527684));
#12368=CARTESIAN_POINT('Ctrl Pts',(-2.07926989313185,-5.75127886912873,
2.60112994016134));
#12369=CARTESIAN_POINT('Ctrl Pts',(-1.91828590825238,-5.80448143564094,
2.60885502755429));
#12370=CARTESIAN_POINT('Ctrl Pts',(-1.75792616345052,-5.85747770104641,
2.61655015973674));
#12371=CARTESIAN_POINT('Ctrl Pts',(-1.59538802431163,-5.90381822726308,
2.62424529191918));
#12372=CARTESIAN_POINT('Ctrl Pts',(-1.43124022628975,-5.94334728727424,
2.63194042410163));
#12373=CARTESIAN_POINT('Ctrl Pts',(-1.26646038104637,-5.98302855299787,
2.6396651862089));
#12374=CARTESIAN_POINT('Ctrl Pts',(-1.10000008925648,-6.01585981834215,
2.64738994831617));
#12375=CARTESIAN_POINT('Ctrl Pts',(-0.932443344467888,-6.04171953766952,
2.65511471042344));
#12376=CARTESIAN_POINT('Ctrl Pts',(-0.764919284766879,-6.06757421257333,
2.66283796567089));
#12377=CARTESIAN_POINT('Ctrl Pts',(-0.596299511869711,-6.08646000669851,
2.67056122091834));
#12378=CARTESIAN_POINT('Ctrl Pts',(-0.42717644441767,-6.09830680171428,
2.67828447616579));
#12379=CARTESIAN_POINT('Ctrl Pts',(-0.258046841170889,-6.11015405455181,
2.68600802987998));
#12380=CARTESIAN_POINT('Ctrl Pts',(-0.0884142203152118,-6.11496173784735,
2.69373158359417));
#12381=CARTESIAN_POINT('Ctrl Pts',(0.081124874046489,-6.11271169918155,
2.70145513730837));
#12382=CARTESIAN_POINT('Ctrl Pts',(0.250652581392769,-6.11046181163856,
2.70917817227362));
#12383=CARTESIAN_POINT('Ctrl Pts',(0.420086457886345,-6.10115515495588,
2.71690120723887));
#12384=CARTESIAN_POINT('Ctrl Pts',(0.588830772081147,-6.08482570698211,
2.72462424220413));
#12385=CARTESIAN_POINT('Ctrl Pts',(0.757619931163056,-6.06849191935248,
2.73234932961561));
#12386=CARTESIAN_POINT('Ctrl Pts',(0.925718845871653,-6.04513163938592,
2.74007441702709));
#12387=CARTESIAN_POINT('Ctrl Pts',(1.09253674965138,-6.01483075515523,2.74779950443857));
#12388=CARTESIAN_POINT('Ctrl Pts',(1.2587077890454,-5.9846473676825,2.75549463652866));
#12389=CARTESIAN_POINT('Ctrl Pts',(1.42360743311793,-5.94757719448578,2.76318976861874));
#12390=CARTESIAN_POINT('Ctrl Pts',(1.58666175608273,-5.90375558727531,2.77088490070882));
#12391=CARTESIAN_POINT('Ctrl Pts',(1.75034234718392,-5.85976566759215,2.77860958869135));
#12392=CARTESIAN_POINT('Ctrl Pts',(1.91222137634933,-5.80895673992962,2.78633427667389));
#12393=CARTESIAN_POINT('Ctrl Pts',(2.07172788897545,-5.75150146627307,2.79405896465642));
#12394=CARTESIAN_POINT('Ctrl Pts',(2.23121533170672,-5.69405306171553,2.80178272910935));
#12395=CARTESIAN_POINT('Ctrl Pts',(2.38833052483343,-5.62996000125963,2.80950649356227));
#12396=CARTESIAN_POINT('Ctrl Pts',(2.54251959434355,-5.55944418758558,2.81723025801519));
#12397=CARTESIAN_POINT('Ctrl Pts',(2.69668717969285,-5.48893819933616,2.82495294626603));
#12398=CARTESIAN_POINT('Ctrl Pts',(2.84792916754531,-5.41201137691455,2.83267563451688));
#12399=CARTESIAN_POINT('Ctrl Pts',(2.99571321128252,-5.32893309380474,2.84039832276772));
#12400=CARTESIAN_POINT('Ctrl Pts',(3.14351076533101,-5.24584721573789,2.84812171702118));
#12401=CARTESIAN_POINT('Ctrl Pts',(3.28784946631342,-5.1566089068414,2.85584511127464));
#12402=CARTESIAN_POINT('Ctrl Pts',(3.42822237126001,-5.06153306179979,2.8635685055281));
#12403=CARTESIAN_POINT('Ctrl Pts',(3.52853996042675,-4.99358704639039,2.86908803432881));
#12404=CARTESIAN_POINT('Ctrl Pts',(3.62683264091644,-4.92266060832901,2.87460756312952));
#12405=CARTESIAN_POINT('Ctrl Pts',(3.72292453512039,-4.84888218750453,2.88012709193022));
#12406=CARTESIAN_POINT('',(-6.11324999796762,0.0001576353973087,2.11474103256055));
#12407=CARTESIAN_POINT('Ctrl Pts',(-6.11324999796762,0.0001576353973087,
2.11474103256055));
#12408=CARTESIAN_POINT('Ctrl Pts',(-6.11325435310326,-0.168738649423157,
2.12243630998825));
#12409=CARTESIAN_POINT('Ctrl Pts',(-6.10625498998438,-0.337657948030418,
2.13013158741595));
#12410=CARTESIAN_POINT('Ctrl Pts',(-6.09227225641602,-0.506008217525845,
2.13782686484365));
#12411=CARTESIAN_POINT('Ctrl Pts',(-6.07828929035017,-0.674361286260356,
2.14552227022435));
#12412=CARTESIAN_POINT('Ctrl Pts',(-6.05732274391698,-0.84214498618751,
2.15321767560505));
#12413=CARTESIAN_POINT('Ctrl Pts',(-6.02944494908661,-1.00877111796181,
2.16091308098575));
#12414=CARTESIAN_POINT('Ctrl Pts',(-6.00156865647815,-1.17538827092607,
2.16860807169209));
#12415=CARTESIAN_POINT('Ctrl Pts',(-5.96678191434973,-1.3408476635067,2.17630306239844));
#12416=CARTESIAN_POINT('Ctrl Pts',(-5.92520844601766,-1.50456985007045,
2.18399805310479));
#12417=CARTESIAN_POINT('Ctrl Pts',(-5.88362467080505,-1.66833262658461,
2.19169495155069));
#12418=CARTESIAN_POINT('Ctrl Pts',(-5.83525088602938,-1.83035702456957,
2.19939184999659));
#12419=CARTESIAN_POINT('Ctrl Pts',(-5.78026131824623,-1.99007654508222,
2.20708874844249));
#12420=CARTESIAN_POINT('Ctrl Pts',(-5.74210347661473,-2.10090760658855,
2.21242970753332));
#12421=CARTESIAN_POINT('Ctrl Pts',(-5.7007611108435,-2.21062911917225,2.21777066662415));
#12422=CARTESIAN_POINT('Ctrl Pts',(-5.65630632717199,-2.31905676853632,
2.22311162571499));
#12423=CARTESIAN_POINT('Ctrl Pts',(-5.59201026082955,-2.47587839179245,
2.23083638853408));
#12424=CARTESIAN_POINT('Ctrl Pts',(-5.52117694864381,-2.6300522157125,2.23856115135317));
#12425=CARTESIAN_POINT('Ctrl Pts',(-5.44404973649907,-2.78103362601468,
2.24628591417226));
#12426=CARTESIAN_POINT('Ctrl Pts',(-5.36693756938016,-2.93198558472442,
2.25400917013984));
#12427=CARTESIAN_POINT('Ctrl Pts',(-5.28353409616438,-3.07974609033716,
2.26173242610742));
#12428=CARTESIAN_POINT('Ctrl Pts',(-5.19412928840774,-3.22379380510059,
2.269455682075));
#12429=CARTESIAN_POINT('Ctrl Pts',(-5.10472102551454,-3.36784708672936,
2.27717923651539));
#12430=CARTESIAN_POINT('Ctrl Pts',(-5.00931112773894,-3.5081870190292,2.28490279095577));
#12431=CARTESIAN_POINT('Ctrl Pts',(-4.90823411184662,-3.64431934190807,
2.29262634539616));
#12432=CARTESIAN_POINT('Ctrl Pts',(-4.80716388472028,-3.78044252155616,
2.3003493810895));
#12433=CARTESIAN_POINT('Ctrl Pts',(-4.70042749013053,-3.9123584028382,2.30807241678284));
#12434=CARTESIAN_POINT('Ctrl Pts',(-4.58840123239069,-4.03960390299539,
2.31579545247618));
#12435=CARTESIAN_POINT('Ctrl Pts',(-4.47634520301125,-4.16688321939573,
2.32352054061187));
#12436=CARTESIAN_POINT('Ctrl Pts',(-4.35899670926232,-4.28948943500712,
2.33124562874755));
#12437=CARTESIAN_POINT('Ctrl Pts',(-4.2367712337785,-4.40699388190261,2.33897071688324));
#12438=CARTESIAN_POINT('Ctrl Pts',(-4.11501977660236,-4.52404261971746,
2.34666584536288));
#12439=CARTESIAN_POINT('Ctrl Pts',(-3.98842934593239,-4.63602889699067,
2.35436097384253));
#12440=CARTESIAN_POINT('Ctrl Pts',(-3.85744566598918,-4.74256665703723,
2.36205610232218));
#12441=CARTESIAN_POINT('Ctrl Pts',(-3.72595757608652,-4.84951468733462,
2.36978086426033));
#12442=CARTESIAN_POINT('Ctrl Pts',(-3.58999574543703,-4.95101000774563,
2.37750562619848));
#12443=CARTESIAN_POINT('Ctrl Pts',(-3.45003442167379,-5.04669080207675,
2.38523038813663));
#12444=CARTESIAN_POINT('Ctrl Pts',(-3.31010040002098,-5.14235293205442,
2.39295364321347));
#12445=CARTESIAN_POINT('Ctrl Pts',(-3.16616870346133,-5.23220262040445,
2.40067689829031));
#12446=CARTESIAN_POINT('Ctrl Pts',(-3.01874338667934,-5.3159207977433,2.40840015336716));
#12447=CARTESIAN_POINT('Ctrl Pts',(-2.87131237262796,-5.39964221038134,
2.41612370691013));
#12448=CARTESIAN_POINT('Ctrl Pts',(-2.72038774181563,-5.47723147791105,
2.42384726045311));
#12449=CARTESIAN_POINT('Ctrl Pts',(-2.56649971049706,-5.54841462027835,
2.43157081399609));
#12450=CARTESIAN_POINT('Ctrl Pts',(-2.41262201499729,-5.61959298166265,
2.43929384879015));
#12451=CARTESIAN_POINT('Ctrl Pts',(-2.25578160496855,-5.68436594585324,
2.44701688358421));
#12452=CARTESIAN_POINT('Ctrl Pts',(-2.09653047525643,-5.74250690281005,
2.45473991837826));
#12453=CARTESIAN_POINT('Ctrl Pts',(-1.9372370234978,-5.80066331111272,2.46246500562017));
#12454=CARTESIAN_POINT('Ctrl Pts',(-1.77553186902071,-5.85218407946506,
2.47019009286207));
#12455=CARTESIAN_POINT('Ctrl Pts',(-1.61198494511743,-5.89689156244328,
2.47791518010397));
#12456=CARTESIAN_POINT('Ctrl Pts',(-1.44907218021927,-5.94142569056866,
2.48561031304577));
#12457=CARTESIAN_POINT('Ctrl Pts',(-1.28433221319907,-5.97919922568479,
2.49330544598756));
#12458=CARTESIAN_POINT('Ctrl Pts',(-1.11834114801678,-6.01008640862613,
2.50100057892936));
#12459=CARTESIAN_POINT('Ctrl Pts',(-0.951710955509462,-6.04109251870725,
2.50872534099443));
#12460=CARTESIAN_POINT('Ctrl Pts',(-0.783760990323875,-6.06517009324846,
2.51645010305951));
#12461=CARTESIAN_POINT('Ctrl Pts',(-0.615080805155099,-6.08222830594427,
2.52417486512458));
#12462=CARTESIAN_POINT('Ctrl Pts',(-0.446433524243184,-6.09928319111344,
2.53189812032887));
#12463=CARTESIAN_POINT('Ctrl Pts',(-0.27705662269999,-6.10932141473159,
2.53962137553317));
#12464=CARTESIAN_POINT('Ctrl Pts',(-0.107545376246114,-6.1123039481482,
2.54734463073746));
#12465=CARTESIAN_POINT('Ctrl Pts',(0.0619724209804701,-6.115286596825,2.55506818440743));
#12466=CARTESIAN_POINT('Ctrl Pts',(0.231624256707586,-6.11121300013985,
2.56279173807741));
#12467=CARTESIAN_POINT('Ctrl Pts',(0.400813454111122,-6.10009624001978,
2.57051529174738));
#12468=CARTESIAN_POINT('Ctrl Pts',(0.569991287989971,-6.08898022655246,
2.57823832666797));
#12469=CARTESIAN_POINT('Ctrl Pts',(0.738706229452274,-6.070822017091,2.58596136158855));
#12470=CARTESIAN_POINT('Ctrl Pts',(0.90636514052485,-6.04568670992315,2.59368439650914));
#12471=CARTESIAN_POINT('Ctrl Pts',(1.07406860802225,-6.02054472288712,2.6014094838755));
#12472=CARTESIAN_POINT('Ctrl Pts',(1.24071517036138,-5.98842197785238,2.60913457124187));
#12473=CARTESIAN_POINT('Ctrl Pts',(1.40571936345527,-5.94943515249195,2.61685965860824));
#12474=CARTESIAN_POINT('Ctrl Pts',(1.57008373077596,-5.91059950374839,2.62455479091768));
#12475=CARTESIAN_POINT('Ctrl Pts',(1.73281814681099,-5.86495301598595,2.63224992322712));
#12476=CARTESIAN_POINT('Ctrl Pts',(1.89335655291803,-5.81266088173242,2.63994505553656));
#12477=CARTESIAN_POINT('Ctrl Pts',(2.05793420996479,-5.75905304329604,2.64783380239074));
#12478=CARTESIAN_POINT('Ctrl Pts',(2.22026340992346,-5.69844132849409,2.65572254924493));
#12479=CARTESIAN_POINT('Ctrl Pts',(2.37974669582981,-5.6310417531916,2.66361129609911));
#12480=CARTESIAN_POINT('Ctrl Pts',(2.53588773868642,-5.56505465043022,2.67133472086832));
#12481=CARTESIAN_POINT('Ctrl Pts',(2.68930066551015,-5.49256150224778,2.67905814563753));
#12482=CARTESIAN_POINT('Ctrl Pts',(2.83944450143217,-5.4138138576965,2.68678157040674));
#12483=CARTESIAN_POINT('Ctrl Pts',(2.99440914407056,-5.33253778984085,2.69475297830341));
#12484=CARTESIAN_POINT('Ctrl Pts',(3.14589094439971,-5.2445990326299,2.70272438620009));
#12485=CARTESIAN_POINT('Ctrl Pts',(3.29332181854905,-5.15032590832549,2.71069579409676));
#12486=CARTESIAN_POINT('Ctrl Pts',(3.44075269269837,-5.05605278402109,2.71866720199343));
#12487=CARTESIAN_POINT('Ctrl Pts',(3.58413232802228,-4.95544549284129,2.7266386098901));
#12488=CARTESIAN_POINT('Ctrl Pts',(3.72292453512037,-4.84888218750454,2.73461001778677));
#12489=CARTESIAN_POINT('Ctrl Pts',(3.72318137141383,-4.84921626688776,0.984617815426764));
#12490=CARTESIAN_POINT('Ctrl Pts',(4.45925545347764,-4.2832330214638,1.02693048123701));
#12491=CARTESIAN_POINT('Ctrl Pts',(5.72853657905866,-2.74185888015094,1.11555797258299));
#12492=CARTESIAN_POINT('Ctrl Pts',(6.36790888585768,0.246115919908329,1.25050028946468));
#12493=CARTESIAN_POINT('Ctrl Pts',(5.47407798976948,3.26271229099702,1.38944476607187));
#12494=CARTESIAN_POINT('Ctrl Pts',(3.24595379495023,5.48403304914773,1.52838924267906));
#12495=CARTESIAN_POINT('Ctrl Pts',(0.22663497067087,6.36863119357982,1.66733371928624));
#12496=CARTESIAN_POINT('Ctrl Pts',(-2.84792533819912,5.70089041666575,1.80627819589343));
#12497=CARTESIAN_POINT('Ctrl Pts',(-5.22831028765922,3.64356976551659,1.94522267250062));
#12498=CARTESIAN_POINT('Ctrl Pts',(-6.04676335981403,1.4639066170294,2.04804361805632));
#12499=CARTESIAN_POINT('Ctrl Pts',(-6.11351535343457,0.223837879067313,
2.1045497380763));
#12500=CARTESIAN_POINT('Ctrl Pts',(-6.11328444993451,0.000157636285682099,
2.11474103256055));
#12501=CARTESIAN_POINT('Ctrl Pts',(3.87932907111019,-3.36622224230924,0.000294770375723887));
#12502=CARTESIAN_POINT('Ctrl Pts',(4.43916355178267,-2.72105483262093,0.0466153921027713));
#12503=CARTESIAN_POINT('Ctrl Pts',(5.23010367843801,-1.14675700997481,0.139250839365547));
#12504=CARTESIAN_POINT('Ctrl Pts',(5.1410027524235,1.49571158632152,0.278201112164053));
#12505=CARTESIAN_POINT('Ctrl Pts',(3.79898575529339,3.77284335683313,0.417145588771241));
#12506=CARTESIAN_POINT('Ctrl Pts',(1.53088506617911,5.13067232132384,0.556090065378428));
#12507=CARTESIAN_POINT('Ctrl Pts',(-1.11032056394027,5.23774955056566,0.695034541985614));
#12508=CARTESIAN_POINT('Ctrl Pts',(-3.48091084250257,4.06821920710838,0.833979018592801));
#12509=CARTESIAN_POINT('Ctrl Pts',(-5.0030251669043,1.90702749096064,0.972923495199987));
#12510=CARTESIAN_POINT('Ctrl Pts',(-5.30566909132792,-0.71897659277826,
1.11186797180717));
#12511=CARTESIAN_POINT('Ctrl Pts',(-4.31506488185325,-3.16974261036297,
1.25081244841436));
#12512=CARTESIAN_POINT('Ctrl Pts',(-2.27267468398946,-4.84788532362214,
1.38975692502155));
#12513=CARTESIAN_POINT('Ctrl Pts',(0.323675729076908,-5.3443695323507,1.52870140162873));
#12514=CARTESIAN_POINT('Ctrl Pts',(2.84113049893774,-4.53817403915035,1.66764587823592));
#12515=CARTESIAN_POINT('Ctrl Pts',(4.66606619309411,-2.62580938898832,1.80659035484311));
#12516=CARTESIAN_POINT('Ctrl Pts',(5.35365846228852,-0.073409129846628,
1.94553483145029));
#12517=CARTESIAN_POINT('Ctrl Pts',(4.73630836736869,2.49688425172971,2.08447930805749));
#12518=CARTESIAN_POINT('Ctrl Pts',(2.96449354959961,4.45856771298933,2.22342378466467));
#12519=CARTESIAN_POINT('Ctrl Pts',(0.470089995263518,5.33348509944276,2.36236826127186));
#12520=CARTESIAN_POINT('Ctrl Pts',(-2.13889696337894,4.90837730673373,2.50131273787904));
#12521=CARTESIAN_POINT('Ctrl Pts',(-4.22653251122924,3.28686338162061,2.64025721448623));
#12522=CARTESIAN_POINT('Ctrl Pts',(-5.28396010317908,0.864183778737327,
2.77920169109342));
#12523=CARTESIAN_POINT('Ctrl Pts',(-5.05343409817609,-1.76913871345001,
2.9181461677006));
#12524=CARTESIAN_POINT('Ctrl Pts',(-3.59114470180712,-3.97123755285457,
3.05709064430779));
#12525=CARTESIAN_POINT('Ctrl Pts',(-1.25352172162997,-5.20535601723436,
3.19603512091497));
#12526=CARTESIAN_POINT('Ctrl Pts',(1.38964440741605,-5.17068045735624,3.33497959752217));
#12527=CARTESIAN_POINT('Ctrl Pts',(3.69408778374435,-3.87566296496448,3.47392407412935));
#12528=CARTESIAN_POINT('Ctrl Pts',(5.09810542778582,-1.63596119111572,3.61286855073654));
#12529=CARTESIAN_POINT('Ctrl Pts',(5.25947114215003,1.0025025070482,3.75181302734373));
#12530=CARTESIAN_POINT('Ctrl Pts',(4.13885239060241,3.39660843497763,3.89075750395091));
#12531=CARTESIAN_POINT('Ctrl Pts',(2.00939751694447,4.96279856438097,4.0297019805581));
#12532=CARTESIAN_POINT('Ctrl Pts',(-0.609843560104704,5.31931751298505,
4.16864645716528));
#12533=CARTESIAN_POINT('Ctrl Pts',(-3.0804366173129,4.37926457506889,4.30759093377247));
#12534=CARTESIAN_POINT('Ctrl Pts',(-4.80018005773276,2.3717755764589,4.44653541037966));
#12535=CARTESIAN_POINT('Ctrl Pts',(-5.34989021890557,-0.213828476584512,
4.58547988698684));
#12536=CARTESIAN_POINT('Ctrl Pts',(-4.5955764640689,-2.74731231108447,4.72442436359404));
#12537=CARTESIAN_POINT('Ctrl Pts',(-2.72110110370615,-4.61114484213517,
4.86336884020122));
#12538=CARTESIAN_POINT('Ctrl Pts',(-0.183363363757842,-5.35102100991686,
5.00231331680841));
#12539=CARTESIAN_POINT('Ctrl Pts',(2.3990687908189,-4.78659763387935,5.14125779341559));
#12540=CARTESIAN_POINT('Ctrl Pts',(4.39673323028909,-3.0554516643881,5.28020227002279));
#12541=CARTESIAN_POINT('Ctrl Pts',(5.32270366296445,-0.579546105159232,
5.41914674662996));
#12542=CARTESIAN_POINT('Ctrl Pts',(4.95127684255042,2.03762253623294,5.55809122323716));
#12543=CARTESIAN_POINT('Ctrl Pts',(3.37298723555918,4.15812518817019,5.69703569984434));
#12544=CARTESIAN_POINT('Ctrl Pts',(0.97253944520539,5.26509401618431,5.83598017645153));
#12545=CARTESIAN_POINT('Ctrl Pts',(-1.66496268531579,5.08870781517731,5.97492465305872));
#12546=CARTESIAN_POINT('Ctrl Pts',(-3.89663384135399,3.67196033177855,6.1138691296659));
#12547=CARTESIAN_POINT('Ctrl Pts',(-5.17850911128188,1.36018063363326,6.2528136062731));
#12548=CARTESIAN_POINT('Ctrl Pts',(-5.19813423138016,-1.28314008755638,
6.39175808288028));
#12549=CARTESIAN_POINT('Ctrl Pts',(-3.95072562200224,-3.61369824852538,
6.53070255948746));
#12550=CARTESIAN_POINT('Ctrl Pts',(-1.74033637453994,-5.06342544876427,
6.66964703609465));
#12551=CARTESIAN_POINT('Ctrl Pts',(0.894256017555476,-5.27895388754308,
6.80859151270184));
#12552=CARTESIAN_POINT('Ctrl Pts',(3.31087548194349,-4.20774898429146,6.94753598930903));
#12553=CARTESIAN_POINT('Ctrl Pts',(4.92047636562735,-2.11091456649553,7.08648046591621));
#12554=CARTESIAN_POINT('Ctrl Pts',(5.33072201090579,0.500450611134641,7.2254249425234));
#12555=CARTESIAN_POINT('Ctrl Pts',(4.44161594850704,2.98983205844547,7.36436941913058));
#12556=CARTESIAN_POINT('Ctrl Pts',(2.46987581595201,4.75044854992828,7.50331389573778));
#12557=CARTESIAN_POINT('Ctrl Pts',(-0.103891087581167,5.35315370727028,
7.64225837234496));
#12558=CARTESIAN_POINT('Ctrl Pts',(-2.65233476814663,4.65103948052701,7.78120284895214));
#12559=CARTESIAN_POINT('Ctrl Pts',(-4.55427771142509,2.81524466058586,7.92014732555934));
#12560=CARTESIAN_POINT('Ctrl Pts',(-5.34612552885195,0.293240177154901,
8.05909180216652));
#12561=CARTESIAN_POINT('Ctrl Pts',(-4.83486706514864,-2.30024095130953,
8.19803627877371));
#12562=CARTESIAN_POINT('Ctrl Pts',(-3.14512044080958,-4.33304343210892,
8.33698075538089));
#12563=CARTESIAN_POINT('Ctrl Pts',(-0.688757660674787,-5.30967615364648,
8.47592523198808));
#12564=CARTESIAN_POINT('Ctrl Pts',(1.93548827689021,-4.99208704869627,8.61486970859527));
#12565=CARTESIAN_POINT('Ctrl Pts',(4.08796322496798,-3.45768775962346,8.75381418520246));
#12566=CARTESIAN_POINT('Ctrl Pts',(5.24400617257436,-1.08048472166078,8.89275866180964));
#12567=CARTESIAN_POINT('Ctrl Pts',(5.12183420642909,1.5600840790141,9.03170313841683));
#12568=CARTESIAN_POINT('Ctrl Pts',(3.75122647324369,3.82038583367911,9.17064761502402));
#12569=CARTESIAN_POINT('Ctrl Pts',(1.46626557853135,5.14947698557384,9.3095920916312));
#12570=CARTESIAN_POINT('Ctrl Pts',(-1.176094310065,5.22339450411064,9.4485365682384));
#12571=CARTESIAN_POINT('Ctrl Pts',(-3.53178381010122,4.02412115752588,9.58748104484557));
#12572=CARTESIAN_POINT('Ctrl Pts',(-5.02660881271791,1.84397717329882,9.72642552145276));
#12573=CARTESIAN_POINT('Ctrl Pts',(-5.29620902753513,-0.785632171181832,
9.86536999805996));
#12574=CARTESIAN_POINT('Ctrl Pts',(-4.27486999808783,-3.22374541041766,
10.0043144746671));
#12575=CARTESIAN_POINT('Ctrl Pts',(-2.21154085534078,-4.87607783130038,
10.1432589512744));
#12576=CARTESIAN_POINT('Ctrl Pts',(0.390846482732544,-5.33987705838589,
10.2822034278815));
#12577=CARTESIAN_POINT('Ctrl Pts',(2.89796585452676,-4.50209305520636,10.4211479044887));
#12578=CARTESIAN_POINT('Ctrl Pts',(4.69871245464655,-2.56693382078497,10.5600923810959));
#12579=CARTESIAN_POINT('Ctrl Pts',(5.3541582794983,-0.0060901412344418,
10.6990368577031));
#12580=CARTESIAN_POINT('Ctrl Pts',(4.70453985800457,2.55623799678097,10.8379813343103));
#12581=CARTESIAN_POINT('Ctrl Pts',(2.90820024455455,4.49548877312727,10.9769258109175));
#12582=CARTESIAN_POINT('Ctrl Pts',(0.402993249481863,5.33897409739104,11.1158702875246));
#12583=CARTESIAN_POINT('Ctrl Pts',(-2.20044245941706,4.88109628613643,11.2548147641319));
#12584=CARTESIAN_POINT('Ctrl Pts',(-4.26752518246539,3.23346204381065,11.393759240739));
#12585=CARTESIAN_POINT('Ctrl Pts',(-5.29440807478772,0.797678575218822,
11.5327037173462));
#12586=CARTESIAN_POINT('Ctrl Pts',(-5.03079070109704,-1.83253728297569,
11.6716481939534));
#12587=CARTESIAN_POINT('Ctrl Pts',(-3.54092921355771,-4.0160762288973,11.8105926705606));
#12588=CARTESIAN_POINT('Ctrl Pts',(-1.18797405672042,-5.22070547074815,
11.9495371471678));
#12589=CARTESIAN_POINT('Ctrl Pts',(1.4545471506665,-5.15279929341601,12.088481623775));
#12590=CARTESIAN_POINT('Ctrl Pts',(3.74252570506027,-3.8289096775327,12.2274261003821));
#12591=CARTESIAN_POINT('Ctrl Pts',(5.11827189094052,-1.57173179078,12.3663705769893));
#12592=CARTESIAN_POINT('Ctrl Pts',(5.24645061630721,1.06855224598058,12.5053150535965));
#12593=CARTESIAN_POINT('Ctrl Pts',(4.0958186001653,3.44837903460169,12.6442595302037));
#12594=CARTESIAN_POINT('Ctrl Pts',(1.94683985321038,4.98767105548193,12.7832040068109));
#12595=CARTESIAN_POINT('Ctrl Pts',(-0.676676804869458,5.31122928082493,
12.9221484834181));
#12596=CARTESIAN_POINT('Ctrl Pts',(-3.13525498741935,4.34018710836324,13.0610929600253));
#12597=CARTESIAN_POINT('Ctrl Pts',(-4.8296216966318,2.31123392134241,13.2000374366325));
#12598=CARTESIAN_POINT('Ctrl Pts',(-5.34677879219064,-0.281077425491243,
13.3389819132396));
#12599=CARTESIAN_POINT('Ctrl Pts',(-4.56067037512442,-2.80487677112613,
13.4779263898468));
#12600=CARTESIAN_POINT('Ctrl Pts',(-2.66290863455959,-4.64499360341092,
13.616870866454));
#12601=CARTESIAN_POINT('Ctrl Pts',(-0.116068800140973,-5.35290351168169,
13.7558153430612));
#12602=CARTESIAN_POINT('Ctrl Pts',(2.45906254776543,-4.75605502048891,13.8947598196684));
#12603=CARTESIAN_POINT('Ctrl Pts',(4.43480283491366,-2.99992863034811,14.0337042962756));
#12604=CARTESIAN_POINT('Ctrl Pts',(5.32956973328494,-0.51257626729447,14.1726487728828));
#12605=CARTESIAN_POINT('Ctrl Pts',(4.92526578910227,2.09971542796619,14.3115932494899));
#12606=CARTESIAN_POINT('Ctrl Pts',(3.3204391951282,4.20020612865568,14.4505377260972));
#12607=CARTESIAN_POINT('Ctrl Pts',(0.906262886499855,5.27690586919013,14.5894822027043));
#12608=CARTESIAN_POINT('Ctrl Pts',(-1.72881299760231,5.06737146764097,14.7284266793115));
#12609=CARTESIAN_POINT('Ctrl Pts',(-3.94249453472985,3.62267647125239,14.8673711559187));
#12610=CARTESIAN_POINT('Ctrl Pts',(-5.19520174310249,1.29496209218852,15.0063156325259));
#12611=CARTESIAN_POINT('Ctrl Pts',(-5.18159000953491,-1.34839643459491,
15.1452601091331));
#12612=CARTESIAN_POINT('Ctrl Pts',(-3.90497716399828,-3.663086310803,15.2842045857403));
#12613=CARTESIAN_POINT('Ctrl Pts',(-1.67653476589803,-5.08490699526312,
15.4231490623474));
#12614=CARTESIAN_POINT('Ctrl Pts',(0.960559275749421,-5.26729283878464,
15.5620935389546));
#12615=CARTESIAN_POINT('Ctrl Pts',(3.36351911705462,-4.16578769513627,15.7010380155618));
#12616=CARTESIAN_POINT('Ctrl Pts',(4.9466286079554,-2.04888100842811,15.839982492169));
#12617=CARTESIAN_POINT('Ctrl Pts',(5.3240083091875,0.567435895447707,15.9789269687762));
#12618=CARTESIAN_POINT('Ctrl Pts',(4.40367275269707,3.04544155401079,16.1178714453834));
#12619=CARTESIAN_POINT('Ctrl Pts',(2.40995169616313,4.78112756511432,16.2568159219906));
#12620=CARTESIAN_POINT('Ctrl Pts',(-0.171189759600305,5.35142429993724,
16.3957603985978));
#12621=CARTESIAN_POINT('Ctrl Pts',(-2.71060408984193,4.61732318988572,16.5347048752049));
#12622=CARTESIAN_POINT('Ctrl Pts',(-4.58931466442483,2.75775975796512,16.6736493518122));
#12623=CARTESIAN_POINT('Ctrl Pts',(-5.34938993330653,0.225998480494149,
16.8125938284193));
#12624=CARTESIAN_POINT('Ctrl Pts',(-4.8055632296837,-2.36084942704272,16.9515383050265));
#12625=CARTESIAN_POINT('Ctrl Pts',(-3.09039111055703,-4.37224550497758,
17.0904827816337));
#12626=CARTESIAN_POINT('Ctrl Pts',(-0.62194298890082,-5.31791640491889,
17.2294272582409));
#12627=CARTESIAN_POINT('Ctrl Pts',(1.99810236159196,-4.96735693557013,17.3683717348481));
#12628=CARTESIAN_POINT('Ctrl Pts',(4.13111467790414,-3.40601519205724,17.5073162114553));
#12629=CARTESIAN_POINT('Ctrl Pts',(5.25717692235762,-1.01446477468014,17.6462606880624));
#12630=CARTESIAN_POINT('Ctrl Pts',(5.10181391213023,1.62435919100904,17.7852051646696));
#12631=CARTESIAN_POINT('Ctrl Pts',(3.7028950369171,3.86724919076739,17.9241496412768));
#12632=CARTESIAN_POINT('Ctrl Pts',(1.4014036817988,5.16750575479613,18.063094117884));
#12633=CARTESIAN_POINT('Ctrl Pts',(-1.24167672489521,5.20819419957418,18.2020385944912));
#12634=CARTESIAN_POINT('Ctrl Pts',(-3.58210117112083,3.97939684585284,18.3409830710984));
#12635=CARTESIAN_POINT('Ctrl Pts',(-5.04939638077243,1.78063025560751,18.4799275477056));
#12636=CARTESIAN_POINT('Ctrl Pts',(-5.28591237076347,-0.852160923645241,
18.6188720243127));
#12637=CARTESIAN_POINT('Ctrl Pts',(-4.23399892837806,-3.27723995766688,
18.7578165009199));
#12638=CARTESIAN_POINT('Ctrl Pts',(-2.15005755740551,-4.90349861032466,
18.8967609775271));
#12639=CARTESIAN_POINT('Ctrl Pts',(0.457955496349907,-5.33454107110207,
19.0357054541343));
#12640=CARTESIAN_POINT('Ctrl Pts',(2.95434309566094,-4.4652994528204,19.1746499307415));
#12641=CARTESIAN_POINT('Ctrl Pts',(4.73061573122731,-2.50765387444491,19.3135944073487));
#12642=CARTESIAN_POINT('Ctrl Pts',(5.35381195296333,0.0612325072370531,
19.4525388839559));
#12643=CARTESIAN_POINT('Ctrl Pts',(4.67202694242282,2.61518238775666,19.591483360563));
#12644=CARTESIAN_POINT('Ctrl Pts',(2.85144844297689,4.53170934500242,19.7304278371702));
#12645=CARTESIAN_POINT('Ctrl Pts',(0.335830287665,5.34359898636174,19.8693723137774));
#12646=CARTESIAN_POINT('Ctrl Pts',(-2.261635153541,4.85308293633194,20.0083167903846));
#12647=CARTESIAN_POINT('Ctrl Pts',(-4.30785291211701,3.1794721341265,20.1472612669918));
#12648=CARTESIAN_POINT('Ctrl Pts',(-5.30399919630087,0.731201050000791,
20.286205743599));
#12649=CARTESIAN_POINT('Ctrl Pts',(-5.00739898838945,-1.89596936210377,
20.4251502202062));
#12650=CARTESIAN_POINT('Ctrl Pts',(-3.99577265594572,-3.33825103356245,
20.5177798712776));
#12651=CARTESIAN_POINT('Ctrl Pts',(-3.34807986563007,-3.89499774607468,
20.5640946968134));
#12652=CARTESIAN_POINT('Ctrl Pts',(4.12541174102849,-3.57975632042981,-0.187812896454475));
#12653=CARTESIAN_POINT('Ctrl Pts',(4.72075895114229,-2.89366314347346,-0.141492274727428));
#12654=CARTESIAN_POINT('Ctrl Pts',(5.56187184080512,-1.2195007812789,-0.0488568274646514));
#12655=CARTESIAN_POINT('Ctrl Pts',(5.46711885657024,1.59059106002505,0.0900934453338543));
#12656=CARTESIAN_POINT('Ctrl Pts',(4.03997190019308,4.01217117600349,0.229037921941041));
#12657=CARTESIAN_POINT('Ctrl Pts',(1.62799574627811,5.45613312141676,0.367982398548228));
#12658=CARTESIAN_POINT('Ctrl Pts',(-1.18075301342602,5.57000272376648,0.506926875155415));
#12659=CARTESIAN_POINT('Ctrl Pts',(-3.70172011600548,4.32628399768095,0.645871351762602));
#12660=CARTESIAN_POINT('Ctrl Pts',(-5.32038875431141,2.02799851661506,0.784815828369788));
#12661=CARTESIAN_POINT('Ctrl Pts',(-5.64223069560639,-0.76458439668364,
0.923760304976975));
#12662=CARTESIAN_POINT('Ctrl Pts',(-4.58878816429013,-3.37081313318115,
1.06270478158417));
#12663=CARTESIAN_POINT('Ctrl Pts',(-2.41684029712518,-5.15540771783689,
1.20164925819134));
#12664=CARTESIAN_POINT('Ctrl Pts',(0.344207884544761,-5.68338607346986,
1.34059373479854));
#12665=CARTESIAN_POINT('Ctrl Pts',(3.02135573014372,-4.82605010319058,1.47953821140572));
#12666=CARTESIAN_POINT('Ctrl Pts',(4.96205501120267,-2.79237586821557,1.61848268801291));
#12667=CARTESIAN_POINT('Ctrl Pts',(5.69326424052521,-0.0780657893714859,
1.75742716462009));
#12668=CARTESIAN_POINT('Ctrl Pts',(5.03675295127321,2.65527245027631,1.89637164122728));
#12669=CARTESIAN_POINT('Ctrl Pts',(3.15254423420737,4.74139400246158,2.03531611783446));
#12670=CARTESIAN_POINT('Ctrl Pts',(0.499909842720598,5.67181119377037,2.17426059444165));
#12671=CARTESIAN_POINT('Ctrl Pts',(-2.27457647542348,5.21973696982665,2.31320507104884));
#12672=CARTESIAN_POINT('Ctrl Pts',(-4.49463980138035,3.49536338298151,2.45214954765603));
#12673=CARTESIAN_POINT('Ctrl Pts',(-5.61914461217458,0.919002704297289,
2.59109402426322));
#12674=CARTESIAN_POINT('Ctrl Pts',(-5.37399534274702,-1.88136285584198,
2.7300385008704));
#12675=CARTESIAN_POINT('Ctrl Pts',(-3.81894658715497,-4.2231503764312,2.86898297747759));
#12676=CARTESIAN_POINT('Ctrl Pts',(-1.33303804169586,-5.53555432810611,
3.00792745408478));
#12677=CARTESIAN_POINT('Ctrl Pts',(1.47779557988571,-5.49867914705657,3.14687193069196));
#12678=CARTESIAN_POINT('Ctrl Pts',(3.92841979530433,-4.12151307786789,3.28581640729915));
#12679=CARTESIAN_POINT('Ctrl Pts',(5.42150036855981,-1.73973730559658,3.42476088390633));
#12680=CARTESIAN_POINT('Ctrl Pts',(5.59310221012439,1.06609558951481,3.56370536051352));
#12681=CARTESIAN_POINT('Ctrl Pts',(4.40139775038178,3.61207004110198,3.70264983712071));
#12682=CARTESIAN_POINT('Ctrl Pts',(2.1368623173862,5.27761040390352,3.8415943137279));
#12683=CARTESIAN_POINT('Ctrl Pts',(-0.64852858237328,5.65674489585048,3.98053879033508));
#12684=CARTESIAN_POINT('Ctrl Pts',(-3.27584207361916,4.65706032251836,4.11948326694227));
#12685=CARTESIAN_POINT('Ctrl Pts',(-5.10467630000627,2.52222758906297,4.25842774354946));
#12686=CARTESIAN_POINT('Ctrl Pts',(-5.6892569611194,-0.227392544354466,
4.39737222015664));
#12687=CARTESIAN_POINT('Ctrl Pts',(-4.88709381290986,-2.9215862476901,4.53631669676383));
#12688=CARTESIAN_POINT('Ctrl Pts',(-2.89371234973432,-4.90364976072612,
4.67526117337102));
#12689=CARTESIAN_POINT('Ctrl Pts',(-0.194994897276038,-5.69045948310944,
4.81420564997821));
#12690=CARTESIAN_POINT('Ctrl Pts',(2.55125213039659,-5.09023228409283,4.9531501265854));
#12691=CARTESIAN_POINT('Ctrl Pts',(4.67563709031104,-3.24927221675587,5.09209460319257));
#12692=CARTESIAN_POINT('Ctrl Pts',(5.66034584401081,-0.616309228442691,
5.23103907979977));
#12693=CARTESIAN_POINT('Ctrl Pts',(5.26535780928076,2.1668777720767,5.36998355640696));
#12694=CARTESIAN_POINT('Ctrl Pts',(3.58695044654535,4.42189310509675,5.50892803301416));
#12695=CARTESIAN_POINT('Ctrl Pts',(1.03423184069184,5.59908176744841,5.64787250962132));
#12696=CARTESIAN_POINT('Ctrl Pts',(-1.77057849037035,5.41150662462054,5.78681698622853));
#12697=CARTESIAN_POINT('Ctrl Pts',(-4.14381422790984,3.90488870308054,5.92576146283571));
#12698=CARTESIAN_POINT('Ctrl Pts',(-5.5070044064582,1.44646279113011,6.0647059394429));
#12699=CARTESIAN_POINT('Ctrl Pts',(-5.52787443305004,-1.36453522904529,
6.20365041605009));
#12700=CARTESIAN_POINT('Ctrl Pts',(-4.20133728483256,-3.8429308031696,6.34259489265727));
#12701=CARTESIAN_POINT('Ctrl Pts',(-1.85073345964212,-5.38462048804139,
6.48153936926446));
#12702=CARTESIAN_POINT('Ctrl Pts',(0.950982555664699,-5.61382083056589,
6.62048384587164));
#12703=CARTESIAN_POINT('Ctrl Pts',(3.52089867498252,-4.47466475385366,6.75942832247883));
#12704=CARTESIAN_POINT('Ctrl Pts',(5.23260352450663,-2.24481903372962,6.89837279908602));
#12705=CARTESIAN_POINT('Ctrl Pts',(5.66887283054235,0.532196364148326,7.0373172756932));
#12706=CARTESIAN_POINT('Ctrl Pts',(4.72336691402839,3.17949007457737,7.17626175230039));
#12707=CARTESIAN_POINT('Ctrl Pts',(2.6265507522657,5.05179010694687,7.31520622890758));
#12708=CARTESIAN_POINT('Ctrl Pts',(-0.110481349903347,5.69272746670676,
7.45415070551477));
#12709=CARTESIAN_POINT('Ctrl Pts',(-2.82058386723012,4.94607508907772,7.59309518212195));
#12710=CARTESIAN_POINT('Ctrl Pts',(-4.84317530124881,2.99382784078302,7.73203965872915));
#12711=CARTESIAN_POINT('Ctrl Pts',(-5.685253460446,0.311841673547404,7.87098413533632));
#12712=CARTESIAN_POINT('Ctrl Pts',(-5.14156365476053,-2.44615521235253,
8.00992861194351));
#12713=CARTESIAN_POINT('Ctrl Pts',(-3.34462907261211,-4.60790717197209,
8.1488730885507));
#12714=CARTESIAN_POINT('Ctrl Pts',(-0.732448546639514,-5.64649194326881,
8.28781756515788));
#12715=CARTESIAN_POINT('Ctrl Pts',(2.05826469364734,-5.30875678382038,8.42676204176508));
#12716=CARTESIAN_POINT('Ctrl Pts',(4.34728046423481,-3.67702389224715,8.56570651837225));
#12717=CARTESIAN_POINT('Ctrl Pts',(5.57665623044785,-1.14902455425511,8.70465099497944));
#12718=CARTESIAN_POINT('Ctrl Pts',(5.44673436655812,1.65904697915057,8.84359547158665));
#12719=CARTESIAN_POINT('Ctrl Pts',(3.98918303972281,4.06272947837557,8.98253994819381));
#12720=CARTESIAN_POINT('Ctrl Pts',(1.55927716423605,5.47613064708706,9.12148442480103));
#12721=CARTESIAN_POINT('Ctrl Pts',(-1.25069907356697,5.5547370744485,9.26042890140818));
#12722=CARTESIAN_POINT('Ctrl Pts',(-3.75582017660497,4.27938861753417,9.39937337801538));
#12723=CARTESIAN_POINT('Ctrl Pts',(-5.34546841307515,1.96094864381752,9.53831785462256));
#12724=CARTESIAN_POINT('Ctrl Pts',(-5.63217053893333,-0.835468227549896,
9.67726233122977));
#12725=CARTESIAN_POINT('Ctrl Pts',(-4.54604354469856,-3.4282415650853,9.81620680783694));
#12726=CARTESIAN_POINT('Ctrl Pts',(-2.35182848455184,-5.18538859856469,
9.95515128444412));
#12727=CARTESIAN_POINT('Ctrl Pts',(0.415639570463942,-5.67860862239497,
10.0940957610513));
#12728=CARTESIAN_POINT('Ctrl Pts',(3.0817963988662,-4.7876803459305,10.2330402376585));
#12729=CARTESIAN_POINT('Ctrl Pts',(4.99677216673147,-2.72976556734303,10.3719847142657));
#12730=CARTESIAN_POINT('Ctrl Pts',(5.69379576330861,-0.00647646530947798,
10.5109291908729));
#12731=CARTESIAN_POINT('Ctrl Pts',(5.00296922756137,2.71839126082836,10.6498736674801));
#12732=CARTESIAN_POINT('Ctrl Pts',(3.09268000064603,4.78065712559247,10.7888181440872));
#12733=CARTESIAN_POINT('Ctrl Pts',(0.428556859315862,5.67764838266755,10.9277626206944));
#12734=CARTESIAN_POINT('Ctrl Pts',(-2.34002606923442,5.19072539575898,11.0667070973016));
#12735=CARTESIAN_POINT('Ctrl Pts',(-4.53823281556239,3.43857456668117,11.2056515739088));
#12736=CARTESIAN_POINT('Ctrl Pts',(-5.63025534394137,0.848278787247312,
11.344596050516));
#12737=CARTESIAN_POINT('Ctrl Pts',(-5.34991557677349,-1.94878307162965,
11.4835405271232));
#12738=CARTESIAN_POINT('Ctrl Pts',(-3.76554571267171,-4.2708333641871,11.6224850037304));
#12739=CARTESIAN_POINT('Ctrl Pts',(-1.26333240408221,-5.55187746403591,
11.7614294803376));
#12740=CARTESIAN_POINT('Ctrl Pts',(1.546815385662,-5.47966370332645,11.9003739569447));
#12741=CARTESIAN_POINT('Ctrl Pts',(3.97993034407314,-4.07179402661772,12.0393184335519));
#12742=CARTESIAN_POINT('Ctrl Pts',(5.44294607794625,-1.67143355579679,12.1782629101591));
#12743=CARTESIAN_POINT('Ctrl Pts',(5.57925573584966,1.13633514988432,12.3172073867663));
#12744=CARTESIAN_POINT('Ctrl Pts',(4.35563413995431,3.66712467441981,12.4561518633735));
#12745=CARTESIAN_POINT('Ctrl Pts',(2.07033634969198,5.30406066500168,12.5950963399807));
#12746=CARTESIAN_POINT('Ctrl Pts',(-0.719601349748659,5.64814359204101,
12.7340408165879));
#12747=CARTESIAN_POINT('Ctrl Pts',(-3.33413781072106,4.61550400259756,12.872985293195));
#12748=CARTESIAN_POINT('Ctrl Pts',(-5.13598554976642,2.45784551415759,13.0119297698022));
#12749=CARTESIAN_POINT('Ctrl Pts',(-5.68594816311183,-0.298907385788696,
13.1508742464094));
#12750=CARTESIAN_POINT('Ctrl Pts',(-4.84997347933535,-2.98280227112322,
13.2898187230166));
#12751=CARTESIAN_POINT('Ctrl Pts',(-2.83182847985474,-4.93964569575163,
13.4287631996238));
#12752=CARTESIAN_POINT('Ctrl Pts',(-0.123431547592747,-5.69246140012673,
13.567707676231));
#12753=CARTESIAN_POINT('Ctrl Pts',(2.61505155157454,-5.05775222025373,13.7066521528382));
#12754=CARTESIAN_POINT('Ctrl Pts',(4.71612161508726,-3.19022711583059,13.8455966294454));
#12755=CARTESIAN_POINT('Ctrl Pts',(5.66764745895392,-0.54509120327449,13.9845411060525));
#12756=CARTESIAN_POINT('Ctrl Pts',(5.23769676188712,2.23290948526608,14.1234855826597));
#12757=CARTESIAN_POINT('Ctrl Pts',(3.53106905597799,4.46664342216709,14.2624300592669));
#12758=CARTESIAN_POINT('Ctrl Pts',(0.963751072387092,5.61164289752535,14.4013745358741));
#12759=CARTESIAN_POINT('Ctrl Pts',(-1.83847910492166,5.38881682001165,14.5403190124813));
#12760=CARTESIAN_POINT('Ctrl Pts',(-4.1925840639914,3.85247855350803,14.6792634890885));
#12761=CARTESIAN_POINT('Ctrl Pts',(-5.52475592432099,1.37710715471025,14.8182079656957));
#12762=CARTESIAN_POINT('Ctrl Pts',(-5.5102807394511,-1.43393106923174,14.9571524423028));
#12763=CARTESIAN_POINT('Ctrl Pts',(-4.15268680369936,-3.89545176446264,
15.0960969189101));
#12764=CARTESIAN_POINT('Ctrl Pts',(-1.78288463821885,-5.4074647022128,15.2350413955172));
#12765=CARTESIAN_POINT('Ctrl Pts',(1.02149171712221,-5.60142007090385,15.3739858721244));
#12766=CARTESIAN_POINT('Ctrl Pts',(3.57688172421524,-4.43004167811651,15.5129303487316));
#12767=CARTESIAN_POINT('Ctrl Pts',(5.26041471700324,-2.17885041799783,15.6518748253388));
#12768=CARTESIAN_POINT('Ctrl Pts',(5.66173324960281,0.603430815600041,15.790819301946));
#12769=CARTESIAN_POINT('Ctrl Pts',(4.68301681672617,3.23862712165757,15.9297637785531));
#12770=CARTESIAN_POINT('Ctrl Pts',(2.56282538563238,5.08441522513913,16.0687082551604));
#12771=CARTESIAN_POINT('Ctrl Pts',(-0.18204906860269,5.6908883555651,16.2076527317675));
#12772=CARTESIAN_POINT('Ctrl Pts',(-2.88254946474894,4.91022002787362,16.3465972083747));
#12773=CARTESIAN_POINT('Ctrl Pts',(-4.88043480015326,2.93269642144313,16.4855416849819));
#12774=CARTESIAN_POINT('Ctrl Pts',(-5.68872494023477,0.24033454440057,16.6244861615891));
#12775=CARTESIAN_POINT('Ctrl Pts',(-5.11040094990405,-2.51060834659618,
16.7634306381963));
#12776=CARTESIAN_POINT('Ctrl Pts',(-3.28642802354827,-4.64959600236532,
16.9023751148035));
#12777=CARTESIAN_POINT('Ctrl Pts',(-0.661395530420292,-5.65525490942225,
17.0413195914106));
#12778=CARTESIAN_POINT('Ctrl Pts',(2.12485066133594,-5.28245793234956,17.1802640680179));
#12779=CARTESIAN_POINT('Ctrl Pts',(4.39316920100402,-3.6220735095858,17.319208544625));
#12780=CARTESIAN_POINT('Ctrl Pts',(5.59066245801917,-1.07881667567005,17.4581530212322));
#12781=CARTESIAN_POINT('Ctrl Pts',(5.42544409815205,1.72739934029841,17.5970974978394));
#12782=CARTESIAN_POINT('Ctrl Pts',(3.93778573074807,4.11256558147797,17.7360419744466));
#12783=CARTESIAN_POINT('Ctrl Pts',(1.49030079604946,5.49530305934251,17.8749864510538));
#12784=CARTESIAN_POINT('Ctrl Pts',(-1.32044166543948,5.53857254866263,18.0139309276609));
#12785=CARTESIAN_POINT('Ctrl Pts',(-3.80932938609013,4.231827248776,18.1528754042682));
#12786=CARTESIAN_POINT('Ctrl Pts',(-5.36970149541447,1.89358335636413,18.2918198808753));
#12787=CARTESIAN_POINT('Ctrl Pts',(-5.62122072056,-0.906217187356495,18.4307643574825));
#12788=CARTESIAN_POINT('Ctrl Pts',(-4.50257984575516,-3.48512950350393,
18.5697088340897));
#12789=CARTESIAN_POINT('Ctrl Pts',(-2.28644503433923,-5.21454879654256,
18.7086533106969));
#12790=CARTESIAN_POINT('Ctrl Pts',(0.48700559990642,-5.67293415029241,18.8475977873041));
#12791=CARTESIAN_POINT('Ctrl Pts',(3.14174989294686,-4.74855276574965,18.9865422639113));
#12792=CARTESIAN_POINT('Ctrl Pts',(5.03069920652907,-2.66672523687453,19.1254867405184));
#12793=CARTESIAN_POINT('Ctrl Pts',(5.69342746777932,0.0651167507725929,
19.2644312171257));
#12794=CARTESIAN_POINT('Ctrl Pts',(4.96839387671658,2.78107475020022,19.4033756937328));
#12795=CARTESIAN_POINT('Ctrl Pts',(3.03232818612828,4.81917532545164,19.5423201703401));
#12796=CARTESIAN_POINT('Ctrl Pts',(0.357133459505582,5.68256664840653,19.6812646469472));
#12797=CARTESIAN_POINT('Ctrl Pts',(-2.40510048137543,5.16093503766596,19.8202091235544));
#12798=CARTESIAN_POINT('Ctrl Pts',(-4.58111870803096,3.38115984283969,19.9591536001616));
#12799=CARTESIAN_POINT('Ctrl Pts',(-5.64045487189444,0.777584304252472,
20.0980980767688));
#12800=CARTESIAN_POINT('Ctrl Pts',(-5.32504002626521,-2.01623892267917,
20.237042553376));
#12801=CARTESIAN_POINT('Ctrl Pts',(-4.24924184753463,-3.55001077658457,
20.3296722044474));
#12802=CARTESIAN_POINT('Ctrl Pts',(-3.56046309410368,-4.14207434801025,
20.3759870299831));
#12803=CARTESIAN_POINT('Ctrl Pts',(4.37149441094678,-3.79329039855036,-0.375920563284674));
#12804=CARTESIAN_POINT('Ctrl Pts',(5.0023543505019,-3.06627145432599,-0.329599941557627));
#12805=CARTESIAN_POINT('Ctrl Pts',(5.8936400031722,-1.29224455258298,-0.23696449429485));
#12806=CARTESIAN_POINT('Ctrl Pts',(5.79323496071699,1.68547053372857,-0.0980142214963448));
#12807=CARTESIAN_POINT('Ctrl Pts',(4.28095804509276,4.25149899517385,0.0409302551108422));
#12808=CARTESIAN_POINT('Ctrl Pts',(1.72510642637714,5.78159392150968,0.179874731718029));
#12809=CARTESIAN_POINT('Ctrl Pts',(-1.25118546291179,5.90225589696729,0.318819208325216));
#12810=CARTESIAN_POINT('Ctrl Pts',(-3.92252938950839,4.5843487882535,0.457763684932403));
#12811=CARTESIAN_POINT('Ctrl Pts',(-5.63775234171852,2.14896954226947,0.596708161539589));
#12812=CARTESIAN_POINT('Ctrl Pts',(-5.97879229988485,-0.810192200589017,
0.735652638146776));
#12813=CARTESIAN_POINT('Ctrl Pts',(-4.86251144672701,-3.57188365599933,
0.874597114753963));
#12814=CARTESIAN_POINT('Ctrl Pts',(-2.5610059102609,-5.46293011205162,1.01354159136115));
#12815=CARTESIAN_POINT('Ctrl Pts',(0.364740040012614,-6.02240261458903,
1.15248606796834));
#12816=CARTESIAN_POINT('Ctrl Pts',(3.20158096134969,-5.11392616723079,1.29143054457553));
#12817=CARTESIAN_POINT('Ctrl Pts',(5.25804382931122,-2.95894234744282,1.43037502118271));
#12818=CARTESIAN_POINT('Ctrl Pts',(6.0328700187619,-0.0827224488963419,
1.5693194977899));
#12819=CARTESIAN_POINT('Ctrl Pts',(5.33719753517774,2.81366064882291,1.70826397439709));
#12820=CARTESIAN_POINT('Ctrl Pts',(3.34059491881512,5.02422029193383,1.84720845100427));
#12821=CARTESIAN_POINT('Ctrl Pts',(0.529729690177678,6.01013728809799,1.98615292761146));
#12822=CARTESIAN_POINT('Ctrl Pts',(-2.41025598746802,5.53109663291954,2.12509740421865));
#12823=CARTESIAN_POINT('Ctrl Pts',(-4.76274709153145,3.70386338434242,2.26404188082583));
#12824=CARTESIAN_POINT('Ctrl Pts',(-5.95432912117008,0.973821629857239,
2.40298635743302));
#12825=CARTESIAN_POINT('Ctrl Pts',(-5.69455658731797,-1.99358699823395,
2.5419308340402));
#12826=CARTESIAN_POINT('Ctrl Pts',(-4.04674847250281,-4.47506320000782,
2.6808753106474));
#12827=CARTESIAN_POINT('Ctrl Pts',(-1.41255436176173,-5.86575263897786,
2.81981978725458));
#12828=CARTESIAN_POINT('Ctrl Pts',(1.56594675235535,-5.8266778367569,2.95876426386177));
#12829=CARTESIAN_POINT('Ctrl Pts',(4.1627518068643,-4.3673631907713,3.09770874046896));
#12830=CARTESIAN_POINT('Ctrl Pts',(5.74489530933378,-1.84351342007744,3.23665321707614));
#12831=CARTESIAN_POINT('Ctrl Pts',(5.92673327809876,1.12968867198141,3.37559769368333));
#12832=CARTESIAN_POINT('Ctrl Pts',(4.66394311016112,3.82753164722633,3.51454217029051));
#12833=CARTESIAN_POINT('Ctrl Pts',(2.26432711782793,5.59242224342607,3.65348664689771));
#12834=CARTESIAN_POINT('Ctrl Pts',(-0.68721360464186,5.99417227871591,3.79243112350489));
#12835=CARTESIAN_POINT('Ctrl Pts',(-3.47124752992542,4.93485606996784,3.93137560011208));
#12836=CARTESIAN_POINT('Ctrl Pts',(-5.40917254227977,2.67267960166704,4.07032007671926));
#12837=CARTESIAN_POINT('Ctrl Pts',(-6.02862370333322,-0.240956612124415,
4.20926455332645));
#12838=CARTESIAN_POINT('Ctrl Pts',(-5.17861116175084,-3.09586018429574,
4.34820902993364));
#12839=CARTESIAN_POINT('Ctrl Pts',(-3.06632359576249,-5.19615467931707,
4.48715350654083));
#12840=CARTESIAN_POINT('Ctrl Pts',(-0.206626430794233,-6.029897956302,4.626097983148));
#12841=CARTESIAN_POINT('Ctrl Pts',(2.70343546997428,-5.39386693430633,4.76504245975521));
#12842=CARTESIAN_POINT('Ctrl Pts',(4.95454095033299,-3.44309276912364,4.90398693636238));
#12843=CARTESIAN_POINT('Ctrl Pts',(5.99798802505716,-0.653072351726153,
5.04293141296958));
#12844=CARTESIAN_POINT('Ctrl Pts',(5.5794387760111,2.29613300792046,5.18187588957675));
#12845=CARTESIAN_POINT('Ctrl Pts',(3.80091365753151,4.6856610220233,5.32082036618396));
#12846=CARTESIAN_POINT('Ctrl Pts',(1.09592423617828,5.93306951871249,5.45976484279112));
#12847=CARTESIAN_POINT('Ctrl Pts',(-1.8761942954249,5.73430543406377,5.59870931939833));
#12848=CARTESIAN_POINT('Ctrl Pts',(-4.39099461446568,4.13781707438252,5.73765379600551));
#12849=CARTESIAN_POINT('Ctrl Pts',(-5.83549970163454,1.53274494862695,5.87659827261269));
#12850=CARTESIAN_POINT('Ctrl Pts',(-5.85761463471991,-1.4459303705342,6.01554274921988));
#12851=CARTESIAN_POINT('Ctrl Pts',(-4.45194894766288,-4.07216335781382,
6.15448722582707));
#12852=CARTESIAN_POINT('Ctrl Pts',(-1.9611305447443,-5.70581552731852,6.29343170243426));
#12853=CARTESIAN_POINT('Ctrl Pts',(1.00770909377392,-5.94868777358868,6.43237617904144));
#12854=CARTESIAN_POINT('Ctrl Pts',(3.73092186802155,-4.74158052341587,6.57132065564863));
#12855=CARTESIAN_POINT('Ctrl Pts',(5.54473068338591,-2.37872350096367,6.71026513225582));
#12856=CARTESIAN_POINT('Ctrl Pts',(6.00702365017893,0.563942117162005,6.849209608863));
#12857=CARTESIAN_POINT('Ctrl Pts',(5.00511787954972,3.36914809070927,6.98815408547019));
#12858=CARTESIAN_POINT('Ctrl Pts',(2.78322568857942,5.35313166396547,7.12709856207738));
#12859=CARTESIAN_POINT('Ctrl Pts',(-0.117071612225535,6.03230122614323,
7.26604303868457));
#12860=CARTESIAN_POINT('Ctrl Pts',(-2.98883296631359,5.24111069762843,7.40498751529175));
#12861=CARTESIAN_POINT('Ctrl Pts',(-5.13207289107254,3.17241102098019,7.54393199189894));
#12862=CARTESIAN_POINT('Ctrl Pts',(-6.02438139204003,0.330443169939912,
7.68287646850613));
#12863=CARTESIAN_POINT('Ctrl Pts',(-5.44826024437244,-2.59206947339553,
7.82182094511331));
#12864=CARTESIAN_POINT('Ctrl Pts',(-3.54413770441465,-4.88277091183526,
7.96076542172051));
#12865=CARTESIAN_POINT('Ctrl Pts',(-0.776139432604244,-5.98330773289114,
8.09970989832767));
#12866=CARTESIAN_POINT('Ctrl Pts',(2.18104111040448,-5.62542651894447,8.23865437493489));
#12867=CARTESIAN_POINT('Ctrl Pts',(4.60659770350166,-3.89636002487083,8.37759885154205));
#12868=CARTESIAN_POINT('Ctrl Pts',(5.90930628832132,-1.21756438684943,8.51654332814926));
#12869=CARTESIAN_POINT('Ctrl Pts',(5.77163452668715,1.75800987928705,8.65548780475643));
#12870=CARTESIAN_POINT('Ctrl Pts',(4.22713960620191,4.30507312307204,8.79443228136362));
#12871=CARTESIAN_POINT('Ctrl Pts',(1.65228874994075,5.80278430860025,8.93337675797081));
#12872=CARTESIAN_POINT('Ctrl Pts',(-1.32530383706894,5.88607964478638,9.07232123457799));
#12873=CARTESIAN_POINT('Ctrl Pts',(-3.97985654310871,4.53465607754247,9.21126571118519));
#12874=CARTESIAN_POINT('Ctrl Pts',(-5.6643280134324,2.07792011433624,9.35021018779235));
#12875=CARTESIAN_POINT('Ctrl Pts',(-5.96813205033154,-0.885304283917966,
9.48915466439957));
#12876=CARTESIAN_POINT('Ctrl Pts',(-4.81721709130929,-3.63273771975294,
9.62809914100673));
#12877=CARTESIAN_POINT('Ctrl Pts',(-2.49211611376292,-5.49469936582898,
9.76704361761394));
#12878=CARTESIAN_POINT('Ctrl Pts',(0.44043265819534,-6.01734018640404,9.90598809422111));
#12879=CARTESIAN_POINT('Ctrl Pts',(3.26562694320564,-5.07326763665466,10.0449325708283));
#12880=CARTESIAN_POINT('Ctrl Pts',(5.2948318788164,-2.89259731390109,10.1838770474355));
#12881=CARTESIAN_POINT('Ctrl Pts',(6.03343324711893,-0.00686278938451319,
10.3228215240426));
#12882=CARTESIAN_POINT('Ctrl Pts',(5.30139859711817,2.88054452487575,10.4617660006498));
#12883=CARTESIAN_POINT('Ctrl Pts',(3.27715975673751,5.06582547805768,10.600710477257));
#12884=CARTESIAN_POINT('Ctrl Pts',(0.454120469149858,6.01632266794404,10.7396549538642));
#12885=CARTESIAN_POINT('Ctrl Pts',(-2.47960967905176,5.50035450538153,10.8785994304714));
#12886=CARTESIAN_POINT('Ctrl Pts',(-4.8089404486594,3.64368708955169,11.0175439070786));
#12887=CARTESIAN_POINT('Ctrl Pts',(-5.96610261309502,0.898878999275805,
11.1564883836858));
#12888=CARTESIAN_POINT('Ctrl Pts',(-5.66904045244993,-2.06502886028363,
11.2954328602929));
#12889=CARTESIAN_POINT('Ctrl Pts',(-3.99016221178573,-4.52559049947687,
11.4343773369001));
#12890=CARTESIAN_POINT('Ctrl Pts',(-1.33869075144399,-5.88304945732368,
11.5733218135073));
#12891=CARTESIAN_POINT('Ctrl Pts',(1.63908362065749,-5.80652811323691,11.7122662901145));
#12892=CARTESIAN_POINT('Ctrl Pts',(4.21733498308602,-4.31467837570276,11.8512107667217));
#12893=CARTESIAN_POINT('Ctrl Pts',(5.76762026495197,-1.77113532081357,11.9901552433289));
#12894=CARTESIAN_POINT('Ctrl Pts',(5.91206085539211,1.20411805378807,12.1290997199361));
#12895=CARTESIAN_POINT('Ctrl Pts',(4.61544967974331,3.88587031423793,12.2680441965433));
#12896=CARTESIAN_POINT('Ctrl Pts',(2.19383284617359,5.62045027452143,12.4069886731505));
#12897=CARTESIAN_POINT('Ctrl Pts',(-0.762525894627859,5.98505790325709,
12.5459331497576));
#12898=CARTESIAN_POINT('Ctrl Pts',(-3.53302063402278,4.89082089683188,12.6848776263648));
#12899=CARTESIAN_POINT('Ctrl Pts',(-5.44234940290103,2.60445710697275,12.823822102972));
#12900=CARTESIAN_POINT('Ctrl Pts',(-6.02511753403304,-0.316737346086145,
12.9627665795792));
#12901=CARTESIAN_POINT('Ctrl Pts',(-5.13927658354627,-3.16072777112031,
13.1017110561864));
#12902=CARTESIAN_POINT('Ctrl Pts',(-3.00074832514988,-5.23429778809233,
13.2406555327936));
#12903=CARTESIAN_POINT('Ctrl Pts',(-0.130794295044517,-6.03201928857177,
13.3796000094008));
#12904=CARTESIAN_POINT('Ctrl Pts',(2.77104055538365,-5.35944942001855,13.5185444860079));
#12905=CARTESIAN_POINT('Ctrl Pts',(4.99744039526088,-3.38052560131306,13.6574889626151));
#12906=CARTESIAN_POINT('Ctrl Pts',(6.00572518462289,-0.577606139254506,
13.7964334392223));
#12907=CARTESIAN_POINT('Ctrl Pts',(5.55012773467197,2.36610354256596,13.9353779158295));
#12908=CARTESIAN_POINT('Ctrl Pts',(3.74169891682778,4.73308071567851,14.0743223924367));
#12909=CARTESIAN_POINT('Ctrl Pts',(1.02123925827433,5.94637992586056,14.2132668690439));
#12910=CARTESIAN_POINT('Ctrl Pts',(-1.948145212241,5.71026217238234,14.3522113456511));
#12911=CARTESIAN_POINT('Ctrl Pts',(-4.44267359325295,4.08228063576368,14.4911558222582));
#12912=CARTESIAN_POINT('Ctrl Pts',(-5.85431010553948,1.45925221723197,14.6301002988654));
#12913=CARTESIAN_POINT('Ctrl Pts',(-5.8389714693673,-1.51946570386857,14.7690447754726));
#12914=CARTESIAN_POINT('Ctrl Pts',(-4.40039644340045,-4.12781721812228,
14.9079892520798));
#12915=CARTESIAN_POINT('Ctrl Pts',(-1.88923451053967,-5.73002240916248,
15.046933728687));
#12916=CARTESIAN_POINT('Ctrl Pts',(1.08242415849501,-5.93554730302306,15.1858782052942));
#12917=CARTESIAN_POINT('Ctrl Pts',(3.79024433137585,-4.69429566109675,15.3248226819014));
#12918=CARTESIAN_POINT('Ctrl Pts',(5.57420082605109,-2.30881982756756,15.4637671585085));
#12919=CARTESIAN_POINT('Ctrl Pts',(5.9994581900181,0.63942573575238,15.6027116351158));
#12920=CARTESIAN_POINT('Ctrl Pts',(4.96236088075527,3.43181268930434,15.7416561117229));
#12921=CARTESIAN_POINT('Ctrl Pts',(2.71569907510162,5.38770288516396,15.8806005883301));
#12922=CARTESIAN_POINT('Ctrl Pts',(-0.192908377605067,6.03035241119298,
16.0195450649373));
#12923=CARTESIAN_POINT('Ctrl Pts',(-3.05449483965596,5.20311686586152,16.1584895415445));
#12924=CARTESIAN_POINT('Ctrl Pts',(-5.17155493588167,3.10763308492114,16.2974340181517));
#12925=CARTESIAN_POINT('Ctrl Pts',(-6.02805994716301,0.254670608306993,
16.4363784947589));
#12926=CARTESIAN_POINT('Ctrl Pts',(-5.41523867012438,-2.66036726614962,
16.5753229713661));
#12927=CARTESIAN_POINT('Ctrl Pts',(-3.48246493653952,-4.92694649975305,
16.7142674479732));
#12928=CARTESIAN_POINT('Ctrl Pts',(-0.700848071939763,-5.99259341392561,
16.8532119245804));
#12929=CARTESIAN_POINT('Ctrl Pts',(2.25159896107991,-5.59755892912898,16.9921564011876));
#12930=CARTESIAN_POINT('Ctrl Pts',(4.65522372410391,-3.83813182711437,17.1311008777948));
#12931=CARTESIAN_POINT('Ctrl Pts',(5.92414799368071,-1.14316857665995,17.270045354402));
#12932=CARTESIAN_POINT('Ctrl Pts',(5.74907428417388,1.83043948958779,17.4089898310092));
#12933=CARTESIAN_POINT('Ctrl Pts',(4.17267642457904,4.35788197218855,17.5479343076163));
#12934=CARTESIAN_POINT('Ctrl Pts',(1.57919791030011,5.82310036388892,17.6868787842236));
#12935=CARTESIAN_POINT('Ctrl Pts',(-1.39920660598374,5.86895089775106,17.8258232608307));
#12936=CARTESIAN_POINT('Ctrl Pts',(-4.03655760105942,4.48425765169917,17.9647677374379));
#12937=CARTESIAN_POINT('Ctrl Pts',(-5.69000661005654,2.00653645712075,18.1037122140451));
#12938=CARTESIAN_POINT('Ctrl Pts',(-5.9565290703565,-0.960273451067746,
18.2426566906523));
#12939=CARTESIAN_POINT('Ctrl Pts',(-4.77116076313227,-3.69301904934098,
18.3816011672595));
#12940=CARTESIAN_POINT('Ctrl Pts',(-2.42283251127295,-5.52559898276046,
18.5205456438667));
#12941=CARTESIAN_POINT('Ctrl Pts',(0.516055703462933,-6.01132722948276,
18.6594901204738));
#12942=CARTESIAN_POINT('Ctrl Pts',(3.32915669023277,-5.03180607867891,18.7984345970811));
#12943=CARTESIAN_POINT('Ctrl Pts',(5.33078268183083,-2.82579659930416,18.9373790736882));
#12944=CARTESIAN_POINT('Ctrl Pts',(6.03304298259528,0.0690009943081289,
19.0763235502954));
#12945=CARTESIAN_POINT('Ctrl Pts',(5.26476081101034,2.94696711264378,19.2152680269026));
#12946=CARTESIAN_POINT('Ctrl Pts',(3.21320792927966,5.10664130590087,19.3542125035098));
#12947=CARTESIAN_POINT('Ctrl Pts',(0.378436631346168,6.0215343104513,19.493156980117));
#12948=CARTESIAN_POINT('Ctrl Pts',(-2.54856580920985,5.468787139,19.6321014567242));
#12949=CARTESIAN_POINT('Ctrl Pts',(-4.8543845039449,3.58284755155288,19.7710459333314));
#12950=CARTESIAN_POINT('Ctrl Pts',(-5.97691054748803,0.823967558504157,
19.9099904099385));
#12951=CARTESIAN_POINT('Ctrl Pts',(-5.64268106414096,-2.13650848325456,
20.0489348865457));
#12952=CARTESIAN_POINT('Ctrl Pts',(-4.50271103912352,-3.7617705196067,20.1415645376172));
#12953=CARTESIAN_POINT('Ctrl Pts',(-3.7728463225773,-4.38915094994582,20.1878793631529));
#12954=CARTESIAN_POINT('Ctrl Pts',(4.61757708086507,-4.00682447667092,-0.564028230114873));
#12955=CARTESIAN_POINT('Ctrl Pts',(5.28394974986152,-3.23887976517851,-0.517707608387826));
#12956=CARTESIAN_POINT('Ctrl Pts',(6.22540816553931,-1.36498832388706,-0.425072161125049));
#12957=CARTESIAN_POINT('Ctrl Pts',(6.11935106486372,1.7803500074321,-0.286121888326544));
#12958=CARTESIAN_POINT('Ctrl Pts',(4.52194418999246,4.49082681434422,-0.147177411719357));
#12959=CARTESIAN_POINT('Ctrl Pts',(1.82221710647615,6.1070547216026,-0.00823293511216988));
#12960=CARTESIAN_POINT('Ctrl Pts',(-1.32161791239755,6.2345090701681,0.130711541495017));
#12961=CARTESIAN_POINT('Ctrl Pts',(-4.14333866301131,4.84241357882606,0.269656018102203));
#12962=CARTESIAN_POINT('Ctrl Pts',(-5.95511592912563,2.26994056792388,0.40860049470939));
#12963=CARTESIAN_POINT('Ctrl Pts',(-6.31535390416332,-0.855800004494397,
0.547544971316578));
#12964=CARTESIAN_POINT('Ctrl Pts',(-5.1362347291639,-3.77295417881752,0.686489447923763));
#12965=CARTESIAN_POINT('Ctrl Pts',(-2.70517152339663,-5.77045250626636,
0.825433924530953));
#12966=CARTESIAN_POINT('Ctrl Pts',(0.385272195480467,-6.3614191557082,0.964378401138136));
#12967=CARTESIAN_POINT('Ctrl Pts',(3.38180619255566,-5.40180223127101,1.10332287774532));
#12968=CARTESIAN_POINT('Ctrl Pts',(5.55403264741978,-3.12550882667008,1.24226735435251));
#12969=CARTESIAN_POINT('Ctrl Pts',(6.3724757969986,-0.0873791084211981,
1.3812118309597));
#12970=CARTESIAN_POINT('Ctrl Pts',(5.63764211908227,2.9720488473695,1.52015630756688));
#12971=CARTESIAN_POINT('Ctrl Pts',(3.52864560342288,5.30704658140607,1.65910078417407));
#12972=CARTESIAN_POINT('Ctrl Pts',(0.559549537634755,6.34846338242561,1.79804526078126));
#12973=CARTESIAN_POINT('Ctrl Pts',(-2.54593549951255,5.84245629601246,1.93698973738844));
#12974=CARTESIAN_POINT('Ctrl Pts',(-5.03085438168256,3.9123633857033,2.07593421399563));
#12975=CARTESIAN_POINT('Ctrl Pts',(-6.28951363016558,1.0286405554172,2.21487869060282));
#12976=CARTESIAN_POINT('Ctrl Pts',(-6.0151178318889,-2.10581114062593,2.35382316721));
#12977=CARTESIAN_POINT('Ctrl Pts',(-4.27455035785067,-4.72697602358444,
2.49276764381719));
#12978=CARTESIAN_POINT('Ctrl Pts',(-1.49207068182762,-6.19595094984961,
2.63171212042438));
#12979=CARTESIAN_POINT('Ctrl Pts',(1.65409792482501,-6.15467652645724,2.77065659703156));
#12980=CARTESIAN_POINT('Ctrl Pts',(4.39708381842427,-4.61321330367469,2.90960107363875));
#12981=CARTESIAN_POINT('Ctrl Pts',(6.06829025010777,-1.94728953455831,3.04854555024594));
#12982=CARTESIAN_POINT('Ctrl Pts',(6.26036434607312,1.19328175444802,3.18749002685313));
#12983=CARTESIAN_POINT('Ctrl Pts',(4.92648846994049,4.04299325335068,3.32643450346031));
#12984=CARTESIAN_POINT('Ctrl Pts',(2.39179191826967,5.90723408294864,3.4653789800675));
#12985=CARTESIAN_POINT('Ctrl Pts',(-0.725898626910438,6.33159966158133,
3.60432345667468));
#12986=CARTESIAN_POINT('Ctrl Pts',(-3.66665298623168,5.21265181741733,3.74326793328188));
#12987=CARTESIAN_POINT('Ctrl Pts',(-5.71366878455327,2.82313161427111,3.88221240988906));
#12988=CARTESIAN_POINT('Ctrl Pts',(-6.36799044554703,-0.254520679894365,
4.02115688649625));
#12989=CARTESIAN_POINT('Ctrl Pts',(-5.4701285105918,-3.27013412090137,4.16010136310343));
#12990=CARTESIAN_POINT('Ctrl Pts',(-3.23893484179065,-5.48865959790801,
4.29904583971062));
#12991=CARTESIAN_POINT('Ctrl Pts',(-0.218257964312433,-6.36933642949458,
4.43799031631781));
#12992=CARTESIAN_POINT('Ctrl Pts',(2.85561880955198,-5.69750158451984,4.576934792925));
#12993=CARTESIAN_POINT('Ctrl Pts',(5.23344481035494,-3.6369133214914,4.71587926953218));
#12994=CARTESIAN_POINT('Ctrl Pts',(6.33563020610351,-0.68983547500961,4.85482374613937));
#12995=CARTESIAN_POINT('Ctrl Pts',(5.89351974274144,2.42538824376421,4.99376822274656));
#12996=CARTESIAN_POINT('Ctrl Pts',(4.01487686851768,4.94942893894988,5.13271269935375));
#12997=CARTESIAN_POINT('Ctrl Pts',(1.15761663166472,6.26705726997656,5.27165717596093));
#12998=CARTESIAN_POINT('Ctrl Pts',(-1.98181010047945,6.05710424350701,5.41060165256812));
#12999=CARTESIAN_POINT('Ctrl Pts',(-4.63817500102154,4.3707454456845,5.54954612917531));
#13000=CARTESIAN_POINT('Ctrl Pts',(-6.16399499681084,1.6190271061238,5.68849060578249));
#13001=CARTESIAN_POINT('Ctrl Pts',(-6.18735483638979,-1.52732551202311,
5.82743508238968));
#13002=CARTESIAN_POINT('Ctrl Pts',(-4.70256061049319,-4.30139591245804,
5.96637955899686));
#13003=CARTESIAN_POINT('Ctrl Pts',(-2.07152762984648,-6.02701056659564,
6.10532403560405));
#13004=CARTESIAN_POINT('Ctrl Pts',(1.06443563188314,-6.28355471661148,6.24426851221124));
#13005=CARTESIAN_POINT('Ctrl Pts',(3.94094506106056,-5.00849629297808,6.38321298881842));
#13006=CARTESIAN_POINT('Ctrl Pts',(5.8568578422652,-2.51262796819774,6.52215746542561));
#13007=CARTESIAN_POINT('Ctrl Pts',(6.34517446981551,0.595687870175684,6.6611019420328));
#13008=CARTESIAN_POINT('Ctrl Pts',(5.28686884507105,3.55880610684117,6.80004641863999));
#13009=CARTESIAN_POINT('Ctrl Pts',(2.93990062489312,5.65447322098407,6.93899089524718));
#13010=CARTESIAN_POINT('Ctrl Pts',(-0.123661874547718,6.37187498557969,
7.07793537185436));
#13011=CARTESIAN_POINT('Ctrl Pts',(-3.15708206539707,5.53614630617914,7.21687984846155));
#13012=CARTESIAN_POINT('Ctrl Pts',(-5.42097048089627,3.35099420117735,7.35582432506874));
#13013=CARTESIAN_POINT('Ctrl Pts',(-6.36350932363407,0.349044666332412,
7.49476880167592));
#13014=CARTESIAN_POINT('Ctrl Pts',(-5.75495683398433,-2.73798373443851,
7.63371327828311));
#13015=CARTESIAN_POINT('Ctrl Pts',(-3.74364633621719,-5.15763465169844,
7.7726577548903));
#13016=CARTESIAN_POINT('Ctrl Pts',(-0.819830318568966,-6.32012352251346,
7.91160223149748));
#13017=CARTESIAN_POINT('Ctrl Pts',(2.3038175271616,-5.94209625406859,8.05054670810467));
#13018=CARTESIAN_POINT('Ctrl Pts',(4.86591494276851,-4.11569615749451,8.18949118471185));
#13019=CARTESIAN_POINT('Ctrl Pts',(6.24195634619481,-1.28610421944378,8.32843566131905));
#13020=CARTESIAN_POINT('Ctrl Pts',(6.09653468681619,1.85697277942353,8.46738013792624));
#13021=CARTESIAN_POINT('Ctrl Pts',(4.46509617268103,4.54741676776849,8.60632461453341));
#13022=CARTESIAN_POINT('Ctrl Pts',(1.74530033564544,6.12943797011348,8.74526909114061));
#13023=CARTESIAN_POINT('Ctrl Pts',(-1.39990860057091,6.21742221512424,8.88421356774779));
#13024=CARTESIAN_POINT('Ctrl Pts',(-4.20389290961247,4.78992353755077,9.02315804435498));
#13025=CARTESIAN_POINT('Ctrl Pts',(-5.98318761378964,2.19489158485495,9.16210252096216));
#13026=CARTESIAN_POINT('Ctrl Pts',(-6.30409356172975,-0.935140340286029,
9.30104699756935));
#13027=CARTESIAN_POINT('Ctrl Pts',(-5.08839063792002,-3.83723387442058,
9.43999147417654));
#13028=CARTESIAN_POINT('Ctrl Pts',(-2.63240374297399,-5.80401013309328,
9.57893595078373));
#13029=CARTESIAN_POINT('Ctrl Pts',(0.465225745926736,-6.35607175041312,
9.71788042739091));
#13030=CARTESIAN_POINT('Ctrl Pts',(3.44945748754508,-5.3588549273788,9.8568249039981));
#13031=CARTESIAN_POINT('Ctrl Pts',(5.59289159090131,-3.05542906045914,9.99576938060529));
#13032=CARTESIAN_POINT('Ctrl Pts',(6.37307073092924,-0.00724911345954777,
10.1347138572125));
#13033=CARTESIAN_POINT('Ctrl Pts',(5.59982796667497,3.04269778892314,10.2736583338197));
#13034=CARTESIAN_POINT('Ctrl Pts',(3.46163951282899,5.35099383052288,10.4126028104269));
#13035=CARTESIAN_POINT('Ctrl Pts',(0.479684078983856,6.35499695322053,10.551547287034));
#13036=CARTESIAN_POINT('Ctrl Pts',(-2.6191932888691,5.80998361500408,10.6904917636412));
#13037=CARTESIAN_POINT('Ctrl Pts',(-5.07964808175639,3.84879961242222,10.8294362402485));
#13038=CARTESIAN_POINT('Ctrl Pts',(-6.30194988224866,0.949479211304296,
10.9683807168555));
#13039=CARTESIAN_POINT('Ctrl Pts',(-5.98816532812638,-2.18127464893759,
11.1073251934627));
#13040=CARTESIAN_POINT('Ctrl Pts',(-4.21477871089973,-4.78034763476667,
11.2462696700699));
#13041=CARTESIAN_POINT('Ctrl Pts',(-1.41404909880579,-6.21422145061144,
11.3852141466772));
#13042=CARTESIAN_POINT('Ctrl Pts',(1.73135185565299,-6.13339252314735,11.5241586232844));
#13043=CARTESIAN_POINT('Ctrl Pts',(4.4547396220989,-4.55756272478778,11.6631030998916));
#13044=CARTESIAN_POINT('Ctrl Pts',(6.0922944519577,-1.87083708583035,11.8020475764987));
#13045=CARTESIAN_POINT('Ctrl Pts',(6.24486597493456,1.27190095769183,11.9409920531059));
#13046=CARTESIAN_POINT('Ctrl Pts',(4.87526521953232,4.10461595405606,12.0799365297131));
#13047=CARTESIAN_POINT('Ctrl Pts',(2.31732934265519,5.93683988404119,12.2188810063202));
#13048=CARTESIAN_POINT('Ctrl Pts',(-0.80545043950706,6.32197221447316,12.3578254829274));
#13049=CARTESIAN_POINT('Ctrl Pts',(-3.73190345732448,5.16613779106621,12.4967699595346));
#13050=CARTESIAN_POINT('Ctrl Pts',(-5.74871325603565,2.75106869978792,12.6357144361419));
#13051=CARTESIAN_POINT('Ctrl Pts',(-6.36428690495424,-0.334567306383601,
12.774658912749));
#13052=CARTESIAN_POINT('Ctrl Pts',(-5.4285796877572,-3.33865327111739,12.9136033893563));
#13053=CARTESIAN_POINT('Ctrl Pts',(-3.16966817044503,-5.52894988043305,
13.0525478659634));
#13054=CARTESIAN_POINT('Ctrl Pts',(-0.138157042496288,-6.37157717701681,
13.1914923425705));
#13055=CARTESIAN_POINT('Ctrl Pts',(2.92702955919275,-5.66114661978338,13.3304368191777));
#13056=CARTESIAN_POINT('Ctrl Pts',(5.2787591754345,-3.57082408679553,13.469381295785));
#13057=CARTESIAN_POINT('Ctrl Pts',(6.34380291029186,-0.610121075234528,
13.6083257723922));
#13058=CARTESIAN_POINT('Ctrl Pts',(5.86255870745683,2.49929759986584,13.7472702489993));
#13059=CARTESIAN_POINT('Ctrl Pts',(3.95232877767757,4.99951800918994,13.8862147256066));
#13060=CARTESIAN_POINT('Ctrl Pts',(1.07872744416156,6.28111695419576,14.0251592022138));
#13061=CARTESIAN_POINT('Ctrl Pts',(-2.05781131956035,6.03170752475302,14.1641036788208));
#13062=CARTESIAN_POINT('Ctrl Pts',(-4.6927631225145,4.31208271801931,14.303048155428));
#13063=CARTESIAN_POINT('Ctrl Pts',(-6.18386428675798,1.54139727975371,14.4419926320353));
#13064=CARTESIAN_POINT('Ctrl Pts',(-6.16766219928348,-1.6050003385054,14.5809371086424));
#13065=CARTESIAN_POINT('Ctrl Pts',(-4.64810608310154,-4.36018267178192,
14.7198815852497));
#13066=CARTESIAN_POINT('Ctrl Pts',(-1.99558438286049,-6.05258011611217,
14.8588260618568));
#13067=CARTESIAN_POINT('Ctrl Pts',(1.14335659986781,-6.26967453514227,14.997770538464));
#13068=CARTESIAN_POINT('Ctrl Pts',(4.00360693853646,-4.95854964407699,15.1367150150712));
#13069=CARTESIAN_POINT('Ctrl Pts',(5.88798693509895,-2.43878923713729,15.2756594916783));
#13070=CARTESIAN_POINT('Ctrl Pts',(6.3371831304334,0.675420655904715,15.4146039682855));
#13071=CARTESIAN_POINT('Ctrl Pts',(5.24170494478436,3.62499825695112,15.5535484448927));
#13072=CARTESIAN_POINT('Ctrl Pts',(2.86857276457088,5.69099054518877,15.6924929214999));
#13073=CARTESIAN_POINT('Ctrl Pts',(-0.203767686607458,6.36981646682085,
15.8314373981072));
#13074=CARTESIAN_POINT('Ctrl Pts',(-3.22644021456298,5.49601370384942,15.9703818747144));
#13075=CARTESIAN_POINT('Ctrl Pts',(-5.46267507161012,3.28256974839915,16.1093263513215));
#13076=CARTESIAN_POINT('Ctrl Pts',(-6.36739495409124,0.269006672213413,
16.2482708279286));
#13077=CARTESIAN_POINT('Ctrl Pts',(-5.72007639034474,-2.81012618570307,
16.3872153045359));
#13078=CARTESIAN_POINT('Ctrl Pts',(-3.67850184953075,-5.2042969971408,16.526159781143));
#13079=CARTESIAN_POINT('Ctrl Pts',(-0.740300613459242,-6.32993191842897,
16.6651042577503));
#13080=CARTESIAN_POINT('Ctrl Pts',(2.37834726082389,-5.91265992590842,16.8040487343575));
#13081=CARTESIAN_POINT('Ctrl Pts',(4.91727824720379,-4.05419014464293,16.9429932109646));
#13082=CARTESIAN_POINT('Ctrl Pts',(6.25763352934226,-1.20752047764986,17.0819376875718));
#13083=CARTESIAN_POINT('Ctrl Pts',(6.07270447019572,1.93347963887718,17.220882164179));
#13084=CARTESIAN_POINT('Ctrl Pts',(4.40756711841003,4.60319836289913,17.3598266407861));
#13085=CARTESIAN_POINT('Ctrl Pts',(1.66809502455076,6.15089766843531,17.4987711173933));
#13086=CARTESIAN_POINT('Ctrl Pts',(-1.477971546528,6.1993292468395,17.6377155940006));
#13087=CARTESIAN_POINT('Ctrl Pts',(-4.2637858160287,4.73668805462234,17.7766600706078));
#13088=CARTESIAN_POINT('Ctrl Pts',(-6.0103117246986,2.11948955787736,17.915604547215));
#13089=CARTESIAN_POINT('Ctrl Pts',(-6.29183742015302,-1.014329714779,18.0545490238221));
#13090=CARTESIAN_POINT('Ctrl Pts',(-5.03974168050939,-3.90090859517803,
18.1934935004293));
#13091=CARTESIAN_POINT('Ctrl Pts',(-2.55921998820667,-5.83664916897836,
18.3324379770364));
#13092=CARTESIAN_POINT('Ctrl Pts',(0.545105807019446,-6.34972030867309,
18.4713824536436));
#13093=CARTESIAN_POINT('Ctrl Pts',(3.51656348751869,-5.31505939160815,18.6103269302508));
#13094=CARTESIAN_POINT('Ctrl Pts',(5.63086615713259,-2.98486796173379,18.749271406858));
#13095=CARTESIAN_POINT('Ctrl Pts',(6.37265849741127,0.072885237843671,18.8882158834652));
#13096=CARTESIAN_POINT('Ctrl Pts',(5.56112774530412,3.11285947508733,19.0271603600725));
#13097=CARTESIAN_POINT('Ctrl Pts',(3.39408767243104,5.39410728635009,19.1661048366796));
#13098=CARTESIAN_POINT('Ctrl Pts',(0.399739803186753,6.36050197249609,19.3050493132868));
#13099=CARTESIAN_POINT('Ctrl Pts',(-2.69203113704428,5.77663924033402,19.4439937898939));
#13100=CARTESIAN_POINT('Ctrl Pts',(-5.12765029985884,3.78453526026606,19.5829382665011));
#13101=CARTESIAN_POINT('Ctrl Pts',(-6.3133662230816,0.870350812755841,19.7218827431083));
#13102=CARTESIAN_POINT('Ctrl Pts',(-5.96032210201671,-2.25677804382996,
19.8608272197155));
#13103=CARTESIAN_POINT('Ctrl Pts',(-4.75618023071243,-3.97353026262882,
19.9534568707871));
#13104=CARTESIAN_POINT('Ctrl Pts',(-3.98522955105091,-4.63622755188139,
19.9997716963227));
#13105=CARTESIAN_POINT('',(-2.03522692205371,4.71657388088067,20.0001232957739));
#13106=CARTESIAN_POINT('Ctrl Pts',(-3.98497178445977,-4.63592767842204,
20.));
#13107=CARTESIAN_POINT('Ctrl Pts',(-4.10345142310591,-4.51664357863181,
20.));
#13108=CARTESIAN_POINT('Ctrl Pts',(-4.21664327579648,-4.39262753031591,
20.));
#13109=CARTESIAN_POINT('Ctrl Pts',(-4.32436939900696,-4.2642850247564,20.));
#13110=CARTESIAN_POINT('Ctrl Pts',(-4.43329818051566,-4.13450969886763,
20.));
#13111=CARTESIAN_POINT('Ctrl Pts',(-4.53663891101179,-4.00031013114139,
20.));
#13112=CARTESIAN_POINT('Ctrl Pts',(-4.63416502605001,-3.86207416964644,
20.));
#13113=CARTESIAN_POINT('Ctrl Pts',(-4.73137732966119,-3.72428301233883,
20.));
#13114=CARTESIAN_POINT('Ctrl Pts',(-4.82281267416501,-3.58248070026889,
20.));
#13115=CARTESIAN_POINT('Ctrl Pts',(-4.90819951386566,-3.43703052021648,
20.));
#13116=CARTESIAN_POINT('Ctrl Pts',(-4.99221969940335,-3.29390833467434,
20.));
#13117=CARTESIAN_POINT('Ctrl Pts',(-5.07038362157542,-3.14725345974558,
20.));
#13118=CARTESIAN_POINT('Ctrl Pts',(-5.14238351610632,-2.99740187421602,
20.));
#13119=CARTESIAN_POINT('Ctrl Pts',(-5.17779799209172,-2.92369460823058,
20.));
#13120=CARTESIAN_POINT('Ctrl Pts',(-5.21172040481118,-2.84921385219213,
20.));
#13121=CARTESIAN_POINT('Ctrl Pts',(-5.24410947080105,-2.77399939051084,
20.));
#13122=CARTESIAN_POINT('Ctrl Pts',(-5.25356655628965,-2.75203797938769,
20.));
#13123=CARTESIAN_POINT('Ctrl Pts',(-5.26289289622801,-2.73001401712101,
20.));
#13124=CARTESIAN_POINT('Ctrl Pts',(-5.27208741122818,-2.70792849662542,
20.));
#13125=CARTESIAN_POINT('Ctrl Pts',(-5.28025870056582,-2.68830079705255,
20.));
#13126=CARTESIAN_POINT('Ctrl Pts',(-5.28832272962313,-2.6686319848304,20.));
#13127=CARTESIAN_POINT('Ctrl Pts',(-5.29627731007746,-2.64892710108863,
20.));
#13128=CARTESIAN_POINT('Ctrl Pts',(-5.35809518452346,-2.49579343978298,
20.));
#13129=CARTESIAN_POINT('Ctrl Pts',(-5.41334140189166,-2.34040024681067,
20.));
#13130=CARTESIAN_POINT('Ctrl Pts',(-5.46179567772308,-2.18310192386359,
20.));
#13131=CARTESIAN_POINT('Ctrl Pts',(-5.47241361317542,-2.14863265544187,
20.));
#13132=CARTESIAN_POINT('Ctrl Pts',(-5.48270521458296,-2.11407184571832,
20.));
#13133=CARTESIAN_POINT('Ctrl Pts',(-5.49266783943823,-2.07942313795932,
20.));
#13134=CARTESIAN_POINT('Ctrl Pts',(-5.53831342921429,-1.92067373972215,
20.));
#13135=CARTESIAN_POINT('Ctrl Pts',(-5.57705736058314,-1.76007949695175,
20.));
#13136=CARTESIAN_POINT('Ctrl Pts',(-5.60888551437011,-1.59809685908707,
20.));
#13137=CARTESIAN_POINT('Ctrl Pts',(-5.64065619906291,-1.43640669798783,
20.));
#13138=CARTESIAN_POINT('Ctrl Pts',(-5.66553599618983,-1.2733323692898,20.));
#13139=CARTESIAN_POINT('Ctrl Pts',(-5.68345920600138,-1.10933093107998,
20.));
#13140=CARTESIAN_POINT('Ctrl Pts',(-5.70113221551854,-0.947618882357451,
20.));
#13141=CARTESIAN_POINT('Ctrl Pts',(-5.71204135337902,-0.785004725997997,
20.));
#13142=CARTESIAN_POINT('Ctrl Pts',(-5.71607509551897,-0.621940605475564,
20.));
#13143=CARTESIAN_POINT('Ctrl Pts',(-5.71706208119408,-0.582041686432943,
20.));
#13144=CARTESIAN_POINT('Ctrl Pts',(-5.71763721586455,-0.54211592222943,
20.));
#13145=CARTESIAN_POINT('Ctrl Pts',(-5.71779842995933,-0.502170139060898,
20.));
#13146=CARTESIAN_POINT('Ctrl Pts',(-5.71788229794433,-0.481389249226882,
20.));
#13147=CARTESIAN_POINT('Ctrl Pts',(-5.71785409277925,-0.460611220002977,
20.));
#13148=CARTESIAN_POINT('Ctrl Pts',(-5.71771384536836,-0.439841148815751,
20.));
#13149=CARTESIAN_POINT('Ctrl Pts',(-5.71662256856856,-0.278227492825956,
20.));
#13150=CARTESIAN_POINT('Ctrl Pts',(-5.70875229303737,-0.117013828842298,
20.));
#13151=CARTESIAN_POINT('Ctrl Pts',(-5.69409684800798,0.0433725228550221,
20.));
#13152=CARTESIAN_POINT('Ctrl Pts',(-5.67956337329034,0.202424055085909,
20.));
#13153=CARTESIAN_POINT('Ctrl Pts',(-5.65835705764461,0.36066270542086,20.));
#13154=CARTESIAN_POINT('Ctrl Pts',(-5.63042198125465,0.517661960780568,
20.));
#13155=CARTESIAN_POINT('Ctrl Pts',(-5.61544285829542,0.601846844248007,
20.));
#13156=CARTESIAN_POINT('Ctrl Pts',(-5.59852821807851,0.685675140861376,
20.));
#13157=CARTESIAN_POINT('Ctrl Pts',(-5.57966365650049,0.769078844724802,
20.));
#13158=CARTESIAN_POINT('Ctrl Pts',(-5.54429238610119,0.925461750813273,
20.));
#13159=CARTESIAN_POINT('Ctrl Pts',(-5.50206814309807,1.08035384648384,20.));
#13160=CARTESIAN_POINT('Ctrl Pts',(-5.45314714973918,1.23332826719705,20.));
#13161=CARTESIAN_POINT('Ctrl Pts',(-5.41289015274892,1.35921064143795,20.));
#13162=CARTESIAN_POINT('Ctrl Pts',(-5.36809746764452,1.48379413599428,20.));
#13163=CARTESIAN_POINT('Ctrl Pts',(-5.31883665527128,1.60682291183031,20.));
#13164=CARTESIAN_POINT('Ctrl Pts',(-5.30921006803183,1.63086529331958,20.));
#13165=CARTESIAN_POINT('Ctrl Pts',(-5.29941130945311,1.65485162666062,20.));
#13166=CARTESIAN_POINT('Ctrl Pts',(-5.28945123030884,1.678755478121,20.));
#13167=CARTESIAN_POINT('Ctrl Pts',(-5.22881157867328,1.824288581253,20.));
#13168=CARTESIAN_POINT('Ctrl Pts',(-5.16212791782585,1.96694176941535,20.));
#13169=CARTESIAN_POINT('Ctrl Pts',(-5.08961453505449,2.10634429686568,20.));
#13170=CARTESIAN_POINT('Ctrl Pts',(-5.01729884220903,2.24536677756778,20.));
#13171=CARTESIAN_POINT('Ctrl Pts',(-4.93918471648935,2.38115692318346,20.));
#13172=CARTESIAN_POINT('Ctrl Pts',(-4.8554417170334,2.51331841980725,20.));
#13173=CARTESIAN_POINT('Ctrl Pts',(-4.77314573387395,2.64319626477504,20.));
#13174=CARTESIAN_POINT('Ctrl Pts',(-4.68541322918649,2.76957026126409,20.));
#13175=CARTESIAN_POINT('Ctrl Pts',(-4.59237070154098,2.89202857031072,20.));
#13176=CARTESIAN_POINT('Ctrl Pts',(-4.51158814582467,2.99835086640283,20.));
#13177=CARTESIAN_POINT('Ctrl Pts',(-4.4268020750054,3.10172108215086,20.));
#13178=CARTESIAN_POINT('Ctrl Pts',(-4.33807775610302,3.20184297416315,20.));
#13179=CARTESIAN_POINT('Ctrl Pts',(-4.30162703065241,3.24297617915682,20.));
#13180=CARTESIAN_POINT('Ctrl Pts',(-4.26451141446763,3.28356080052371,20.));
#13181=CARTESIAN_POINT('Ctrl Pts',(-4.22674502571624,3.32358241695396,20.));
#13182=CARTESIAN_POINT('Ctrl Pts',(-4.20574577986708,3.34583563709189,20.));
#13183=CARTESIAN_POINT('Ctrl Pts',(-4.18454533067273,3.36791477988588,20.));
#13184=CARTESIAN_POINT('Ctrl Pts',(-4.16314607616287,3.38981726275068,20.));
#13185=CARTESIAN_POINT('Ctrl Pts',(-4.14604768953812,3.40731773782059,20.));
#13186=CARTESIAN_POINT('Ctrl Pts',(-4.12882477256853,3.42470289052077,20.));
#13187=CARTESIAN_POINT('Ctrl Pts',(-4.11148805803735,3.44196235396036,20.));
#13188=CARTESIAN_POINT('Ctrl Pts',(-4.00202352440943,3.55093912188743,20.));
#13189=CARTESIAN_POINT('Ctrl Pts',(-3.88791934040221,3.65501678237065,20.));
#13190=CARTESIAN_POINT('Ctrl Pts',(-3.76954171862907,3.75394242380618,20.));
#13191=CARTESIAN_POINT('Ctrl Pts',(-3.66605495616142,3.8404240932624,20.));
#13192=CARTESIAN_POINT('Ctrl Pts',(-3.55930146424434,3.92296791358125,20.));
#13193=CARTESIAN_POINT('Ctrl Pts',(-3.44951147850304,4.00137564676462,20.));
#13194=CARTESIAN_POINT('Ctrl Pts',(-3.39461648563239,4.04057951335631,20.));
#13195=CARTESIAN_POINT('Ctrl Pts',(-3.33896219659931,4.0787489115657,20.));
#13196=CARTESIAN_POINT('Ctrl Pts',(-3.28257658007889,4.11585626044096,20.));
#13197=CARTESIAN_POINT('Ctrl Pts',(-3.24675220416138,4.13943226612191,20.));
#13198=CARTESIAN_POINT('Ctrl Pts',(-3.21063260796433,4.16257952185971,20.));
#13199=CARTESIAN_POINT('Ctrl Pts',(-3.17422489271026,4.18529053994777,20.));
#13200=CARTESIAN_POINT('Ctrl Pts',(-3.15332884709973,4.19832542737528,20.));
#13201=CARTESIAN_POINT('Ctrl Pts',(-3.13234039284392,4.21121498778926,20.));
#13202=CARTESIAN_POINT('Ctrl Pts',(-3.1112699212428,4.22395259948423,20.));
#13203=CARTESIAN_POINT('Ctrl Pts',(-2.98179244193094,4.30222487957077,20.));
#13204=CARTESIAN_POINT('Ctrl Pts',(-2.84912244425002,4.37482416604639,20.));
#13205=CARTESIAN_POINT('Ctrl Pts',(-2.71359482646064,4.44147979884137,20.));
#13206=CARTESIAN_POINT('Ctrl Pts',(-2.58015601234134,4.50710810943671,20.));
#13207=CARTESIAN_POINT('Ctrl Pts',(-2.44394632034707,4.56697476102533,20.));
#13208=CARTESIAN_POINT('Ctrl Pts',(-2.3052748294092,4.62077220858218,20.));
#13209=CARTESIAN_POINT('Ctrl Pts',(-2.2623645775541,4.6374191920985,20.));
#13210=CARTESIAN_POINT('Ctrl Pts',(-2.21921856473085,4.6534846662791,20.));
#13211=CARTESIAN_POINT('Ctrl Pts',(-2.17584588854955,4.66895849845131,20.));
#13212=CARTESIAN_POINT('Ctrl Pts',(-2.12925963268156,4.68557882185077,20.));
#13213=CARTESIAN_POINT('Ctrl Pts',(-2.08241187520335,4.70151658422014,20.));
#13214=CARTESIAN_POINT('Ctrl Pts',(-2.03531819920643,4.71676781801449,20.));
#13215=CARTESIAN_POINT('Ctrl Pts',(3.87994761181449,-3.36633437021265,-1.66506348639461E-15));
#13216=CARTESIAN_POINT('Ctrl Pts',(3.98625412824271,-3.26478406208168,-3.99257968720234E-15));
#13217=CARTESIAN_POINT('Ctrl Pts',(4.08787833026421,-3.15878135837575,-4.66065732929026E-15));
#13218=CARTESIAN_POINT('Ctrl Pts',(4.18469942561242,-3.04876049740387,-3.16066617322974E-15));
#13219=CARTESIAN_POINT('Ctrl Pts',(4.28403790290049,-2.93587905602415,-1.62167472872341E-15));
#13220=CARTESIAN_POINT('Ctrl Pts',(4.37832079024333,-2.8187674593301,-5.82952701121535E-16));
#13221=CARTESIAN_POINT('Ctrl Pts',(4.46739427387372,-2.69784518274753,-1.11716191852906E-15));
#13222=CARTESIAN_POINT('Ctrl Pts',(4.55725996217229,-2.57584744365813,-1.65612230338365E-15));
#13223=CARTESIAN_POINT('Ctrl Pts',(4.64182368695275,-2.4499704170692,-3.02543370549841E-15));
#13224=CARTESIAN_POINT('Ctrl Pts',(4.72089616098145,-2.32060185485371,-4.26048085699904E-15));
#13225=CARTESIAN_POINT('Ctrl Pts',(4.80003857099738,-2.19111887206108,-5.49662035122531E-15));
#13226=CARTESIAN_POINT('Ctrl Pts',(4.87368051051603,-2.05813757511725,-3.42002525595283E-15));
#13227=CARTESIAN_POINT('Ctrl Pts',(4.94159337332724,-1.92201238315165,-2.17881268582687E-15));
#13228=CARTESIAN_POINT('Ctrl Pts',(4.9612628949575,-1.88258660581057,-1.819321766357E-15));
#13229=CARTESIAN_POINT('Ctrl Pts',(4.98045155883349,-1.84289691540223,-3.90912234781053E-15));
#13230=CARTESIAN_POINT('Ctrl Pts',(4.99915311004593,-1.8029514969195,-3.83026943495679E-15));
#13231=CARTESIAN_POINT('Ctrl Pts',(5.0122478283282,-1.77498194531617,-3.86522662205903E-15));
#13232=CARTESIAN_POINT('Ctrl Pts',(5.02510451482084,-1.74688523424048,-6.32070288793251E-15));
#13233=CARTESIAN_POINT('Ctrl Pts',(5.03771836274217,-1.71866987256631,-5.49560397189452E-15));
#13234=CARTESIAN_POINT('Ctrl Pts',(5.04744161877782,-1.69692034875664,-4.85958488672596E-15));
#13235=CARTESIAN_POINT('Ctrl Pts',(5.05701729403857,-1.67510763703549,-4.39002047913497E-15));
#13236=CARTESIAN_POINT('Ctrl Pts',(5.0664416202758,-1.65324062354264,-3.95516952522712E-15));
#13237=CARTESIAN_POINT('Ctrl Pts',(5.12809970670852,-1.5101770056215,-1.11018336637909E-15));
#13238=CARTESIAN_POINT('Ctrl Pts',(5.18333108174967,-1.36468296185368,-3.57813607222297E-15));
#13239=CARTESIAN_POINT('Ctrl Pts',(5.23197030770333,-1.21718642306848,-4.52415882534751E-15));
#13240=CARTESIAN_POINT('Ctrl Pts',(5.23918133000613,-1.19531928168388,-4.66441169816742E-15));
#13241=CARTESIAN_POINT('Ctrl Pts',(5.24624739671494,-1.17340805699876,-4.80562514306417E-15));
#13242=CARTESIAN_POINT('Ctrl Pts',(5.25316790132191,-1.15145407394423,-4.71844785465692E-15));
#13243=CARTESIAN_POINT('Ctrl Pts',(5.2993807558818,-1.0048525927621,-3.31652852302662E-15));
#13244=CARTESIAN_POINT('Ctrl Pts',(5.33910647450617,-0.85634686171711,-4.64282921799142E-15));
#13245=CARTESIAN_POINT('Ctrl Pts',(5.37241286996191,-0.70637980290893,-3.24740234702858E-15));
#13246=CARTESIAN_POINT('Ctrl Pts',(5.40605735852673,-0.554890428987424,
-1.83781050255697E-15));
#13247=CARTESIAN_POINT('Ctrl Pts',(5.433151739794,-0.40190923262953,-4.04102800082177E-15));
#13248=CARTESIAN_POINT('Ctrl Pts',(5.45371837894091,-0.247868617103554,
-3.7470027081099E-15));
#13249=CARTESIAN_POINT('Ctrl Pts',(5.47436154606792,-0.0932548200734815,
-3.45188335420551E-15));
#13250=CARTESIAN_POINT('Ctrl Pts',(5.48842846893721,0.0624270392375904,
-4.61732734771393E-15));
#13251=CARTESIAN_POINT('Ctrl Pts',(5.49589140153741,0.218753153023537,-2.94209101525666E-15));
#13252=CARTESIAN_POINT('Ctrl Pts',(5.49724004581173,0.247003216313493,-2.63935507900513E-15));
#13253=CARTESIAN_POINT('Ctrl Pts',(5.49837288778739,0.275274336924491,-2.06251622087461E-15));
#13254=CARTESIAN_POINT('Ctrl Pts',(5.49928958238686,0.303564030594172,-1.08246744900953E-15));
#13255=CARTESIAN_POINT('Ctrl Pts',(5.49992470520323,0.323164265970328,-1.07591380186277E-15));
#13256=CARTESIAN_POINT('Ctrl Pts',(5.50045595765575,0.342771173576785,-2.10354853696197E-15));
#13257=CARTESIAN_POINT('Ctrl Pts',(5.50088315437835,0.362372657450585,-2.38697950294409E-15));
#13258=CARTESIAN_POINT('Ctrl Pts',(5.50434740873726,0.521326418934704,-4.20068571385626E-15));
#13259=CARTESIAN_POINT('Ctrl Pts',(5.50097990316086,0.680128718969271,-5.0287057528373E-15));
#13260=CARTESIAN_POINT('Ctrl Pts',(5.49085897729658,0.83831694807423,-4.49640324973188E-15));
#13261=CARTESIAN_POINT('Ctrl Pts',(5.48062459361156,0.998278502266276,-5.58026560193877E-15));
#13262=CARTESIAN_POINT('Ctrl Pts',(5.46348472039185,1.15761287955169,-3.85240679458042E-15));
#13263=CARTESIAN_POINT('Ctrl Pts',(5.43947063245582,1.31586030999698,-3.60822483003176E-15));
#13264=CARTESIAN_POINT('Ctrl Pts',(5.42659218943676,1.40072634868776,-3.51003661510938E-15));
#13265=CARTESIAN_POINT('Ctrl Pts',(5.41173583367755,1.48528002633643,-6.25273444309056E-15));
#13266=CARTESIAN_POINT('Ctrl Pts',(5.39490030124413,1.56945143909657,-5.93969318174459E-15));
#13267=CARTESIAN_POINT('Ctrl Pts',(5.36361962345765,1.72584321653484,-5.17779511488788E-15));
#13268=CARTESIAN_POINT('Ctrl Pts',(5.32550956672002,1.88091577537441,-5.32303990139189E-15));
#13269=CARTESIAN_POINT('Ctrl Pts',(5.28079475052835,2.0343024122608,-6.21724893790088E-15));
#13270=CARTESIAN_POINT('Ctrl Pts',(5.24056853374701,2.17229166576248,-7.02169474835133E-15));
#13271=CARTESIAN_POINT('Ctrl Pts',(5.19499619626958,2.30891683667062,-8.73640693159127E-15));
#13272=CARTESIAN_POINT('Ctrl Pts',(5.14420597728033,2.44390372836124,-6.38378239159465E-15));
#13273=CARTESIAN_POINT('Ctrl Pts',(5.13676783596577,2.46367232940273,-5.89581381797849E-15));
#13274=CARTESIAN_POINT('Ctrl Pts',(5.12922090618192,2.48339729434992,-7.37503164949818E-15));
#13275=CARTESIAN_POINT('Ctrl Pts',(5.12156722405834,2.50307433977403,-7.16093850883226E-15));
#13276=CARTESIAN_POINT('Ctrl Pts',(5.06254373198642,2.65481933203217,-5.82228573301255E-15));
#13277=CARTESIAN_POINT('Ctrl Pts',(4.99715084449456,2.80378105414597,-6.86084642416168E-15));
#13278=CARTESIAN_POINT('Ctrl Pts',(4.92569221311423,2.94959170115283,-5.93969318174459E-15));
#13279=CARTESIAN_POINT('Ctrl Pts',(4.85355670772662,3.09678350303263,-4.90588385216813E-15));
#13280=CARTESIAN_POINT('Ctrl Pts',(4.77523981660915,3.24076495388049,-2.82624632148367E-15));
#13281=CARTESIAN_POINT('Ctrl Pts',(4.69100020769895,3.38115471434809,-3.1641356201817E-15));
#13282=CARTESIAN_POINT('Ctrl Pts',(4.60668102574095,3.52167708750544,-3.16778207269044E-15));
#13283=CARTESIAN_POINT('Ctrl Pts',(4.51642766943348,3.6586017037791,-3.45017579044051E-15));
#13284=CARTESIAN_POINT('Ctrl Pts',(4.42044948051561,3.79153244523825,-1.72084568816899E-15));
#13285=CARTESIAN_POINT('Ctrl Pts',(4.3370333504216,3.90706461091121,-6.97009822649519E-16));
#13286=CARTESIAN_POINT('Ctrl Pts',(4.24929202402402,4.01958003898395,9.76388561238391E-16));
#13287=CARTESIAN_POINT('Ctrl Pts',(4.15733458420634,4.12880382702963,2.05391259555654E-15));
#13288=CARTESIAN_POINT('Ctrl Pts',(4.11146289933332,4.18328858863024,3.36724768757498E-15));
#13289=CARTESIAN_POINT('Ctrl Pts',(4.0645416851672,4.2369540081248,9.48537125816697E-16));
#13290=CARTESIAN_POINT('Ctrl Pts',(4.01659887073521,4.2897806305052,1.83186799063151E-15));
#13291=CARTESIAN_POINT('Ctrl Pts',(3.99710940469441,4.31125543700396,2.19095510507315E-15));
#13292=CARTESIAN_POINT('Ctrl Pts',(3.97744901168162,4.33259382998145,4.96890495175676E-15));
#13293=CARTESIAN_POINT('Ctrl Pts',(3.95762725058284,4.35378620795006,3.83026943495679E-15));
#13294=CARTESIAN_POINT('Ctrl Pts',(3.93076602539778,4.38250480838041,2.2872609773302E-15));
#13295=CARTESIAN_POINT('Ctrl Pts',(3.90361969409604,4.41094340467956,2.65613658226391E-15));
#13296=CARTESIAN_POINT('Ctrl Pts',(3.87619542506123,4.43909844700456,2.05391259555654E-15));
#13297=CARTESIAN_POINT('Ctrl Pts',(3.7605238672531,4.5578522997236,-4.86180145054305E-16));
#13298=CARTESIAN_POINT('Ctrl Pts',(3.63990082270005,4.67157471441651,6.00296082402392E-16));
#13299=CARTESIAN_POINT('Ctrl Pts',(3.51475018610364,4.78007264497113,1.94289029309402E-15));
#13300=CARTESIAN_POINT('Ctrl Pts',(3.38799964511639,4.88995759456307,3.30264799916393E-15));
#13301=CARTESIAN_POINT('Ctrl Pts',(3.25660455332876,4.99448417190688,4.82424686146942E-16));
#13302=CARTESIAN_POINT('Ctrl Pts',(3.12096094677142,5.09342213195151,4.10782519111308E-15));
#13303=CARTESIAN_POINT('Ctrl Pts',(3.0422347841794,5.15084471254106,6.21197058254715E-15));
#13304=CARTESIAN_POINT('Ctrl Pts',(2.96207671226679,5.20638416123899,4.7199000144875E-15));
#13305=CARTESIAN_POINT('Ctrl Pts',(2.88055840535682,5.25998984590168,5.16253706450698E-15));
#13306=CARTESIAN_POINT('Ctrl Pts',(2.81549585559289,5.30277437686413,5.32754643687697E-15));
#13307=CARTESIAN_POINT('Ctrl Pts',(2.7496398810422,5.34427876513908,2.86135815288528E-15));
#13308=CARTESIAN_POINT('Ctrl Pts',(2.68303739503652,5.38448001903572,3.44169137633799E-15));
#13309=CARTESIAN_POINT('Ctrl Pts',(2.53350644115478,5.47473688785431,4.7446124184256E-15));
#13310=CARTESIAN_POINT('Ctrl Pts',(2.38020694554204,5.55843341882744,6.34977018440613E-15));
#13311=CARTESIAN_POINT('Ctrl Pts',(2.22358026859405,5.63532026171932,7.21644966006352E-15));
#13312=CARTESIAN_POINT('Ctrl Pts',(2.06695359164605,5.7122071046112,8.08312913572091E-15));
#13313=CARTESIAN_POINT('Ctrl Pts',(1.90699906471761,5.78228482847051,5.00728262377208E-15));
#13314=CARTESIAN_POINT('Ctrl Pts',(1.74412150459255,5.84526005779857,3.66373598126302E-15));
#13315=CARTESIAN_POINT('Ctrl Pts',(1.68944058194602,5.86640197348599,3.0447967981167E-15));
#13316=CARTESIAN_POINT('Ctrl Pts',(1.6344299541403,5.88674298606999,3.67419985746786E-15));
#13317=CARTESIAN_POINT('Ctrl Pts',(1.57910765804983,5.90628229011343,4.44089209850063E-15));
#13318=CARTESIAN_POINT('Ctrl Pts',(-2.03514912955913,4.71639359924028,20.0001232957739));
#13319=CARTESIAN_POINT('Ctrl Pts',(-2.0338211300873,4.71696663813373,20.0000821971826));
#13320=CARTESIAN_POINT('Ctrl Pts',(-2.03249288858879,4.71753911613801,20.0000410985913));
#13321=CARTESIAN_POINT('Ctrl Pts',(-2.03116440553748,4.71811103304888,20.));
#13322=CARTESIAN_POINT('Ctrl Pts',(-1.57898373554274,5.90622195601506,0.000227687169849418));
#13323=CARTESIAN_POINT('Ctrl Pts',(-2.56111970282799,5.64365533898239,0.0465425127055785));
#13324=CARTESIAN_POINT('Ctrl Pts',(-4.39088445035941,4.61937212663427,0.139172163777036));
#13325=CARTESIAN_POINT('Ctrl Pts',(-6.0657765047469,1.95510796653054,0.278116640384223));
#13326=CARTESIAN_POINT('Ctrl Pts',(-6.26190048847721,-1.18494435610987,
0.41706111699141));
#13327=CARTESIAN_POINT('Ctrl Pts',(-4.93182523694634,-4.03654277149442,
0.556005593598598));
#13328=CARTESIAN_POINT('Ctrl Pts',(-2.39956484444413,-5.90405390794762,
0.694950070205784));
#13329=CARTESIAN_POINT('Ctrl Pts',(0.717551765537385,-6.33256105617076,
0.833894546812973));
#13330=CARTESIAN_POINT('Ctrl Pts',(3.65978322840781,-5.21747149734623,0.972839023420158));
#13331=CARTESIAN_POINT('Ctrl Pts',(5.70994220793149,-2.83065972743125,1.11178350002735));
#13332=CARTESIAN_POINT('Ctrl Pts',(6.36831967964836,0.246131796845876,1.25072797663453));
#13333=CARTESIAN_POINT('Ctrl Pts',(5.47443112253067,3.26292276856099,1.38967245324172));
#13334=CARTESIAN_POINT('Ctrl Pts',(3.24616319142365,5.48438682410978,1.52861692984891));
#13335=CARTESIAN_POINT('Ctrl Pts',(0.226649590892417,6.36904203396657,1.66756140645609));
#13336=CARTESIAN_POINT('Ctrl Pts',(-2.84810905785752,5.70125818109619,1.80650588306328));
#13337=CARTESIAN_POINT('Ctrl Pts',(-5.22864756594639,3.64380481219555,1.94545035967047));
#13338=CARTESIAN_POINT('Ctrl Pts',(-6.33471471180235,0.698182296261472,
2.08439483627765));
#13339=CARTESIAN_POINT('Ctrl Pts',(-5.89670918641703,-2.4176207243154,2.22333931288484));
#13340=CARTESIAN_POINT('Ctrl Pts',(-4.02139381088499,-4.94413397937359,
2.36228378949203));
#13341=CARTESIAN_POINT('Ctrl Pts',(-1.16587259232897,-6.26552553432391,
2.50122826609921));
#13342=CARTESIAN_POINT('Ctrl Pts',(1.97382749872696,-6.05970907400165,2.6401727427064));
#13343=CARTESIAN_POINT('Ctrl Pts',(4.63241149714395,-4.37685192827009,2.77911721931359));
#13344=CARTESIAN_POINT('Ctrl Pts',(6.1618554334486,-1.62714679528568,2.91806169592078));
#13345=CARTESIAN_POINT('Ctrl Pts',(6.18936072671635,1.51917177059382,3.05700617252796));
#13346=CARTESIAN_POINT('Ctrl Pts',(4.70822302351486,4.2951955762199,3.19595064913515));
#13347=CARTESIAN_POINT('Ctrl Pts',(2.07946636473173,6.02427495328891,3.33489512574233));
#13348=CARTESIAN_POINT('Ctrl Pts',(-1.05615562412742,6.28495062619459,3.47383960234952));
#13349=CARTESIAN_POINT('Ctrl Pts',(-3.93434201406849,5.01368347544235,3.61278407895671));
#13350=CARTESIAN_POINT('Ctrl Pts',(-5.85354123412349,2.52034205935053,3.7517285555639));
#13351=CARTESIAN_POINT('Ctrl Pts',(-6.34595271643967,-0.587327163036974,
3.89067303217109));
#13352=CARTESIAN_POINT('Ctrl Pts',(-5.29155225056067,-3.55183668758433,
4.02961750877827));
#13353=CARTESIAN_POINT('Ctrl Pts',(-2.94734761951486,-5.65059387015744,
4.16856198538546));
#13354=CARTESIAN_POINT('Ctrl Pts',(0.115266479274401,-6.37203128636819,
4.30750646199265));
#13355=CARTESIAN_POINT('Ctrl Pts',(3.14978462851293,-5.54030016061337,4.44645093859983));
#13356=CARTESIAN_POINT('Ctrl Pts',(5.4165497365127,-3.35813311641903,4.58539541520702));
#13357=CARTESIAN_POINT('Ctrl Pts',(6.36304281842322,-0.35742854757112,4.7243398918142));
#13358=CARTESIAN_POINT('Ctrl Pts',(5.75855827756034,2.73039843972416,4.8632843684214));
#13359=CARTESIAN_POINT('Ctrl Pts',(3.75043788466858,5.15269684232915,5.00222884502858));
#13360=CARTESIAN_POINT('Ctrl Pts',(0.828156546972091,6.31903677860904,5.14117332163577));
#13361=CARTESIAN_POINT('Ctrl Pts',(-2.29598611857659,5.94512546705365,5.28011779824296));
#13362=CARTESIAN_POINT('Ctrl Pts',(-4.8604872425344,4.12210296339946,5.41906227485014));
#13363=CARTESIAN_POINT('Ctrl Pts',(-6.2402553442469,1.29432697349022,5.55800675145734));
#13364=CARTESIAN_POINT('Ctrl Pts',(-6.09897499861954,-1.84893835535969,
5.69695122806451));
#13365=CARTESIAN_POINT('Ctrl Pts',(-4.47108297762739,-4.54152904679438,
5.83589570467171));
#13366=CARTESIAN_POINT('Ctrl Pts',(-1.75337436326174,-6.12713207120288,
5.97484018127889));
#13367=CARTESIAN_POINT('Ctrl Pts',(1.39171537667014,-6.21926019603992,6.11378465788608));
#13368=CARTESIAN_POINT('Ctrl Pts',(4.19757756964354,-4.79545739450698,6.25272913449327));
#13369=CARTESIAN_POINT('Ctrl Pts',(5.98028950791123,-2.20277245245013,6.39167361110045));
#13370=CARTESIAN_POINT('Ctrl Pts',(6.30531909684407,0.926833406109166,6.53061808770763));
#13371=CARTESIAN_POINT('Ctrl Pts',(5.09344109255171,3.83052567050686,6.66956256431483));
#13372=CARTESIAN_POINT('Ctrl Pts',(2.6400480799696,5.80053576931951,6.80850704092201));
#13373=CARTESIAN_POINT('Ctrl Pts',(-0.456850816813612,6.35667809526981,
6.9474515175292));
#13374=CARTESIAN_POINT('Ctrl Pts',(-3.44239333677469,5.36339418564733,7.08639599413638));
#13375=CARTESIAN_POINT('Ctrl Pts',(-5.58886008961009,3.06279479796965,7.22534047074357));
#13376=CARTESIAN_POINT('Ctrl Pts',(-6.37305454864607,0.0156459479743102,
7.36428494735076));
#13377=CARTESIAN_POINT('Ctrl Pts',(-5.60383104779562,-3.03531656725757,
7.50322942395795));
#13378=CARTESIAN_POINT('Ctrl Pts',(-3.4686861151783,-5.34642737817279,7.64217390056513));
#13379=CARTESIAN_POINT('Ctrl Pts',(-0.488056608814282,-6.35435833285306,
7.78111837717233));
#13380=CARTESIAN_POINT('Ctrl Pts',(2.61153561719795,-5.81342848892225,7.9200628537795));
#13381=CARTESIAN_POINT('Ctrl Pts',(5.07457180878865,-3.85548830022266,8.0590073303867));
#13382=CARTESIAN_POINT('Ctrl Pts',(6.30069233830012,-0.957781360119654,
8.19795180699388));
#13383=CARTESIAN_POINT('Ctrl Pts',(5.99103303675496,2.17338266953084,8.33689628360107));
#13384=CARTESIAN_POINT('Ctrl Pts',(4.22107267446567,4.77478947730533,8.47584076020826));
#13385=CARTESIAN_POINT('Ctrl Pts',(1.42223517760143,6.21235190369149,8.61478523681544));
#13386=CARTESIAN_POINT('Ctrl Pts',(-1.7232690002404,6.13566728469829,8.75372971342263));
#13387=CARTESIAN_POINT('Ctrl Pts',(-4.44873016821067,4.56342732670946,8.89267419002982));
#13388=CARTESIAN_POINT('Ctrl Pts',(-6.08982319069643,1.87886204436686,9.031618666637));
#13389=CARTESIAN_POINT('Ctrl Pts',(-6.24653527077042,-1.26367170844621,
9.1705631432442));
#13390=CARTESIAN_POINT('Ctrl Pts',(-4.88066818529498,-4.09818827541583,
9.30950761985137));
#13391=CARTESIAN_POINT('Ctrl Pts',(-2.32514901738218,-5.93378050846787,
9.44845209645857));
#13392=CARTESIAN_POINT('Ctrl Pts',(0.797120084246647,-6.32302685800061,
9.58739657306574));
#13393=CARTESIAN_POINT('Ctrl Pts',(3.72509292721283,-5.17104938666566,9.72634104967295));
#13394=CARTESIAN_POINT('Ctrl Pts',(5.74508260273416,-2.75864005688811,9.86528552628012));
#13395=CARTESIAN_POINT('Ctrl Pts',(6.36472109218032,0.3261816893409,10.0042300028873));
#13396=CARTESIAN_POINT('Ctrl Pts',(5.43297288333417,3.33149736975161,10.1431744794944));
#13397=CARTESIAN_POINT('Ctrl Pts',(3.17694954266129,5.52476792988544,10.2821189561018));
#13398=CARTESIAN_POINT('Ctrl Pts',(0.146551772968109,6.37138851849,10.4210634327089));
#13399=CARTESIAN_POINT('Ctrl Pts',(-2.91956766746306,5.66499723837627,10.560007909316));
#13400=CARTESIAN_POINT('Ctrl Pts',(-5.27404894206298,3.57777540273711,10.6989523859233));
#13401=CARTESIAN_POINT('Ctrl Pts',(-6.34299244425185,0.618478720628544,
10.8378968625304));
#13402=CARTESIAN_POINT('Ctrl Pts',(-5.86584555805418,-2.49157078261131,
10.9768413391376));
#13403=CARTESIAN_POINT('Ctrl Pts',(-3.95891178234414,-4.99430541470214,
11.1157858157449));
#13404=CARTESIAN_POINT('Ctrl Pts',(-1.08700201006022,-6.27968914085971,
11.254730292352));
#13405=CARTESIAN_POINT('Ctrl Pts',(2.04986209957812,-6.03441251891346,11.3936747689591));
#13406=CARTESIAN_POINT('Ctrl Pts',(4.6870768532492,-4.31826118332852,11.5326192455664));
#13407=CARTESIAN_POINT('Ctrl Pts',(6.18182698377473,-1.54954322894881,11.6715637221736));
#13408=CARTESIAN_POINT('Ctrl Pts',(6.16977045068138,1.59687246253577,11.8105081987807));
#13409=CARTESIAN_POINT('Ctrl Pts',(4.65384600726222,4.35405402084034,11.949452675388));
#13410=CARTESIAN_POINT('Ctrl Pts',(2.0035568859567,6.04994453531947,12.0883971519952));
#13411=CARTESIAN_POINT('Ctrl Pts',(-1.13509479784413,6.27117444149129,12.2273416286023));
#13412=CARTESIAN_POINT('Ctrl Pts',(-3.99706963356756,4.96381943871032,12.3662861052095));
#13413=CARTESIAN_POINT('Ctrl Pts',(-5.88476758082163,2.44654441926103,12.5052305818167));
#13414=CARTESIAN_POINT('Ctrl Pts',(-6.33806643733701,-0.667070394792312,
12.6441750584238));
#13415=CARTESIAN_POINT('Ctrl Pts',(-5.24647560876346,-3.61808827453898,
12.783119535031));
#13416=CARTESIAN_POINT('Ctrl Pts',(-2.87606794682533,-5.68720513441799,
12.9220640116383));
#13417=CARTESIAN_POINT('Ctrl Pts',(0.195374920185906,-6.37007831319747,
13.0610084882454));
#13418=CARTESIAN_POINT('Ctrl Pts',(3.2191955822385,-5.50025898290275,13.1999529648527));
#13419=CARTESIAN_POINT('Ctrl Pts',(5.45834443650017,-3.28976368273376,13.3388974414599));
#13420=CARTESIAN_POINT('Ctrl Pts',(6.36703389892958,-0.27739575625459,13.477841918067));
#13421=CARTESIAN_POINT('Ctrl Pts',(5.7237729215335,2.80258677268451,13.6167863946742));
#13422=CARTESIAN_POINT('Ctrl Pts',(3.68535494575419,5.19944497033206,13.7557308712814));
#13423=CARTESIAN_POINT('Ctrl Pts',(0.748639847677835,6.32894994878103,13.8946753478885));
#13424=CARTESIAN_POINT('Ctrl Pts',(-2.37055455855325,5.91578736607636,14.0336198244957));
#13425=CARTESIAN_POINT('Ctrl Pts',(-4.91193153076762,4.06066468854018,14.172564301103));
#13426=CARTESIAN_POINT('Ctrl Pts',(-6.25603604918701,1.21576396844905,14.3115087777102));
#13427=CARTESIAN_POINT('Ctrl Pts',(-6.07524560831743,-1.92547653175161,
14.4504532543174));
#13428=CARTESIAN_POINT('Ctrl Pts',(-4.41362747852017,-4.59738638321363,
14.5893977309245));
#13429=CARTESIAN_POINT('Ctrl Pts',(-1.67619740626309,-6.14869346535858,
14.7283422075317));
#13430=CARTESIAN_POINT('Ctrl Pts',(1.46980207887581,-6.20127010576371,14.8672866841389));
#13431=CARTESIAN_POINT('Ctrl Pts',(4.25754055598848,-4.74230086454031,15.0062311607461));
#13432=CARTESIAN_POINT('Ctrl Pts',(6.00751293300991,-2.12740626948055,15.1451756373533));
#13433=CARTESIAN_POINT('Ctrl Pts',(6.2931673110005,1.00603890156448,15.2841201139604));
#13434=CARTESIAN_POINT('Ctrl Pts',(5.04487606670623,3.89426431399836,15.4230645905676));
#13435=CARTESIAN_POINT('Ctrl Pts',(2.56690743182888,5.83327140737748,15.5620090671748));
#13436=CARTESIAN_POINT('Ctrl Pts',(-0.536739215927813,6.3504314884732,15.7009535437819));
#13437=CARTESIAN_POINT('Ctrl Pts',(-3.50955686615555,5.3196879305958,15.8398980203891));
#13438=CARTESIAN_POINT('Ctrl Pts',(-5.62692778742215,2.99228219772843,15.9788424969964));
#13439=CARTESIAN_POINT('Ctrl Pts',(-6.37274749768898,-0.0644857070020716,
16.1177869736036));
#13440=CARTESIAN_POINT('Ctrl Pts',(-5.56522409106071,-3.10553536318246,
16.2567314502108));
#13441=CARTESIAN_POINT('Ctrl Pts',(-3.40118961303849,-5.3896176387458,16.395675926818));
#13442=CARTESIAN_POINT('Ctrl Pts',(-0.408122684475576,-6.35999252751921,
16.5346204034251));
#13443=CARTESIAN_POINT('Ctrl Pts',(2.68442324634952,-5.78013329519202,16.6735648800323));
#13444=CARTESIAN_POINT('Ctrl Pts',(5.1226469442629,-3.79137934796153,16.8125093566395));
#13445=CARTESIAN_POINT('Ctrl Pts',(6.31223677206156,-0.878485064768902,
16.9514538332466));
#13446=CARTESIAN_POINT('Ctrl Pts',(5.96323283863802,2.24853801130179,17.0903983098538));
#13447=CARTESIAN_POINT('Ctrl Pts',(4.16070408122212,4.82748491694963,17.2293427864611));
#13448=CARTESIAN_POINT('Ctrl Pts',(1.34401290058344,6.22974304447622,17.3682872630683));
#13449=CARTESIAN_POINT('Ctrl Pts',(-1.80027845426065,6.11351507408893,17.5072317396755));
#13450=CARTESIAN_POINT('Ctrl Pts',(-4.50575591432981,4.50713131787952,17.6461762162826));
#13451=CARTESIAN_POINT('Ctrl Pts',(-6.11296533071532,1.8021442634666,17.7851206928898));
#13452=CARTESIAN_POINT('Ctrl Pts',(-6.23015295651432,-1.3421114688075,17.924065169497));
#13453=CARTESIAN_POINT('Ctrl Pts',(-4.82875457494639,-4.15923050307904,
18.0630096461041));
#13454=CARTESIAN_POINT('Ctrl Pts',(-2.25035792833039,-5.96254628347833,
18.2019541227113));
#13455=CARTESIAN_POINT('Ctrl Pts',(0.876558468963431,-6.31250460960645,
18.3408985993185));
#13456=CARTESIAN_POINT('Ctrl Pts',(3.78981571693129,-5.12380384386822,18.4798430759257));
#13457=CARTESIAN_POINT('Ctrl Pts',(5.77931368194271,-2.68618730619559,18.6187875525329));
#13458=CARTESIAN_POINT('Ctrl Pts',(6.3601168652194,0.406181626514434,18.7577320291401));
#13459=CARTESIAN_POINT('Ctrl Pts',(5.39065531759173,3.39954433923207,18.8966765057473));
#13460=CARTESIAN_POINT('Ctrl Pts',(3.10723404554619,5.56427631305468,19.0356209823545));
#13461=CARTESIAN_POINT('Ctrl Pts',(0.0664301762482525,6.37272689989223,
19.1745654589617));
#13462=CARTESIAN_POINT('Ctrl Pts',(-2.99056361179,5.62784200981625,19.3135099355688));
#13463=CARTESIAN_POINT('Ctrl Pts',(-5.31861862440418,3.51117792749949,19.452454412176));
#13464=CARTESIAN_POINT('Ctrl Pts',(-6.35026327979242,0.538682078665528,
19.5913988887833));
#13465=CARTESIAN_POINT('Ctrl Pts',(-5.83406261636922,-2.56513614738856,
19.7303433653904));
#13466=CARTESIAN_POINT('Ctrl Pts',(-3.89578808605346,-5.04366921786192,
19.8692878419977));
#13467=CARTESIAN_POINT('Ctrl Pts',(-1.00799057796779,-6.29289541535634,
20.0082323186047));
#13468=CARTESIAN_POINT('Ctrl Pts',(2.12563365775662,-6.0080922436061,20.147176795212));
#13469=CARTESIAN_POINT('Ctrl Pts',(4.74087939902799,-4.25912600074273,20.2861212718192));
#13470=CARTESIAN_POINT('Ctrl Pts',(6.20114346261515,-1.4712913257721,20.4250715454063));
#13471=CARTESIAN_POINT('Ctrl Pts',(6.16597040977451,0.625509887000643,20.5177069934577));
#13472=CARTESIAN_POINT('Ctrl Pts',(5.89878813698322,1.60653227262758,20.5640276159734));
#13473=CARTESIAN_POINT('Ctrl Pts',(-1.49483566411598,5.59146432056281,-0.187879788315434));
#13474=CARTESIAN_POINT('Ctrl Pts',(-2.42463110016866,5.34289054838787,-0.141564962779705));
#13475=CARTESIAN_POINT('Ctrl Pts',(-4.15688301637475,4.37319400148394,-0.0489353117082476));
#13476=CARTESIAN_POINT('Ctrl Pts',(-5.74251580035167,1.85091527530052,0.0900091648989393));
#13477=CARTESIAN_POINT('Ctrl Pts',(-5.92818783665532,-1.12179564845051,
0.228953641506126));
#13478=CARTESIAN_POINT('Ctrl Pts',(-4.66899568844553,-3.82142510954073,
0.367898118113314));
#13479=CARTESIAN_POINT('Ctrl Pts',(-2.27168591233214,-5.58941181330781,
0.5068425947205));
#13480=CARTESIAN_POINT('Ctrl Pts',(0.6793116013991,-5.99508272243367,0.645787071327689));
#13481=CARTESIAN_POINT('Ctrl Pts',(3.46474404365988,-4.93941913091394,0.784731547934873));
#13482=CARTESIAN_POINT('Ctrl Pts',(5.40564482098563,-2.67980664923482,0.923676024542063));
#13483=CARTESIAN_POINT('Ctrl Pts',(6.02893567764199,0.233014805482908,1.06262050114925));
#13484=CARTESIAN_POINT('Ctrl Pts',(5.1826847221403,3.08903329015262,1.20156497775644));
#13485=CARTESIAN_POINT('Ctrl Pts',(3.07316687363643,5.19210985898417,1.34050945436363));
#13486=CARTESIAN_POINT('Ctrl Pts',(0.214570855985937,6.02961953585579,1.47945393097081));
#13487=CARTESIAN_POINT('Ctrl Pts',(-2.69632606032752,5.39742358809429,1.618398407578));
#13488=CARTESIAN_POINT('Ctrl Pts',(-4.94999959830705,3.44961715801027,1.75734288418519));
#13489=CARTESIAN_POINT('Ctrl Pts',(-5.99712160426244,0.66097438055453,1.89628736079237));
#13490=CARTESIAN_POINT('Ctrl Pts',(-5.58245851072475,-2.28877954830255,
2.03523183739956));
#13491=CARTESIAN_POINT('Ctrl Pts',(-3.80708347568884,-4.68064846658789,
2.17417631400675));
#13492=CARTESIAN_POINT('Ctrl Pts',(-1.10374026761565,-5.93161969456096,
2.31312079061393));
#13493=CARTESIAN_POINT('Ctrl Pts',(1.86863719587062,-5.73677171846951,2.45206526722112));
#13494=CARTESIAN_POINT('Ctrl Pts',(4.3855384706743,-4.14359832318604,2.59100974382831));
#13495=CARTESIAN_POINT('Ctrl Pts',(5.83347443783502,-1.54043199153601,2.72995422043549));
#13496=CARTESIAN_POINT('Ctrl Pts',(5.85951390385553,1.43821123136604,2.86889869704268));
#13497=CARTESIAN_POINT('Ctrl Pts',(4.45730980740144,4.06629364645088,3.00784317364986));
#13498=CARTESIAN_POINT('Ctrl Pts',(1.96864629720973,5.70322597244586,3.14678765025706));
#13499=CARTESIAN_POINT('Ctrl Pts',(-0.999870396549506,5.95000957373033,
3.28573212686423));
#13500=CARTESIAN_POINT('Ctrl Pts',(-3.72467089120331,4.74649149258279,3.42467660347143));
#13501=CARTESIAN_POINT('Ctrl Pts',(-5.54159108873511,2.38602660134033,3.56362108007861));
#13502=CARTESIAN_POINT('Ctrl Pts',(-6.00776070696327,-0.5560270001831,3.7025655566858));
#13503=CARTESIAN_POINT('Ctrl Pts',(-5.00955193180152,-3.36255024938027,
3.84151003329299));
#13504=CARTESIAN_POINT('Ctrl Pts',(-2.79027594586576,-5.34945930753565,
3.98045450990018));
#13505=CARTESIAN_POINT('Ctrl Pts',(0.109123634536512,-6.03244948337102,
4.11939898650736));
#13506=CARTESIAN_POINT('Ctrl Pts',(2.98192457021544,-5.24504343114447,4.25834346311455));
#13507=CARTESIAN_POINT('Ctrl Pts',(5.12788798284495,-3.1791696356813,4.39728793972173));
#13508=CARTESIAN_POINT('Ctrl Pts',(6.0239400338134,-0.338380268431863,4.53623241632893));
#13509=CARTESIAN_POINT('Ctrl Pts',(5.45167001623907,2.58488854132713,4.67517689293611));
#13510=CARTESIAN_POINT('Ctrl Pts',(3.5505674820186,4.87809648250993,4.8141213695433));
#13511=CARTESIAN_POINT('Ctrl Pts',(0.784021971866293,5.98227918812514,4.95306584615048));
#13512=CARTESIAN_POINT('Ctrl Pts',(-2.17362716100671,5.62829456425105,5.09201032275767));
#13513=CARTESIAN_POINT('Ctrl Pts',(-4.60145947774681,3.90242558054578,5.23095479936486));
#13514=CARTESIAN_POINT('Ctrl Pts',(-5.90769621738016,1.22534898710367,5.36989927597204));
#13515=CARTESIAN_POINT('Ctrl Pts',(-5.77394506179285,-1.75040371355922,
5.50884375257924));
#13516=CARTESIAN_POINT('Ctrl Pts',(-4.23280755952943,-4.29949937795489,
5.64778822918641));
#13517=CARTESIAN_POINT('Ctrl Pts',(-1.65993257039433,-5.80060157214647,
5.78673270579361));
#13518=CARTESIAN_POINT('Ctrl Pts',(1.3175473138297,-5.88781995418203,5.92567718240079));
#13519=CARTESIAN_POINT('Ctrl Pts',(3.97387795247917,-4.539895236219,6.06462165900799));
#13520=CARTESIAN_POINT('Ctrl Pts',(5.66158462366403,-2.08538108894634,6.20356613561516));
#13521=CARTESIAN_POINT('Ctrl Pts',(5.9692925566167,0.877440089444528,6.34251061222236));
#13522=CARTESIAN_POINT('Ctrl Pts',(4.82199862280603,3.62638718543689,6.48145508882954));
#13523=CARTESIAN_POINT('Ctrl Pts',(2.4993531827375,5.49141042037324,6.62039956543673));
#13524=CARTESIAN_POINT('Ctrl Pts',(-0.432504071309366,6.01791450299395,
6.75934404204391));
#13525=CARTESIAN_POINT('Ctrl Pts',(-3.25893941393721,5.07756522689079,6.8982885186511));
#13526=CARTESIAN_POINT('Ctrl Pts',(-5.29101547764327,2.89957064966237,7.03723299525829));
#13527=CARTESIAN_POINT('Ctrl Pts',(-6.03341821339165,0.0148121354922382,
7.17617747186546));
#13528=CARTESIAN_POINT('Ctrl Pts',(-5.30518859527455,-2.87355680396488,
7.31512194847268));
#13529=CARTESIAN_POINT('Ctrl Pts',(-3.28383098310395,-5.06150262387076,
7.45406642507984));
#13530=CARTESIAN_POINT('Ctrl Pts',(-0.462046827044943,-6.01571836663433,
7.59301090168704));
#13531=CARTESIAN_POINT('Ctrl Pts',(2.47236022184536,-5.50361605405762,7.73195537829422));
#13532=CARTESIAN_POINT('Ctrl Pts',(4.8041349313123,-3.65001949293274,7.87089985490142));
#13533=CARTESIAN_POINT('Ctrl Pts',(5.96491236983892,-0.906738748034197,
8.00984433150859));
#13534=CARTESIAN_POINT('Ctrl Pts',(5.67175560244776,2.05755756253537,8.1487888081158));
#13535=CARTESIAN_POINT('Ctrl Pts',(3.99612094322675,4.52032876505112,8.28773328472297));
#13536=CARTESIAN_POINT('Ctrl Pts',(1.34644063671004,5.88127982235669,8.42667776133016));
#13537=CARTESIAN_POINT('Ctrl Pts',(-1.63143159897046,5.80868192234044,8.56562223793735));
#13538=CARTESIAN_POINT('Ctrl Pts',(-4.21164598835098,4.32023064266841,8.70456671454454));
#13539=CARTESIAN_POINT('Ctrl Pts',(-5.76528097706123,1.7787326928406,8.84351119115172));
#13540=CARTESIAN_POINT('Ctrl Pts',(-5.91364147059847,-1.19632741933878,
8.98245566775891));
#13541=CARTESIAN_POINT('Ctrl Pts',(-4.62056492658388,-3.87978536729377,
9.1214001443661));
#13542=CARTESIAN_POINT('Ctrl Pts',(-2.20123589453721,-5.61755420745052,
9.26034462097328));
#13543=CARTESIAN_POINT('Ctrl Pts',(0.754639521416892,-5.98605662600678,
9.39928909758048));
#13544=CARTESIAN_POINT('Ctrl Pts',(3.52657322200342,-4.89547097293942,9.53823357418765));
#13545=CARTESIAN_POINT('Ctrl Pts',(5.4389124945023,-2.61162509066496,9.67717805079486));
#13546=CARTESIAN_POINT('Ctrl Pts',(6.02552886808051,0.308798634990865,9.81612252740202));
#13547=CARTESIAN_POINT('Ctrl Pts',(5.14343589827507,3.15395337590449,9.95506700400922));
#13548=CARTESIAN_POINT('Ctrl Pts',(3.00764179678818,5.23033895261644,10.0940114806164));
#13549=CARTESIAN_POINT('Ctrl Pts',(0.138741655117083,6.03184097023283,10.2329559572236));
#13550=CARTESIAN_POINT('Ctrl Pts',(-2.76397645832849,5.36309508351754,10.3719004338308));
#13551=CARTESIAN_POINT('Ctrl Pts',(-4.99298141926652,3.38710662423008,10.510844910438));
#13552=CARTESIAN_POINT('Ctrl Pts',(-6.0049581952323,0.585518411799595,10.6497893870452));
#13553=CARTESIAN_POINT('Ctrl Pts',(-5.55323968385385,-2.35878861933721,
10.7887338636523));
#13554=CARTESIAN_POINT('Ctrl Pts',(-3.74793127384739,-4.72814613813498,
10.9276783402595));
#13555=CARTESIAN_POINT('Ctrl Pts',(-1.02907289988345,-5.94502848637157,
11.0666228168667));
#13556=CARTESIAN_POINT('Ctrl Pts',(1.94061971886987,-5.71282328133623,11.2055672934739));
#13557=CARTESIAN_POINT('Ctrl Pts',(4.43729057049544,-4.08813002851381,11.3445117700811));
#13558=CARTESIAN_POINT('Ctrl Pts',(5.85238165329467,-1.46696411722439,11.4834562466883));
#13559=CARTESIAN_POINT('Ctrl Pts',(5.84096764360742,1.51177105521146,11.6224007232955));
#13560=CARTESIAN_POINT('Ctrl Pts',(4.4058306810666,4.1220153744032,11.7613451999027));
#13561=CARTESIAN_POINT('Ctrl Pts',(1.89678222821199,5.72752755696409,11.9002896765098));
#13562=CARTESIAN_POINT('Ctrl Pts',(-1.07460270031642,5.93696755705441,12.039234153117));
#13563=CARTESIAN_POINT('Ctrl Pts',(-3.78405559583427,4.69928483757681,12.1781786297242));
#13564=CARTESIAN_POINT('Ctrl Pts',(-5.57115330375587,2.31616182575703,12.3171231063314));
#13565=CARTESIAN_POINT('Ctrl Pts',(-6.00029470779274,-0.631520511684512,
12.4560675829386));
#13566=CARTESIAN_POINT('Ctrl Pts',(-4.9668775392411,-3.42527112025111,12.5950120595458));
#13567=CARTESIAN_POINT('Ctrl Pts',(-2.72279494877608,-5.38411946412442,
12.733956536153));
#13568=CARTESIAN_POINT('Ctrl Pts',(0.184962892266474,-6.03060058912282,
12.8729010127602));
#13569=CARTESIAN_POINT('Ctrl Pts',(3.04763643714207,-5.20713614994345,13.0118454893673));
#13570=CARTESIAN_POINT('Ctrl Pts',(5.16745533664726,-3.114443783535,13.1507899659745));
#13571=CARTESIAN_POINT('Ctrl Pts',(6.02771841945788,-0.262612628736961,
13.2897344425817));
#13572=CARTESIAN_POINT('Ctrl Pts',(5.41873846057615,2.6532297738637,13.4286789191889));
#13573=CARTESIAN_POINT('Ctrl Pts',(3.48895297895264,4.92235328351202,13.5676233957961));
#13574=CARTESIAN_POINT('Ctrl Pts',(0.7087429203332,5.99166406016906,13.7065678724033));
#13575=CARTESIAN_POINT('Ctrl Pts',(-2.24422165858479,5.60051996551953,13.8455123490105));
#13576=CARTESIAN_POINT('Ctrl Pts',(-4.65016216862009,3.84426150808949,13.9844568256176));
#13577=CARTESIAN_POINT('Ctrl Pts',(-5.92263592829572,1.15097280502394,14.1234013022249));
#13578=CARTESIAN_POINT('Ctrl Pts',(-5.75148027123621,-1.82286297527398,
14.262345778832));
#13579=CARTESIAN_POINT('Ctrl Pts',(-4.17841401054488,-4.35237993441822,
14.4012902554392));
#13580=CARTESIAN_POINT('Ctrl Pts',(-1.58686857032097,-5.82101390460213,
14.5402347320464));
#13581=CARTESIAN_POINT('Ctrl Pts',(1.39147257646715,-5.87078860171135,14.6791792086536));
#13582=CARTESIAN_POINT('Ctrl Pts',(4.03064535830965,-4.48957155334236,14.8181236852608));
#13583=CARTESIAN_POINT('Ctrl Pts',(5.68735724298926,-2.01403136213456,14.957068161868));
#13584=CARTESIAN_POINT('Ctrl Pts',(5.95778837044127,0.952424521985176,15.0960126384751));
#13585=CARTESIAN_POINT('Ctrl Pts',(4.77602175108252,3.6867290340125,15.2349571150823));
#13586=CARTESIAN_POINT('Ctrl Pts',(2.43011038632597,5.52240149276691,15.3739015916895));
#13587=CARTESIAN_POINT('Ctrl Pts',(-0.508135013830756,6.0120007938093,15.5128460682967));
#13588=CARTESIAN_POINT('Ctrl Pts',(-3.32252362749587,5.03618818967038,15.6517905449039));
#13589=CARTESIAN_POINT('Ctrl Pts',(-5.32705445072409,2.83281584577332,15.7907350215111));
#13590=CARTESIAN_POINT('Ctrl Pts',(-6.03312752596339,-0.0610490991658619,
15.9296794981182));
#13591=CARTESIAN_POINT('Ctrl Pts',(-5.26863910175461,-2.94003346111913,
16.0686239747255));
#13592=CARTESIAN_POINT('Ctrl Pts',(-3.21993154175411,-5.10239116527476,
16.2075684513326));
#13593=CARTESIAN_POINT('Ctrl Pts',(-0.386372785454403,-6.02105230069328,
16.3465129279398));
#13594=CARTESIAN_POINT('Ctrl Pts',(2.54136348329514,-5.47209524614095,16.485457404547));
#13595=CARTESIAN_POINT('Ctrl Pts',(4.84964802017221,-3.58932707028654,16.6244018811542));
#13596=CARTESIAN_POINT('Ctrl Pts',(5.97584157127411,-0.831668354556176,
16.7633463577614));
#13597=CARTESIAN_POINT('Ctrl Pts',(5.6454369478098,2.12870768441387,16.9022908343686));
#13598=CARTESIAN_POINT('Ctrl Pts',(3.93896954632401,4.57021593028499,17.0412353109758));
#13599=CARTESIAN_POINT('Ctrl Pts',(1.27238702438789,5.89774414488229,17.1801797875829));
#13600=CARTESIAN_POINT('Ctrl Pts',(-1.70433702272646,5.78771025954717,17.3191242641901));
#13601=CARTESIAN_POINT('Ctrl Pts',(-4.26563268698053,4.26693479176628,17.4580687407973));
#13602=CARTESIAN_POINT('Ctrl Pts',(-5.78718981340038,1.70610339819993,17.5970132174045));
#13603=CARTESIAN_POINT('Ctrl Pts',(-5.89813221166215,-1.27058692476204,
17.7359576940117));
#13604=CARTESIAN_POINT('Ctrl Pts',(-4.57141792496805,-3.93757449891943,
17.8749021706189));
#13605=CARTESIAN_POINT('Ctrl Pts',(-2.13043061342123,-5.64478698092605,
18.0138466472261));
#13606=CARTESIAN_POINT('Ctrl Pts',(0.829844431956138,-5.97609513507295,
18.1527911238333));
#13607=CARTESIAN_POINT('Ctrl Pts',(3.58784676914289,-4.85074326564618,18.2917356004405));
#13608=CARTESIAN_POINT('Ctrl Pts',(5.47131931217262,-2.54303353189171,18.4306800770476));
#13609=CARTESIAN_POINT('Ctrl Pts',(6.02117001212022,0.38453517142386,18.5696245536548));
#13610=CARTESIAN_POINT('Ctrl Pts',(5.10337354356777,3.2183739487861,18.708569030262));
#13611=CARTESIAN_POINT('Ctrl Pts',(2.94164161636617,5.2677418332564,18.8475135068692));
#13612=CARTESIAN_POINT('Ctrl Pts',(0.0628899426853606,6.03310802587577,
18.9864579834764));
#13613=CARTESIAN_POINT('Ctrl Pts',(-2.83118884766385,5.32791995187452,19.1254024600835));
#13614=CARTESIAN_POINT('Ctrl Pts',(-5.03517586953364,3.32405829834529,19.2643469366908));
#13615=CARTESIAN_POINT('Ctrl Pts',(-6.01184154939821,0.509974336456724,
19.4032914132979));
#13616=CARTESIAN_POINT('Ctrl Pts',(-5.52315053621304,-2.42843349815221,
19.5422358899051));
#13617=CARTESIAN_POINT('Ctrl Pts',(-3.68817160036747,-4.77487921829192,
19.6811803665123));
#13618=CARTESIAN_POINT('Ctrl Pts',(-0.954272188574022,-5.95753096480961,
19.8201248431195));
#13619=CARTESIAN_POINT('Ctrl Pts',(2.01235321741153,-5.68790568064591,19.9590693197267));
#13620=CARTESIAN_POINT('Ctrl Pts',(4.48822584135349,-4.03214631066831,20.0980137963339));
#13621=CARTESIAN_POINT('Ctrl Pts',(5.87066870769925,-1.39288245759711,20.236964069921));
#13622=CARTESIAN_POINT('Ctrl Pts',(5.83737011657478,0.592174869378453,20.3295995179724));
#13623=CARTESIAN_POINT('Ctrl Pts',(5.58442666871165,1.52091606938026,20.3759201404881));
#13624=CARTESIAN_POINT('Ctrl Pts',(-1.41068759268922,5.27670668511055,-0.375987263800719));
#13625=CARTESIAN_POINT('Ctrl Pts',(-2.28814249750933,5.04212575779336,-0.329672438264988));
#13626=CARTESIAN_POINT('Ctrl Pts',(-3.92288158239009,4.12701587633362,-0.237042787193532));
#13627=CARTESIAN_POINT('Ctrl Pts',(-5.41925509595642,1.7467225840705,-0.0980983105863442));
#13628=CARTESIAN_POINT('Ctrl Pts',(-5.59447518483343,-1.05864694079116,
0.0408461660208423));
#13629=CARTESIAN_POINT('Ctrl Pts',(-4.40616613994472,-3.60630744758704,
0.179790642628029));
#13630=CARTESIAN_POINT('Ctrl Pts',(-2.14380698022015,-5.27476971866798,
0.318735119235216));
#13631=CARTESIAN_POINT('Ctrl Pts',(0.641071437260819,-5.65760438869658,
0.457679595842404));
#13632=CARTESIAN_POINT('Ctrl Pts',(3.26970485891195,-4.66136676448167,0.59662407244959));
#13633=CARTESIAN_POINT('Ctrl Pts',(5.10134743403979,-2.52895357103839,0.735568549056777));
#13634=CARTESIAN_POINT('Ctrl Pts',(5.68955167563563,0.219897814119939,0.874513025663964));
#13635=CARTESIAN_POINT('Ctrl Pts',(4.89093832174991,2.91514381174423,1.01345750227115));
#13636=CARTESIAN_POINT('Ctrl Pts',(2.9001705558492,4.89983289385856,1.15240197887834));
#13637=CARTESIAN_POINT('Ctrl Pts',(0.202492121079464,5.690197037745,1.29134645548553));
#13638=CARTESIAN_POINT('Ctrl Pts',(-2.54454306279754,5.09358899509239,1.43029093209272));
#13639=CARTESIAN_POINT('Ctrl Pts',(-4.67135163066769,3.25542950382497,1.5692354086999));
#13640=CARTESIAN_POINT('Ctrl Pts',(-5.65952849672254,0.623766464847588,
1.70817988530709));
#13641=CARTESIAN_POINT('Ctrl Pts',(-5.26820783503249,-2.1599383722897,1.84712436191428));
#13642=CARTESIAN_POINT('Ctrl Pts',(-3.59277314049268,-4.41716295380219,
1.98606883852146));
#13643=CARTESIAN_POINT('Ctrl Pts',(-1.04160794290234,-5.59771385479801,
2.12501331512865));
#13644=CARTESIAN_POINT('Ctrl Pts',(1.76344689301429,-5.41383436293737,2.26395779173584));
#13645=CARTESIAN_POINT('Ctrl Pts',(4.13866544420465,-3.91034471810202,2.40290226834302));
#13646=CARTESIAN_POINT('Ctrl Pts',(5.50509344222147,-1.45371718778633,2.54184674495021));
#13647=CARTESIAN_POINT('Ctrl Pts',(5.52966708099472,1.35725069213826,2.6807912215574));
#13648=CARTESIAN_POINT('Ctrl Pts',(4.20639659128802,3.83739171668186,2.81973569816458));
#13649=CARTESIAN_POINT('Ctrl Pts',(1.85782622968774,5.38217699160281,2.95868017477177));
#13650=CARTESIAN_POINT('Ctrl Pts',(-0.943585168971598,5.61506852126607,
3.09762465137895));
#13651=CARTESIAN_POINT('Ctrl Pts',(-3.51499976833812,4.47929950972323,3.23656912798615));
#13652=CARTESIAN_POINT('Ctrl Pts',(-5.22964094334671,2.25171114333013,3.37551360459333));
#13653=CARTESIAN_POINT('Ctrl Pts',(-5.66956869748686,-0.524726837329223,
3.51445808120052));
#13654=CARTESIAN_POINT('Ctrl Pts',(-4.72755161304236,-3.17326381117624,
3.65340255780771));
#13655=CARTESIAN_POINT('Ctrl Pts',(-2.63320427221665,-5.04832474491386,
3.79234703441489));
#13656=CARTESIAN_POINT('Ctrl Pts',(0.10298078979862,-5.69286768037385,3.93129151102208));
#13657=CARTESIAN_POINT('Ctrl Pts',(2.81406451191796,-4.94978670167555,4.07023598762927));
#13658=CARTESIAN_POINT('Ctrl Pts',(4.83922622917719,-3.00020615494359,4.20918046423645));
#13659=CARTESIAN_POINT('Ctrl Pts',(5.68483724920358,-0.319331989292594,
4.34812494084364));
#13660=CARTESIAN_POINT('Ctrl Pts',(5.1447817549178,2.43937864293008,4.48706941745082));
#13661=CARTESIAN_POINT('Ctrl Pts',(3.35069707936864,4.60349612269073,4.62601389405802));
#13662=CARTESIAN_POINT('Ctrl Pts',(0.739887396760496,5.64552159764121,4.7649583706652));
#13663=CARTESIAN_POINT('Ctrl Pts',(-2.05126820343682,5.31146366144845,4.90390284727239));
#13664=CARTESIAN_POINT('Ctrl Pts',(-4.34243171295922,3.68274819769209,5.04284732387957));
#13665=CARTESIAN_POINT('Ctrl Pts',(-5.57513709051344,1.15637100071714,5.18179180048677));
#13666=CARTESIAN_POINT('Ctrl Pts',(-5.44891512496616,-1.65186907175875,
5.32073627709394));
#13667=CARTESIAN_POINT('Ctrl Pts',(-3.99453214143147,-4.05746970911543,
5.45968075370114));
#13668=CARTESIAN_POINT('Ctrl Pts',(-1.56649077752693,-5.47407107309006,
5.59862523030832));
#13669=CARTESIAN_POINT('Ctrl Pts',(1.24337925098927,-5.55637971232417,5.73756970691551));
#13670=CARTESIAN_POINT('Ctrl Pts',(3.75017833531478,-4.28433307793102,5.8765141835227));
#13671=CARTESIAN_POINT('Ctrl Pts',(5.34287973941681,-1.96798972544256,6.01545866012988));
#13672=CARTESIAN_POINT('Ctrl Pts',(5.63326601638935,0.828046772779887,6.15440313673707));
#13673=CARTESIAN_POINT('Ctrl Pts',(4.55055615306033,3.42224870036692,6.29334761334426));
#13674=CARTESIAN_POINT('Ctrl Pts',(2.3586582855054,5.18228507142697,6.43229208995144));
#13675=CARTESIAN_POINT('Ctrl Pts',(-0.40815732580512,5.67915091071807,6.57123656655863));
#13676=CARTESIAN_POINT('Ctrl Pts',(-3.07548549109974,4.79173626813426,6.71018104316582));
#13677=CARTESIAN_POINT('Ctrl Pts',(-4.99317086567645,2.73634650135507,6.849125519773));
#13678=CARTESIAN_POINT('Ctrl Pts',(-5.69378187813725,0.0139783230101666,
6.9880699963802));
#13679=CARTESIAN_POINT('Ctrl Pts',(-5.00654614275347,-2.71179704067219,
7.12701447298738));
#13680=CARTESIAN_POINT('Ctrl Pts',(-3.0989758510296,-4.77657786956871,7.26595894959457));
#13681=CARTESIAN_POINT('Ctrl Pts',(-0.4360370452756,-5.6770784004156,7.40490342620175));
#13682=CARTESIAN_POINT('Ctrl Pts',(2.33318482649275,-5.19380361919299,7.54384790280894));
#13683=CARTESIAN_POINT('Ctrl Pts',(4.53369805383594,-3.44455068564283,7.68279237941613));
#13684=CARTESIAN_POINT('Ctrl Pts',(5.62913240137773,-0.855696135948733,
7.82173685602332));
#13685=CARTESIAN_POINT('Ctrl Pts',(5.35247816814056,1.9417324555399,7.9606813326305));
#13686=CARTESIAN_POINT('Ctrl Pts',(3.77116921198781,4.26586805279693,8.09962580923769));
#13687=CARTESIAN_POINT('Ctrl Pts',(1.27064609581863,5.55020774102186,8.23857028584488));
#13688=CARTESIAN_POINT('Ctrl Pts',(-1.53959419770053,5.48169655998261,8.37751476245207));
#13689=CARTESIAN_POINT('Ctrl Pts',(-3.9745618084913,4.07703395862735,8.51645923905925));
#13690=CARTESIAN_POINT('Ctrl Pts',(-5.44073876342602,1.67860334131436,8.65540371566644));
#13691=CARTESIAN_POINT('Ctrl Pts',(-5.58074767042653,-1.12898313023138,
8.79434819227362));
#13692=CARTESIAN_POINT('Ctrl Pts',(-4.36046166787279,-3.6613824591717,8.93329266888081));
#13693=CARTESIAN_POINT('Ctrl Pts',(-2.07732277169224,-5.30132790643318,
9.072237145488));
#13694=CARTESIAN_POINT('Ctrl Pts',(0.712158958587137,-5.64908639401295,
9.21118162209519));
#13695=CARTESIAN_POINT('Ctrl Pts',(3.32805351679401,-4.61989255921318,9.35012609870237));
#13696=CARTESIAN_POINT('Ctrl Pts',(5.13274238627044,-2.4646101244418,9.48907057530957));
#13697=CARTESIAN_POINT('Ctrl Pts',(5.68633664398072,0.291415580640832,9.62801505191675));
#13698=CARTESIAN_POINT('Ctrl Pts',(4.85389891321596,2.97640938205737,9.76695952852393));
#13699=CARTESIAN_POINT('Ctrl Pts',(2.83833405091507,4.93590997534744,9.90590400513113));
#13700=CARTESIAN_POINT('Ctrl Pts',(0.130931537266056,5.69229342197565,10.0448484817383));
#13701=CARTESIAN_POINT('Ctrl Pts',(-2.6083852491939,5.06119292865881,10.1837929583455));
#13702=CARTESIAN_POINT('Ctrl Pts',(-4.71191389647006,3.19643784572305,10.3227374349526));
#13703=CARTESIAN_POINT('Ctrl Pts',(-5.66692394621277,0.552558102970641,
10.4616819115598));
#13704=CARTESIAN_POINT('Ctrl Pts',(-5.24063380965353,-2.2260064560631,10.600626388167));
#13705=CARTESIAN_POINT('Ctrl Pts',(-3.53695076535063,-4.46198686156782,
10.7395708647742));
#13706=CARTESIAN_POINT('Ctrl Pts',(-0.971143789706699,-5.61036783188342,
10.8785153413814));
#13707=CARTESIAN_POINT('Ctrl Pts',(1.83137733816162,-5.39123404375903,11.0174598179886));
#13708=CARTESIAN_POINT('Ctrl Pts',(4.18750428774166,-3.85799887369909,11.1564042945958));
#13709=CARTESIAN_POINT('Ctrl Pts',(5.52293632281464,-1.38438500549997,11.295348771203));
#13710=CARTESIAN_POINT('Ctrl Pts',(5.51216483653343,1.42666964788716,11.4342932478101));
#13711=CARTESIAN_POINT('Ctrl Pts',(4.15781535487098,3.88997672796604,11.5732377244173));
#13712=CARTESIAN_POINT('Ctrl Pts',(1.79000757046727,5.40511057860874,11.7121822010245));
#13713=CARTESIAN_POINT('Ctrl Pts',(-1.0141106027887,5.60276067261754,11.8511266776317));
#13714=CARTESIAN_POINT('Ctrl Pts',(-3.57104155810099,4.4347502364433,11.9900711542389));
#13715=CARTESIAN_POINT('Ctrl Pts',(-5.25753902669011,2.18577923225303,12.1290156308461));
#13716=CARTESIAN_POINT('Ctrl Pts',(-5.66252297824849,-0.595970628576718,
12.2679601074533));
#13717=CARTESIAN_POINT('Ctrl Pts',(-4.68727946971874,-3.23245396596321,
12.4069045840605));
#13718=CARTESIAN_POINT('Ctrl Pts',(-2.56952195072682,-5.08103379383087,
12.5458490606676));
#13719=CARTESIAN_POINT('Ctrl Pts',(0.174550864347044,-5.69112286504815,
12.6847935372748));
#13720=CARTESIAN_POINT('Ctrl Pts',(2.87607729204563,-4.91401331698417,12.823738013882));
#13721=CARTESIAN_POINT('Ctrl Pts',(4.87656623679432,-2.93912388433625,12.9626824904892));
#13722=CARTESIAN_POINT('Ctrl Pts',(5.6884029399862,-0.247829501219334,13.1016269670964));
#13723=CARTESIAN_POINT('Ctrl Pts',(5.11370399961879,2.50387277504289,13.2405714437036));
#13724=CARTESIAN_POINT('Ctrl Pts',(3.29255101215109,4.64526159669196,13.3795159203108));
#13725=CARTESIAN_POINT('Ctrl Pts',(0.668845992988569,5.6543781715571,13.518460396918));
#13726=CARTESIAN_POINT('Ctrl Pts',(-2.11788875861632,5.2852525649627,13.6574048735251));
#13727=CARTESIAN_POINT('Ctrl Pts',(-4.38839280647255,3.62785832763879,13.7963493501323));
#13728=CARTESIAN_POINT('Ctrl Pts',(-5.58923580740444,1.08618164159884,13.9352938267395));
#13729=CARTESIAN_POINT('Ctrl Pts',(-5.42771493415498,-1.72024941879635,
14.0742383033467));
#13730=CARTESIAN_POINT('Ctrl Pts',(-3.94320054256959,-4.1073734856228,14.2131827799539));
#13731=CARTESIAN_POINT('Ctrl Pts',(-1.49753973437886,-5.49333434384569,
14.3521272565611));
#13732=CARTESIAN_POINT('Ctrl Pts',(1.31314307405848,-5.54030709765898,14.4910717331683));
#13733=CARTESIAN_POINT('Ctrl Pts',(3.80375016063084,-4.2368422421444,14.6300162097754));
#13734=CARTESIAN_POINT('Ctrl Pts',(5.36720155296861,-1.90065645478859,14.7689606863826));
#13735=CARTESIAN_POINT('Ctrl Pts',(5.62240942988205,0.898810142405872,14.9079051629898));
#13736=CARTESIAN_POINT('Ctrl Pts',(4.50716743545881,3.47919375402662,15.046849639597));
#13737=CARTESIAN_POINT('Ctrl Pts',(2.29331334082306,5.21153157815636,15.1857941162042));
#13738=CARTESIAN_POINT('Ctrl Pts',(-0.479530811733698,5.67357009914538,
15.3247385928114));
#13739=CARTESIAN_POINT('Ctrl Pts',(-3.1354903888362,4.75268844874498,15.4636830694186));
#13740=CARTESIAN_POINT('Ctrl Pts',(-5.02718111402602,2.67334949381821,15.6026275460257));
#13741=CARTESIAN_POINT('Ctrl Pts',(-5.69350755423781,-0.0576124913296487,
15.741572022633));
#13742=CARTESIAN_POINT('Ctrl Pts',(-4.9720541124485,-2.7745315590558,15.8805164992401));
#13743=CARTESIAN_POINT('Ctrl Pts',(-3.03867347046972,-4.81516469180373,
16.0194609758473));
#13744=CARTESIAN_POINT('Ctrl Pts',(-0.364622886433228,-5.68211207386736,
16.1584054524545));
#13745=CARTESIAN_POINT('Ctrl Pts',(2.39830372024077,-5.16405719708987,16.2973499290617));
#13746=CARTESIAN_POINT('Ctrl Pts',(4.57664909608152,-3.38727479261154,16.4362944056689));
#13747=CARTESIAN_POINT('Ctrl Pts',(5.63944637048666,-0.784851644343455,
16.575238882276));
#13748=CARTESIAN_POINT('Ctrl Pts',(5.32764105698159,2.00887735752595,16.7141833588833));
#13749=CARTESIAN_POINT('Ctrl Pts',(3.71723501142589,4.31294694362033,16.8531278354904));
#13750=CARTESIAN_POINT('Ctrl Pts',(1.20076114819234,5.56574524528835,16.9920723120976));
#13751=CARTESIAN_POINT('Ctrl Pts',(-1.60839559119228,5.4619054450054,17.1310167887048));
#13752=CARTESIAN_POINT('Ctrl Pts',(-4.02550945963125,4.02673826565304,17.269961265312));
#13753=CARTESIAN_POINT('Ctrl Pts',(-5.46141429608546,1.61006253293328,17.4089057419192));
#13754=CARTESIAN_POINT('Ctrl Pts',(-5.56611146680997,-1.1990623807166,17.5478502185264));
#13755=CARTESIAN_POINT('Ctrl Pts',(-4.31408127498971,-3.71591849475981,
17.6867946951336));
#13756=CARTESIAN_POINT('Ctrl Pts',(-2.01050329851204,-5.32702767837376,
17.8257391717407));
#13757=CARTESIAN_POINT('Ctrl Pts',(0.78313039494884,-5.63968566053946,17.9646836483479));
#13758=CARTESIAN_POINT('Ctrl Pts',(3.3858778213545,-4.57768268742415,18.1036281249551));
#13759=CARTESIAN_POINT('Ctrl Pts',(5.16332494240252,-2.39987975758783,18.2425726015623));
#13760=CARTESIAN_POINT('Ctrl Pts',(5.68222315902107,0.362888716333284,18.3815170781695));
#13761=CARTESIAN_POINT('Ctrl Pts',(4.81609176954379,3.03720355834013,18.5204615547767));
#13762=CARTESIAN_POINT('Ctrl Pts',(2.77604918718616,4.97120735345811,18.6594060313839));
#13763=CARTESIAN_POINT('Ctrl Pts',(0.0593497091224659,5.69348915185932,
18.7983505079911));
#13764=CARTESIAN_POINT('Ctrl Pts',(-2.6718140835377,5.02799789393279,18.9372949845982));
#13765=CARTESIAN_POINT('Ctrl Pts',(-4.7517331146631,3.13693866919109,19.0762394612054));
#13766=CARTESIAN_POINT('Ctrl Pts',(-5.67341981900402,0.481266594247914,
19.2151839378126));
#13767=CARTESIAN_POINT('Ctrl Pts',(-5.21223845605685,-2.29173084891586,
19.3541284144198));
#13768=CARTESIAN_POINT('Ctrl Pts',(-3.48055511468148,-4.50608921872194,
19.493072891027));
#13769=CARTESIAN_POINT('Ctrl Pts',(-0.900553799180242,-5.6221665142629,
19.6320173676342));
#13770=CARTESIAN_POINT('Ctrl Pts',(1.89907277706644,-5.3677191176857,19.7709618442413));
#13771=CARTESIAN_POINT('Ctrl Pts',(4.23557228367901,-3.8051666205939,19.9099063208486));
#13772=CARTESIAN_POINT('Ctrl Pts',(5.54019395278335,-1.31447358942211,20.0488565944357));
#13773=CARTESIAN_POINT('Ctrl Pts',(5.50876982337505,0.558839851756261,20.1414920424871));
#13774=CARTESIAN_POINT('Ctrl Pts',(5.27006520044008,1.43529986613293,20.1878126650028));
#13775=CARTESIAN_POINT('Ctrl Pts',(-1.32653952126248,4.96194904965828,-0.564094739286002));
#13776=CARTESIAN_POINT('Ctrl Pts',(-2.15165389485,4.74136096719883,-0.517779913750273));
#13777=CARTESIAN_POINT('Ctrl Pts',(-3.68888014840542,3.88083775118329,-0.425150262678815));
#13778=CARTESIAN_POINT('Ctrl Pts',(-5.0959943915612,1.64252989284048,-0.286205786071628));
#13779=CARTESIAN_POINT('Ctrl Pts',(-5.26076253301154,-0.99549823313181,
-0.147261309464441));
#13780=CARTESIAN_POINT('Ctrl Pts',(-4.14333659144391,-3.39118978563335,
-0.00831683285725419));
#13781=CARTESIAN_POINT('Ctrl Pts',(-2.01592804810816,-4.96012762402817,
0.130627643749933));
#13782=CARTESIAN_POINT('Ctrl Pts',(0.602831273122537,-5.32012605495949,
0.269572120357121));
#13783=CARTESIAN_POINT('Ctrl Pts',(3.07466567416403,-4.38331439804939,0.408516596964306));
#13784=CARTESIAN_POINT('Ctrl Pts',(4.79705004709394,-2.37810049284196,0.547461073571495));
#13785=CARTESIAN_POINT('Ctrl Pts',(5.35016767362928,0.20678082275697,0.686405550178681));
#13786=CARTESIAN_POINT('Ctrl Pts',(4.59919192135954,2.74125433333585,0.825350026785868));
#13787=CARTESIAN_POINT('Ctrl Pts',(2.72717423806198,4.60755592873295,0.964294503393056));
#13788=CARTESIAN_POINT('Ctrl Pts',(0.190413386172985,5.35077453963423,1.10323898000024));
#13789=CARTESIAN_POINT('Ctrl Pts',(-2.39276006526755,4.78975440209051,1.24218345660743));
#13790=CARTESIAN_POINT('Ctrl Pts',(-4.39270366302834,3.06124184963968,1.38112793321462));
#13791=CARTESIAN_POINT('Ctrl Pts',(-5.32193538918262,0.586558549140649,
1.5200724098218));
#13792=CARTESIAN_POINT('Ctrl Pts',(-4.95395715934022,-2.03109719627685,
1.65901688642899));
#13793=CARTESIAN_POINT('Ctrl Pts',(-3.37846280529652,-4.15367744101648,
1.79796136303618));
#13794=CARTESIAN_POINT('Ctrl Pts',(-0.979475618189015,-5.26380801503507,
1.93690583964336));
#13795=CARTESIAN_POINT('Ctrl Pts',(1.65825659015796,-5.09089700740523,2.07585031625056));
#13796=CARTESIAN_POINT('Ctrl Pts',(3.89179241773501,-3.67709111301799,2.21479479285774));
#13797=CARTESIAN_POINT('Ctrl Pts',(5.1767124466079,-1.36700238403667,2.35373926946493));
#13798=CARTESIAN_POINT('Ctrl Pts',(5.19982025813391,1.27629015291048,2.49268374607211));
#13799=CARTESIAN_POINT('Ctrl Pts',(3.9554833751746,3.60848978691285,2.6316282226793));
#13800=CARTESIAN_POINT('Ctrl Pts',(1.74700616216575,5.06112801075975,2.77057269928649));
#13801=CARTESIAN_POINT('Ctrl Pts',(-0.887299941393687,5.28012746880181,
2.90951717589367));
#13802=CARTESIAN_POINT('Ctrl Pts',(-3.30532864547293,4.21210752686368,3.04846165250086));
#13803=CARTESIAN_POINT('Ctrl Pts',(-4.91769079795831,2.11739568531994,3.18740612910805));
#13804=CARTESIAN_POINT('Ctrl Pts',(-5.33137668801045,-0.49342667447535,
3.32635060571523));
#13805=CARTESIAN_POINT('Ctrl Pts',(-4.44555129428321,-2.98397737297218,
3.46529508232243));
#13806=CARTESIAN_POINT('Ctrl Pts',(-2.47613259856755,-4.74719018229208,
3.60423955892961));
#13807=CARTESIAN_POINT('Ctrl Pts',(0.0968379450607276,-5.35328587737668,
3.7431840355368));
#13808=CARTESIAN_POINT('Ctrl Pts',(2.64620445362047,-4.65452997220665,3.88212851214398));
#13809=CARTESIAN_POINT('Ctrl Pts',(4.55056447550943,-2.82124267420587,4.02107298875117));
#13810=CARTESIAN_POINT('Ctrl Pts',(5.34573446459376,-0.30028371015333,4.16001746535835));
#13811=CARTESIAN_POINT('Ctrl Pts',(4.83789349359654,2.29386874453304,4.29896194196555));
#13812=CARTESIAN_POINT('Ctrl Pts',(3.15082667671865,4.32889576287152,4.43790641857272));
#13813=CARTESIAN_POINT('Ctrl Pts',(0.695752821654702,5.30876400715728,4.57685089517993));
#13814=CARTESIAN_POINT('Ctrl Pts',(-1.92890924586693,4.99463275864584,4.7157953717871));
#13815=CARTESIAN_POINT('Ctrl Pts',(-4.08340394817162,3.4630708148384,4.8547398483943));
#13816=CARTESIAN_POINT('Ctrl Pts',(-5.2425779636467,1.08739301433061,4.99368432500148));
#13817=CARTESIAN_POINT('Ctrl Pts',(-5.1238851881395,-1.55333442995828,5.13262880160866));
#13818=CARTESIAN_POINT('Ctrl Pts',(-3.7562567233335,-3.81544004027595,5.27157327821586));
#13819=CARTESIAN_POINT('Ctrl Pts',(-1.47304898465952,-5.14754057403365,
5.41051775482304));
#13820=CARTESIAN_POINT('Ctrl Pts',(1.16921118814885,-5.2249394704663,5.54946223143023));
#13821=CARTESIAN_POINT('Ctrl Pts',(3.5264787181504,-4.02877091964304,5.68840670803742));
#13822=CARTESIAN_POINT('Ctrl Pts',(5.0241748551696,-1.85059836193878,5.8273511846446));
#13823=CARTESIAN_POINT('Ctrl Pts',(5.29723947616198,0.778653456115254,5.96629566125179));
#13824=CARTESIAN_POINT('Ctrl Pts',(4.27911368331464,3.21811021529694,6.10524013785897));
#13825=CARTESIAN_POINT('Ctrl Pts',(2.2179633882733,4.87315972248072,6.24418461446617));
#13826=CARTESIAN_POINT('Ctrl Pts',(-0.383810580300875,5.34038731844219,
6.38312909107335));
#13827=CARTESIAN_POINT('Ctrl Pts',(-2.89203156826225,4.50590730937773,6.52207356768053));
#13828=CARTESIAN_POINT('Ctrl Pts',(-4.69532625370965,2.57312235304776,6.66101804428772));
#13829=CARTESIAN_POINT('Ctrl Pts',(-5.35414554288283,0.0131445105281004,
6.79996252089491));
#13830=CARTESIAN_POINT('Ctrl Pts',(-4.70790369023241,-2.55003727737951,
6.9389069975021));
#13831=CARTESIAN_POINT('Ctrl Pts',(-2.91412071895525,-4.49165311526668,
7.07785147410929));
#13832=CARTESIAN_POINT('Ctrl Pts',(-0.410027263506262,-5.3384384341969,
7.21679595071647));
#13833=CARTESIAN_POINT('Ctrl Pts',(2.19400943114016,-4.88399118432835,7.35574042732366));
#13834=CARTESIAN_POINT('Ctrl Pts',(4.26326117635958,-3.23908187835291,7.49468490393085));
#13835=CARTESIAN_POINT('Ctrl Pts',(5.29335243291654,-0.804653523863272,
7.63362938053803));
#13836=CARTESIAN_POINT('Ctrl Pts',(5.03320073383335,1.82590734854443,7.77257385714523));
#13837=CARTESIAN_POINT('Ctrl Pts',(3.54621748074888,4.01140734054273,7.9115183337524));
#13838=CARTESIAN_POINT('Ctrl Pts',(1.19485155492724,5.21913565968705,8.0504628103596));
#13839=CARTESIAN_POINT('Ctrl Pts',(-1.4477567964306,5.15471119762476,8.18940728696677));
#13840=CARTESIAN_POINT('Ctrl Pts',(-3.7374776286316,3.83383727458631,8.32835176357398));
#13841=CARTESIAN_POINT('Ctrl Pts',(-5.11619654979082,1.57847398978809,8.46729624018115));
#13842=CARTESIAN_POINT('Ctrl Pts',(-5.24785387025458,-1.06163884112396,
8.60624071678835));
#13843=CARTESIAN_POINT('Ctrl Pts',(-4.1003584091617,-3.44297955104964,8.74518519339552));
#13844=CARTESIAN_POINT('Ctrl Pts',(-1.95340964884727,-4.98510160541583,
8.88412967000273));
#13845=CARTESIAN_POINT('Ctrl Pts',(0.669678395757383,-5.31211616201914,
9.0230741466099));
#13846=CARTESIAN_POINT('Ctrl Pts',(3.1295338115846,-4.34431414548693,9.16201862321709));
#13847=CARTESIAN_POINT('Ctrl Pts',(4.82657227803858,-2.31759515821866,9.30096309982428));
#13848=CARTESIAN_POINT('Ctrl Pts',(5.34714441988092,0.274032526290802,9.43990757643146));
#13849=CARTESIAN_POINT('Ctrl Pts',(4.56436192815685,2.79886538821026,9.57885205303865));
#13850=CARTESIAN_POINT('Ctrl Pts',(2.66902630504195,4.64148099807844,9.71779652964585));
#13851=CARTESIAN_POINT('Ctrl Pts',(0.123121419415037,5.35274587371849,9.85674100625302));
#13852=CARTESIAN_POINT('Ctrl Pts',(-2.45279404005934,4.75929077380007,9.99568548286022));
#13853=CARTESIAN_POINT('Ctrl Pts',(-4.4308463736736,3.00576906721603,10.1346299594674));
#13854=CARTESIAN_POINT('Ctrl Pts',(-5.32888969719323,0.519597794141693,
10.2735744360746));
#13855=CARTESIAN_POINT('Ctrl Pts',(-4.92802793545319,-2.09322429278901,
10.4125189126818));
#13856=CARTESIAN_POINT('Ctrl Pts',(-3.32597025685388,-4.19582758500065,
10.551463389289));
#13857=CARTESIAN_POINT('Ctrl Pts',(-0.913214679529933,-5.27570717739528,
10.6904078658962));
#13858=CARTESIAN_POINT('Ctrl Pts',(1.72213495745338,-5.0696448061818,10.8293523425034));
#13859=CARTESIAN_POINT('Ctrl Pts',(3.93771800498789,-3.62786771888437,10.9682968191105));
#13860=CARTESIAN_POINT('Ctrl Pts',(5.19349099233457,-1.30180589377555,11.1072412957177));
#13861=CARTESIAN_POINT('Ctrl Pts',(5.18336202945946,1.34156824056286,11.2461857723249));
#13862=CARTESIAN_POINT('Ctrl Pts',(3.90980002867536,3.65793808152889,11.3851302489321));
#13863=CARTESIAN_POINT('Ctrl Pts',(1.68323291272256,5.08269360025337,11.5240747255393));
#13864=CARTESIAN_POINT('Ctrl Pts',(-0.953618505260992,5.26855378818066,
11.6630192021465));
#13865=CARTESIAN_POINT('Ctrl Pts',(-3.3580275203677,4.17021563530979,11.8019636787537));
#13866=CARTESIAN_POINT('Ctrl Pts',(-4.94392474962437,2.05539663874902,11.9409081553609));
#13867=CARTESIAN_POINT('Ctrl Pts',(-5.32475124870422,-0.560420745468919,
12.079852631968));
#13868=CARTESIAN_POINT('Ctrl Pts',(-4.40768140019639,-3.03963681167534,
12.2187971085752));
#13869=CARTESIAN_POINT('Ctrl Pts',(-2.41624895267756,-4.77794812353731,
12.3577415851824));
#13870=CARTESIAN_POINT('Ctrl Pts',(0.164138836427611,-5.35164514097351,
12.4966860617896));
#13871=CARTESIAN_POINT('Ctrl Pts',(2.70451814694919,-4.62089048402487,12.6356305383968));
#13872=CARTESIAN_POINT('Ctrl Pts',(4.58567713694141,-2.76380398513751,12.774575015004));
#13873=CARTESIAN_POINT('Ctrl Pts',(5.34908746051452,-0.233046373701707,
12.9135194916112));
#13874=CARTESIAN_POINT('Ctrl Pts',(4.80866953866144,2.35451577622209,13.0524639682184));
#13875=CARTESIAN_POINT('Ctrl Pts',(3.09614904534953,4.36816990987189,13.1914084448255));
#13876=CARTESIAN_POINT('Ctrl Pts',(0.628949065643935,5.31709228294514,13.3303529214327));
#13877=CARTESIAN_POINT('Ctrl Pts',(-1.99155585864786,4.96998516440586,13.4692973980399));
#13878=CARTESIAN_POINT('Ctrl Pts',(-4.12662344432501,3.41145514718809,13.6082418746471));
#13879=CARTESIAN_POINT('Ctrl Pts',(-5.25583568651315,1.02139047817374,13.7471863512543));
#13880=CARTESIAN_POINT('Ctrl Pts',(-5.10394959707376,-1.61763586231873,
13.8861308278615));
#13881=CARTESIAN_POINT('Ctrl Pts',(-3.70798707459429,-3.86236703682739,
14.0250753044687));
#13882=CARTESIAN_POINT('Ctrl Pts',(-1.40821089843674,-5.16565478308926,
14.1640197810758));
#13883=CARTESIAN_POINT('Ctrl Pts',(1.23481357164983,-5.20982559360661,14.302964257683));
#13884=CARTESIAN_POINT('Ctrl Pts',(3.57685496295202,-3.98411293094645,14.4419087342902));
#13885=CARTESIAN_POINT('Ctrl Pts',(5.04704586294798,-1.7872815474426,14.5808532108974));
#13886=CARTESIAN_POINT('Ctrl Pts',(5.28703048932282,0.845195762826563,14.7197976875046));
#13887=CARTESIAN_POINT('Ctrl Pts',(4.2383131198351,3.27165847404077,14.8587421641118));
#13888=CARTESIAN_POINT('Ctrl Pts',(2.15651629532014,4.9006616635458,14.997686640719));
#13889=CARTESIAN_POINT('Ctrl Pts',(-0.450926609636636,5.33513940448148,
15.1366311173262));
#13890=CARTESIAN_POINT('Ctrl Pts',(-2.94845715017653,4.46918870781955,15.2755755939333));
#13891=CARTESIAN_POINT('Ctrl Pts',(-4.72730777732795,2.5138831418631,15.4145200705406));
#13892=CARTESIAN_POINT('Ctrl Pts',(-5.35388758251222,-0.054175883493441,
15.5534645471477));
#13893=CARTESIAN_POINT('Ctrl Pts',(-4.67546912314239,-2.60902965699247,
15.6924090237549));
#13894=CARTESIAN_POINT('Ctrl Pts',(-2.85741539918533,-4.52793821833268,
15.8313535003621));
#13895=CARTESIAN_POINT('Ctrl Pts',(-0.342872987412053,-5.34317184704143,
15.9702979769693));
#13896=CARTESIAN_POINT('Ctrl Pts',(2.25524395718639,-4.85601914803879,16.1092424535765));
#13897=CARTESIAN_POINT('Ctrl Pts',(4.30365017199082,-3.18522251493655,16.2481869301836));
#13898=CARTESIAN_POINT('Ctrl Pts',(5.30305116969921,-0.73803493413073,16.3871314067908));
#13899=CARTESIAN_POINT('Ctrl Pts',(5.00984516615337,1.88904703063804,16.526075883398));
#13900=CARTESIAN_POINT('Ctrl Pts',(3.49550047652777,4.05567795695568,16.6650203600052));
#13901=CARTESIAN_POINT('Ctrl Pts',(1.12913527199678,5.23374634569442,16.8039648366124));
#13902=CARTESIAN_POINT('Ctrl Pts',(-1.51245415965809,5.13610063046365,16.9429093132196));
#13903=CARTESIAN_POINT('Ctrl Pts',(-3.78538623228198,3.78654173953978,17.0818537898268));
#13904=CARTESIAN_POINT('Ctrl Pts',(-5.13563877877053,1.51402166766663,17.220798266434));
#13905=CARTESIAN_POINT('Ctrl Pts',(-5.23409072195781,-1.12753783667114,
17.3597427430411));
#13906=CARTESIAN_POINT('Ctrl Pts',(-4.05674462501138,-3.4942624906002,17.4986872196483));
#13907=CARTESIAN_POINT('Ctrl Pts',(-1.89057598360286,-5.00926837582149,
17.6376316962555));
#13908=CARTESIAN_POINT('Ctrl Pts',(0.736416357941547,-5.30327618600596,
17.7765761728627));
#13909=CARTESIAN_POINT('Ctrl Pts',(3.18390887356609,-4.3046221092021,17.9155206494699));
#13910=CARTESIAN_POINT('Ctrl Pts',(4.85533057263242,-2.25672598328394,18.0544651260771));
#13911=CARTESIAN_POINT('Ctrl Pts',(5.3432763059219,0.341242261242714,18.1934096026843));
#13912=CARTESIAN_POINT('Ctrl Pts',(4.52880999551982,2.85603316789416,18.3323540792915));
#13913=CARTESIAN_POINT('Ctrl Pts',(2.61045675800614,4.67467287365983,18.4712985558986));
#13914=CARTESIAN_POINT('Ctrl Pts',(0.0558094755595731,5.35387027784286,
18.6102430325058));
#13915=CARTESIAN_POINT('Ctrl Pts',(-2.51243931941155,4.72807583599107,18.749187509113));
#13916=CARTESIAN_POINT('Ctrl Pts',(-4.46829035979255,2.9498190400369,18.8881319857202));
#13917=CARTESIAN_POINT('Ctrl Pts',(-5.33499808860984,0.452558852039112,
19.0270764623274));
#13918=CARTESIAN_POINT('Ctrl Pts',(-4.90132637590066,-2.15502819967951,
19.1660209389346));
#13919=CARTESIAN_POINT('Ctrl Pts',(-3.27293862899549,-4.23729921915194,
19.3049654155417));
#13920=CARTESIAN_POINT('Ctrl Pts',(-0.846835409786463,-5.28680206371619,
19.443909892149));
#13921=CARTESIAN_POINT('Ctrl Pts',(1.78579233672135,-5.0475325547255,19.5828543687561));
#13922=CARTESIAN_POINT('Ctrl Pts',(3.98291872600452,-3.57818693051949,19.7217988453633));
#13923=CARTESIAN_POINT('Ctrl Pts',(5.20971919786745,-1.23606472124711,19.8607491189504));
#13924=CARTESIAN_POINT('Ctrl Pts',(5.18016953017532,0.525504834134071,19.9533845670019));
#13925=CARTESIAN_POINT('Ctrl Pts',(4.95570373216851,1.3496836628856,19.9997051895175));
#13926=CARTESIAN_POINT('Ctrl Pts',(4.95630975100502,1.34951628911715,20.));
#13927=CARTESIAN_POINT('Ctrl Pts',(5.00802755365851,1.211898038485,20.));
#13928=CARTESIAN_POINT('Ctrl Pts',(5.05359491432269,1.07229989795897,20.));
#13929=CARTESIAN_POINT('Ctrl Pts',(5.09309141450286,0.931165512631317,20.));
#13930=CARTESIAN_POINT('Ctrl Pts',(5.13361484558061,0.786361555054366,20.));
#13931=CARTESIAN_POINT('Ctrl Pts',(5.16774795161437,0.639939896759643,20.));
#13932=CARTESIAN_POINT('Ctrl Pts',(5.1955341576068,0.492345209748209,20.));
#13933=CARTESIAN_POINT('Ctrl Pts',(5.22356749502463,0.343437810760418,20.));
#13934=CARTESIAN_POINT('Ctrl Pts',(5.24514076865378,0.193335729449919,20.));
#13935=CARTESIAN_POINT('Ctrl Pts',(5.26025167875134,0.0424704475167592,
20.));
#13936=CARTESIAN_POINT('Ctrl Pts',(5.27537595868635,-0.108528317064509,
20.));
#13937=CARTESIAN_POINT('Ctrl Pts',(5.28402662307941,-0.260292389709474,
20.));
#13938=CARTESIAN_POINT('Ctrl Pts',(5.28615148445568,-0.412403260215922,
20.));
#13939=CARTESIAN_POINT('Ctrl Pts',(5.28676690382088,-0.456458828457367,
20.));
#13940=CARTESIAN_POINT('Ctrl Pts',(5.28683458090809,-0.500543537596189,
20.));
#13941=CARTESIAN_POINT('Ctrl Pts',(5.2863524316627,-0.544647299363032,20.));
#13942=CARTESIAN_POINT('Ctrl Pts',(5.28606370890326,-0.571057710498386,
20.));
#13943=CARTESIAN_POINT('Ctrl Pts',(5.28557781638241,-0.597474953969446,
20.));
#13944=CARTESIAN_POINT('Ctrl Pts',(5.28489424200912,-0.62389686300013,20.));
#13945=CARTESIAN_POINT('Ctrl Pts',(5.2843968262318,-0.643123263128963,20.));
#13946=CARTESIAN_POINT('Ctrl Pts',(5.28379474164197,-0.662350293752617,
20.));
#13947=CARTESIAN_POINT('Ctrl Pts',(5.28308839198291,-0.681565428488897,
20.));
#13948=CARTESIAN_POINT('Ctrl Pts',(5.27736618453607,-0.837229108183571,
20.));
#13949=CARTESIAN_POINT('Ctrl Pts',(5.26480020104454,-0.9923217207242,20.));
#13950=CARTESIAN_POINT('Ctrl Pts',(5.2454298214747,-1.14638516961014,20.));
#13951=CARTESIAN_POINT('Ctrl Pts',(5.24142362338621,-1.17824870084388,20.));
#13952=CARTESIAN_POINT('Ctrl Pts',(5.23712620434838,-1.21006827943255,20.));
#13953=CARTESIAN_POINT('Ctrl Pts',(5.23253765420047,-1.24183995038678,20.));
#13954=CARTESIAN_POINT('Ctrl Pts',(5.21056598904419,-1.39397439223904,20.));
#13955=CARTESIAN_POINT('Ctrl Pts',(5.18192339605888,-1.54500983747171,20.));
#13956=CARTESIAN_POINT('Ctrl Pts',(5.14686314689944,-1.69457665028804,20.));
#13957=CARTESIAN_POINT('Ctrl Pts',(5.11144700718872,-1.84566169006348,20.));
#13958=CARTESIAN_POINT('Ctrl Pts',(5.0694821499338,-1.99524882750055,20.));
#13959=CARTESIAN_POINT('Ctrl Pts',(5.02117633579842,-2.14295818514512,20.));
#13960=CARTESIAN_POINT('Ctrl Pts',(4.97269078910331,-2.29121712841247,20.));
#13961=CARTESIAN_POINT('Ctrl Pts',(4.91781683973363,-2.43758503571107,20.));
#13962=CARTESIAN_POINT('Ctrl Pts',(4.85671337014158,-2.58166803167885,20.));
#13963=CARTESIAN_POINT('Ctrl Pts',(4.84567119665135,-2.60770566013255,20.));
#13964=CARTESIAN_POINT('Ctrl Pts',(4.83442545485886,-2.63366862717467,20.));
#13965=CARTESIAN_POINT('Ctrl Pts',(4.82297691173008,-2.65955454483019,20.));
#13966=CARTESIAN_POINT('Ctrl Pts',(4.81504490372224,-2.6774893426315,20.));
#13967=CARTESIAN_POINT('Ctrl Pts',(4.807016416577,-2.69538508390504,20.));
#13968=CARTESIAN_POINT('Ctrl Pts',(4.79889653142679,-2.71323079035806,20.));
#13969=CARTESIAN_POINT('Ctrl Pts',(4.73305025549089,-2.85794629921556,20.));
#13970=CARTESIAN_POINT('Ctrl Pts',(4.66111448930543,-2.99956115386831,20.));
#13971=CARTESIAN_POINT('Ctrl Pts',(4.58336053077309,-3.1376925483382,20.));
#13972=CARTESIAN_POINT('Ctrl Pts',(4.50473495546917,-3.27737238667349,20.));
#13973=CARTESIAN_POINT('Ctrl Pts',(4.4201598678686,-3.4134909783492,20.));
#13974=CARTESIAN_POINT('Ctrl Pts',(4.32986292961299,-3.54564765538286,20.));
#13975=CARTESIAN_POINT('Ctrl Pts',(4.28143800460734,-3.61652134498943,20.));
#13976=CARTESIAN_POINT('Ctrl Pts',(4.23136657861736,-3.68625543000986,20.));
#13977=CARTESIAN_POINT('Ctrl Pts',(4.17967784234231,-3.75478638155876,20.));
#13978=CARTESIAN_POINT('Ctrl Pts',(4.08363909948493,-3.88211830932257,20.));
#13979=CARTESIAN_POINT('Ctrl Pts',(3.98201968089173,-4.00529850891546,20.));
#13980=CARTESIAN_POINT('Ctrl Pts',(3.87518106995263,-4.12409405024153,20.));
#13981=CARTESIAN_POINT('Ctrl Pts',(3.7790674283499,-4.23096432853,20.));
#13982=CARTESIAN_POINT('Ctrl Pts',(3.67872896688893,-4.33428603353984,20.));
#13983=CARTESIAN_POINT('Ctrl Pts',(3.57440019418943,-4.43386776444262,20.));
#13984=CARTESIAN_POINT('Ctrl Pts',(3.55912119418721,-4.44845155784223,20.));
#13985=CARTESIAN_POINT('Ctrl Pts',(3.54376310959292,-4.46294883322329,20.));
#13986=CARTESIAN_POINT('Ctrl Pts',(3.52832963421354,-4.47735661404417,20.));
#13987=CARTESIAN_POINT('Ctrl Pts',(3.40931164145479,-4.58846478062726,20.));
#13988=CARTESIAN_POINT('Ctrl Pts',(3.28576263570275,-4.69430173361665,20.));
#13989=CARTESIAN_POINT('Ctrl Pts',(3.15811578368783,-4.7946678411415,20.));
#13990=CARTESIAN_POINT('Ctrl Pts',(3.02925981578756,-4.89598465174318,20.));
#13991=CARTESIAN_POINT('Ctrl Pts',(2.89622752993871,-4.99172703492966,20.));
#13992=CARTESIAN_POINT('Ctrl Pts',(2.75941743654065,-5.08166364708008,20.));
#13993=CARTESIAN_POINT('Ctrl Pts',(2.62247809700501,-5.1716852234277,20.));
#13994=CARTESIAN_POINT('Ctrl Pts',(2.48175325925716,-5.25589059093984,20.));
#13995=CARTESIAN_POINT('Ctrl Pts',(2.33760340461929,-5.33401368905513,20.));
#13996=CARTESIAN_POINT('Ctrl Pts',(2.21232042361525,-5.40191174307497,20.));
#13997=CARTESIAN_POINT('Ctrl Pts',(2.08444948553081,-5.46521516943517,20.));
#13998=CARTESIAN_POINT('Ctrl Pts',(1.95420814809202,-5.52372361795384,20.));
#13999=CARTESIAN_POINT('Ctrl Pts',(1.89742161393368,-5.54923389046558,20.));
#14000=CARTESIAN_POINT('Ctrl Pts',(1.84018425350229,-5.57383227726414,20.));
#14001=CARTESIAN_POINT('Ctrl Pts',(1.78251853632916,-5.59751523771367,20.));
#14002=CARTESIAN_POINT('Ctrl Pts',(1.75691956432136,-5.60802858032569,20.));
#14003=CARTESIAN_POINT('Ctrl Pts',(1.73123617245675,-5.6183615112354,20.));
#14004=CARTESIAN_POINT('Ctrl Pts',(1.70547030102192,-5.62851365711605,20.));
#14005=CARTESIAN_POINT('Ctrl Pts',(1.68482728538373,-5.63664731976764,20.));
#14006=CARTESIAN_POINT('Ctrl Pts',(1.66413268935087,-5.64466435227788,20.));
#14007=CARTESIAN_POINT('Ctrl Pts',(1.64339888368342,-5.65256041345011,20.));
#14008=CARTESIAN_POINT('Ctrl Pts',(1.4887528735376,-5.71145429794664,20.));
#14009=CARTESIAN_POINT('Ctrl Pts',(1.33175860111718,-5.76368915521618,20.));
#14010=CARTESIAN_POINT('Ctrl Pts',(1.17288405441337,-5.80928192680759,20.));
#14011=CARTESIAN_POINT('Ctrl Pts',(1.0117104916612,-5.85553445489085,20.));
#14012=CARTESIAN_POINT('Ctrl Pts',(0.848601209939264,-5.89495157525683,
20.));
#14013=CARTESIAN_POINT('Ctrl Pts',(0.684016067746065,-5.92750558887808,
20.));
#14014=CARTESIAN_POINT('Ctrl Pts',(0.561129089048119,-5.95181194074616,
20.));
#14015=CARTESIAN_POINT('Ctrl Pts',(0.437418685281485,-5.97229131717515,
20.));
#14016=CARTESIAN_POINT('Ctrl Pts',(0.313069360631807,-5.98891456741767,
20.));
#14017=CARTESIAN_POINT('Ctrl Pts',(0.286181878098548,-5.99250893636018,
20.));
#14018=CARTESIAN_POINT('Ctrl Pts',(0.259274152325606,-5.99592166155524,
20.));
#14019=CARTESIAN_POINT('Ctrl Pts',(0.232350196748965,-5.99915251615709,
20.));
#14020=CARTESIAN_POINT('Ctrl Pts',(0.0633272905923215,-6.01943513891737,
20.));
#14021=CARTESIAN_POINT('Ctrl Pts',(-0.106359787945285,-6.03255750685238,
20.));
#14022=CARTESIAN_POINT('Ctrl Pts',(-0.276237342802518,-6.03850393719931,
20.));
#14023=CARTESIAN_POINT('Ctrl Pts',(-0.446444855390507,-6.04446191745738,
20.));
#14024=CARTESIAN_POINT('Ctrl Pts',(-0.61684432643634,-6.04321626583662,
20.));
#14025=CARTESIAN_POINT('Ctrl Pts',(-0.786975461233458,-6.03470182931886,
20.));
#14026=CARTESIAN_POINT('Ctrl Pts',(-0.846277277337399,-6.03173399189624,
20.));
#14027=CARTESIAN_POINT('Ctrl Pts',(-0.90554658260626,-6.02788255987274,
20.));
#14028=CARTESIAN_POINT('Ctrl Pts',(-0.964764086495351,-6.02314329455464,
20.));
#14029=CARTESIAN_POINT('Ctrl Pts',(-1.02320302808891,-6.01846633874036,
20.));
#14030=CARTESIAN_POINT('Ctrl Pts',(-1.08159152517642,-6.01292474055862,
20.));
#14031=CARTESIAN_POINT('Ctrl Pts',(-1.13991297760764,-6.00652560023185,
20.));
#14032=CARTESIAN_POINT('',(-3.88011837732335,-3.36643235951024,-0.00012510356376383));
#14033=CARTESIAN_POINT('Ctrl Pts',(-3.87712761685009,-3.36958187393604,
0.));
#14034=CARTESIAN_POINT('Ctrl Pts',(-3.87807635419917,-3.36849023232742,
-4.17011879212766E-5));
#14035=CARTESIAN_POINT('Ctrl Pts',(-3.87902463050534,-3.36739819002994,
-8.34023758425532E-5));
#14036=CARTESIAN_POINT('Ctrl Pts',(-3.87997244543031,-3.36630574743317,
-0.00012510356376383));
#14037=CARTESIAN_POINT('Ctrl Pts',(-1.5788818818754,5.90584097022478,2.71050543121376E-20));
#14038=CARTESIAN_POINT('Ctrl Pts',(-1.73738372178013,5.84977611874637,1.41954999535879E-15));
#14039=CARTESIAN_POINT('Ctrl Pts',(-1.89317454668904,5.78715364031114,-1.62634446731416E-15));
#14040=CARTESIAN_POINT('Ctrl Pts',(-2.04591809998494,5.71826166590681,-1.90819582357449E-15));
#14041=CARTESIAN_POINT('Ctrl Pts',(-2.20036694327166,5.6486005540046,-2.19319388086643E-15));
#14042=CARTESIAN_POINT('Ctrl Pts',(-2.35170073198387,5.57252876729252,-1.64505916368078E-15));
#14043=CARTESIAN_POINT('Ctrl Pts',(-2.49954705832695,5.49029744531603,-2.67841304690819E-15));
#14044=CARTESIAN_POINT('Ctrl Pts',(-2.64691768285296,5.40833070610091,-3.70844207024844E-15));
#14045=CARTESIAN_POINT('Ctrl Pts',(-2.79082382020564,5.32024350753178,-1.82369499736428E-15));
#14046=CARTESIAN_POINT('Ctrl Pts',(-2.93086319241294,5.22624534364585,9.71445146547012E-17));
#14047=CARTESIAN_POINT('Ctrl Pts',(-3.06866119336755,5.13375164796069,1.98724042653163E-15));
#14048=CARTESIAN_POINT('Ctrl Pts',(-3.20271565751252,5.03553416804527,6.50016582170925E-16));
#14049=CARTESIAN_POINT('Ctrl Pts',(-3.33260352332624,4.93176207959357,1.49880108324396E-15));
#14050=CARTESIAN_POINT('Ctrl Pts',(-3.39649124541486,4.88071988018546,1.9162912620067E-15));
#14051=CARTESIAN_POINT('Ctrl Pts',(-3.45937026984301,4.82833340907307,1.89993404248056E-15));
#14052=CARTESIAN_POINT('Ctrl Pts',(-3.52118613976384,4.77462059891634,1.4432899320127E-15));
#14053=CARTESIAN_POINT('Ctrl Pts',(-3.5392354254394,4.7589372823797,1.30251253808548E-15));
#14054=CARTESIAN_POINT('Ctrl Pts',(-3.55719405290947,4.74314088034149,2.3520270366554E-16));
#14055=CARTESIAN_POINT('Ctrl Pts',(-3.57506061886072,4.72723181907044,1.62370117351429E-15));
#14056=CARTESIAN_POINT('Ctrl Pts',(-3.5909387783033,4.71309330962589,3.67955640940023E-15));
#14057=CARTESIAN_POINT('Ctrl Pts',(-3.60673813814453,4.69887122125484,1.47731149873469E-15));
#14058=CARTESIAN_POINT('Ctrl Pts',(-3.62245453970707,4.68456914621453,1.67921232474555E-15));
#14059=CARTESIAN_POINT('Ctrl Pts',(-3.74459274110421,4.57342222020102,2.48255805465195E-15));
#14060=CARTESIAN_POINT('Ctrl Pts',(-3.86179045770333,4.45738819529234,1.89396572533195E-15));
#14061=CARTESIAN_POINT('Ctrl Pts',(-3.97369545139774,4.33669080159381,3.10862446895044E-15));
#14062=CARTESIAN_POINT('Ctrl Pts',(-3.99821750982727,4.31024203963195,3.70849224798273E-15));
#14063=CARTESIAN_POINT('Ctrl Pts',(-4.02248527033337,4.28356921164166,2.25584676567993E-15));
#14064=CARTESIAN_POINT('Ctrl Pts',(-4.04649477136385,4.25667445357649,2.24820162486594E-15));
#14065=CARTESIAN_POINT('Ctrl Pts',(-4.15647220143564,4.13348087405744,2.10178287836601E-15));
#14066=CARTESIAN_POINT('Ctrl Pts',(-4.26103452091919,4.00563289035671,3.48538070402028E-16));
#14067=CARTESIAN_POINT('Ctrl Pts',(-4.35997112081345,3.87353532936375,1.69309011255336E-15));
#14068=CARTESIAN_POINT('Ctrl Pts',(-4.45871887377264,3.74168991186016,1.25126370824338E-15));
#14069=CARTESIAN_POINT('Ctrl Pts',(-4.55186264529244,3.60561039414627,1.98141016501602E-15));
#14070=CARTESIAN_POINT('Ctrl Pts',(-4.63914521870387,3.46567967142402,2.08166817117217E-15));
#14071=CARTESIAN_POINT('Ctrl Pts',(-4.72248228550573,3.33207435330206,3.79683147803274E-15));
#14072=CARTESIAN_POINT('Ctrl Pts',(-4.80047597977778,3.19495747398172,2.49449903000048E-16));
#14073=CARTESIAN_POINT('Ctrl Pts',(-4.8728580206208,3.05465465625189,2.80331313717852E-15));
#14074=CARTESIAN_POINT('Ctrl Pts',(-4.8935934643793,3.01446179691395,2.71989202312118E-15));
#14075=CARTESIAN_POINT('Ctrl Pts',(-4.91386809532294,2.9740074624354,-1.98418256427254E-15));
#14076=CARTESIAN_POINT('Ctrl Pts',(-4.93367490701556,2.93329929699418,-7.49400541621981E-16));
#14077=CARTESIAN_POINT('Ctrl Pts',(-4.95079469490032,2.89811366649765,9.45444324111637E-16));
#14078=CARTESIAN_POINT('Ctrl Pts',(-4.96755007806123,2.86276890738097,7.94867220024555E-16));
#14079=CARTESIAN_POINT('Ctrl Pts',(-4.98393512137525,2.82727792454592,6.66133814775094E-16));
#14080=CARTESIAN_POINT('Ctrl Pts',(-5.05163794692084,2.68062955912676,1.34208746866495E-16));
#14081=CARTESIAN_POINT('Ctrl Pts',(-5.11304163000182,2.53144510009992,-1.76889492459881E-15));
#14082=CARTESIAN_POINT('Ctrl Pts',(-5.16794971273575,2.38010471812791,-2.35922392732846E-15));
#14083=CARTESIAN_POINT('Ctrl Pts',(-5.22236412788884,2.23012500723624,-2.94424540016139E-15));
#14084=CARTESIAN_POINT('Ctrl Pts',(-5.27039939637123,2.07802726364688,2.92689554064512E-16));
#14085=CARTESIAN_POINT('Ctrl Pts',(-5.31181481886995,1.92416985016893,-2.16493489801906E-15));
#14086=CARTESIAN_POINT('Ctrl Pts',(-5.32933332980379,1.85908895475255,-3.20449741452864E-15));
#14087=CARTESIAN_POINT('Ctrl Pts',(-5.34566676203086,1.79369312832893,-5.30184591639501E-15));
#14088=CARTESIAN_POINT('Ctrl Pts',(-5.36079407817689,1.72800931712517,-4.9960036108132E-15));
#14089=CARTESIAN_POINT('Ctrl Pts',(-5.39677766745839,1.57176618305015,-4.14671790720287E-15));
#14090=CARTESIAN_POINT('Ctrl Pts',(-5.4259401021884,1.41389282238529,-6.4852137940373E-15));
#14091=CARTESIAN_POINT('Ctrl Pts',(-5.44823692450669,1.25484161090092,-6.10622663543836E-15));
#14092=CARTESIAN_POINT('Ctrl Pts',(-5.46658493932396,1.12395865621973,-5.79435878708482E-15));
#14093=CARTESIAN_POINT('Ctrl Pts',(-5.48028287698849,0.992277986873389,
-5.87332885153964E-15));
#14094=CARTESIAN_POINT('Ctrl Pts',(-5.48928060351323,0.86005942044192,-4.6074255521944E-15));
#14095=CARTESIAN_POINT('Ctrl Pts',(-5.49103894671333,0.83422115823499,-3.71615202053864E-15));
#14096=CARTESIAN_POINT('Ctrl Pts',(-5.49261785043889,0.808358691214049,
-6.19489801465623E-15));
#14097=CARTESIAN_POINT('Ctrl Pts',(-5.49401562173337,0.782500543343462,
-5.99520433297585E-15));
#14098=CARTESIAN_POINT('Ctrl Pts',(-5.50252562943416,0.625069182163987,
-4.45309984798879E-15));
#14099=CARTESIAN_POINT('Ctrl Pts',(-5.50434062410808,0.467610134203912,
-8.25842126848828E-15));
#14100=CARTESIAN_POINT('Ctrl Pts',(-5.49949281171653,0.310550407416323,
-7.38298311375729E-15));
#14101=CARTESIAN_POINT('Ctrl Pts',(-5.49465821572017,0.1539188662209,-5.31715605658429E-15));
#14102=CARTESIAN_POINT('Ctrl Pts',(-5.48319695438002,-0.00231628880926202,
-7.47697400666613E-15));
#14103=CARTESIAN_POINT('Ctrl Pts',(-5.46508984137315,-0.157724420450921,
-6.82787160144471E-15));
#14104=CARTESIAN_POINT('Ctrl Pts',(-5.44729560717373,-0.310447203474091,
-6.19858210290864E-15));
#14105=CARTESIAN_POINT('Ctrl Pts',(-5.42308297461965,-0.462371946136479,
-5.20478416826247E-15));
#14106=CARTESIAN_POINT('Ctrl Pts',(-5.39238722509327,-0.613072707074315,
-4.88498130835069E-15));
#14107=CARTESIAN_POINT('Ctrl Pts',(-5.36573616835424,-0.74391605158746,
-6.47002664417425E-15));
#14108=CARTESIAN_POINT('Ctrl Pts',(-5.33419720831201,-0.873836721881379,
-7.00556211049708E-15));
#14109=CARTESIAN_POINT('Ctrl Pts',(-5.29770061351415,-1.00253949229394,
-5.93969318174459E-15));
#14110=CARTESIAN_POINT('Ctrl Pts',(-5.27375172934145,-1.08699361077776,
-5.19880832617926E-15));
#14111=CARTESIAN_POINT('Ctrl Pts',(-5.24766752212855,-1.17092296801775,
-3.77798944519056E-15));
#14112=CARTESIAN_POINT('Ctrl Pts',(-5.21947367702465,-1.25424893059207,
-2.72004641033163E-15));
#14113=CARTESIAN_POINT('Ctrl Pts',(-5.2123588272694,-1.27527663015708,-3.14869267684114E-15));
#14114=CARTESIAN_POINT('Ctrl Pts',(-5.2051112968655,-1.29626080812995,-1.79997908153132E-15));
#14115=CARTESIAN_POINT('Ctrl Pts',(-5.19773424300509,-1.31719316713618,
-1.83186799063151E-15));
#14116=CARTESIAN_POINT('Ctrl Pts',(-5.1464013431419,-1.4628500525406,-2.22845850964274E-15));
#14117=CARTESIAN_POINT('Ctrl Pts',(-5.08876458161359,-1.60610680701176,
-4.14750974226397E-15));
#14118=CARTESIAN_POINT('Ctrl Pts',(-5.02504407081273,-1.74657685516349,
-4.94049245958195E-15));
#14119=CARTESIAN_POINT('Ctrl Pts',(-4.96146013005027,-1.88674583856183,
-2.94724036326532E-15));
#14120=CARTESIAN_POINT('Ctrl Pts',(-4.89181800426118,-2.0241406789921,1.03279346409245E-15));
#14121=CARTESIAN_POINT('Ctrl Pts',(-4.81629593366406,-2.15834507337917,
2.77555756156289E-16));
#14122=CARTESIAN_POINT('Ctrl Pts',(-4.78797515719014,-2.2086717212743,-8.92932335639387E-16));
#14123=CARTESIAN_POINT('Ctrl Pts',(-4.75882714255844,-2.25854933938649,
1.37195633263433E-15));
#14124=CARTESIAN_POINT('Ctrl Pts',(-4.72886002942117,-2.30795452599388,
1.94289029309402E-15));
#14125=CARTESIAN_POINT('Ctrl Pts',(-4.70988523951568,-2.33923725355665,
2.20939297049903E-15));
#14126=CARTESIAN_POINT('Ctrl Pts',(-4.69058154214804,-2.37033133499752,
4.07705897209819E-15));
#14127=CARTESIAN_POINT('Ctrl Pts',(-4.67095240483681,-2.40122824167162,
2.33146835171283E-15));
#14128=CARTESIAN_POINT('Ctrl Pts',(-4.65361468426418,-2.42851838315778,
7.89650087842628E-16));
#14129=CARTESIAN_POINT('Ctrl Pts',(-4.63602837970922,-2.45564625457261,
1.85008738298638E-15));
#14130=CARTESIAN_POINT('Ctrl Pts',(-4.61820068354681,-2.48260005722413,
1.99840144432528E-15));
#14131=CARTESIAN_POINT('Ctrl Pts',(-4.53479193651534,-2.60870625100355,
2.69230434185812E-15));
#14132=CARTESIAN_POINT('Ctrl Pts',(-4.446064923331,-2.73106380349622,4.08197270232755E-15));
#14133=CARTESIAN_POINT('Ctrl Pts',(-4.3522011455562,-2.84928146336898,3.21964677141295E-15));
#14134=CARTESIAN_POINT('Ctrl Pts',(-4.25980099053161,-2.96565574914612,
2.37076713341881E-15));
#14135=CARTESIAN_POINT('Ctrl Pts',(-4.16242250621293,-3.07801870175783,
-2.96586265836701E-15));
#14136=CARTESIAN_POINT('Ctrl Pts',(-4.06020849653285,-3.18595684819616,
2.55351295663786E-15));
#14137=CARTESIAN_POINT('Ctrl Pts',(-4.03579916371253,-3.21173314000457,
3.87157372706141E-15));
#14138=CARTESIAN_POINT('Ctrl Pts',(-4.01111395005447,-3.23725689213896,
5.18084404389532E-15));
#14139=CARTESIAN_POINT('Ctrl Pts',(-3.98615458747356,-3.26252208283929,
5.77315972805081E-15));
#14140=CARTESIAN_POINT('Ctrl Pts',(-3.95139310944715,-3.29770949471794,
6.56610875245429E-15));
#14141=CARTESIAN_POINT('Ctrl Pts',(-3.91609987445632,-3.33239540188103,
3.68058791726313E-15));
#14142=CARTESIAN_POINT('Ctrl Pts',(-3.88028720092977,-3.36656946842384,
5.55111512312578E-16));
#14143=CARTESIAN_POINT('Origin',(0.,0.,20.));
#14144=CARTESIAN_POINT('',(-12.,-1.46957615897682E-15,20.));
#14145=CARTESIAN_POINT('Origin',(0.,0.,20.));
#14146=CARTESIAN_POINT('Origin',(0.,0.,0.));
#14147=CARTESIAN_POINT('',(-12.,-1.46957615897682E-15,0.));
#14148=CARTESIAN_POINT('',(-12.,-1.46957615897682E-15,0.));
#14149=CARTESIAN_POINT('Origin',(0.,0.,0.));
#14150=CARTESIAN_POINT('Origin',(0.,0.,0.));
#14151=CARTESIAN_POINT('',(0.,0.,0.));
#14152=CARTESIAN_POINT('Origin',(0.,0.,0.));
#14153=CARTESIAN_POINT('',(-6.5,-7.9602041944578E-16,0.));
#14154=CARTESIAN_POINT('Origin',(0.,0.,0.));
#14155=CARTESIAN_POINT('',(-6.5,-7.9602041944578E-16,2.));
#14156=CARTESIAN_POINT('',(-6.5,-7.9602041944578E-16,0.));
#14157=CARTESIAN_POINT('Origin',(0.,0.,2.));
#14158=CARTESIAN_POINT('Origin',(0.,0.,0.));
#14159=CARTESIAN_POINT('',(-12.,-1.46957615897682E-15,2.));
#14160=CARTESIAN_POINT('Origin',(0.,0.,2.));
#14161=CARTESIAN_POINT('',(-12.,-1.46957615897682E-15,0.));
#14162=CARTESIAN_POINT('',(-12.,-1.46957615897682E-15,0.));
#14163=CARTESIAN_POINT('Origin',(0.,0.,0.));
#14164=CARTESIAN_POINT('Origin',(0.,0.,2.));
#14165=CARTESIAN_POINT('Origin',(0.,0.,0.));
#14166=CARTESIAN_POINT('',(0.,0.,0.));
#14167=CARTESIAN_POINT('Origin',(0.,0.,0.));
#14168=CARTESIAN_POINT('',(-5.91674999809507,0.000150139963024017,0.56337519223592));
#14169=CARTESIAN_POINT('',(-5.91671935081961,9.79311290895061E-5,0.311624807795122));
#14170=CARTESIAN_POINT('',(-5.91675,-7.2459289488551E-16,0.));
#14171=CARTESIAN_POINT('',(2.58392005625187,5.32271431746993,5.66418127782893E-6));
#14172=CARTESIAN_POINT('Ctrl Pts',(-5.91674999809505,0.000150140621988509,
0.563375192204898));
#14173=CARTESIAN_POINT('Ctrl Pts',(-5.91674553653358,0.175971603634398,
0.555097989792623));
#14174=CARTESIAN_POINT('Ctrl Pts',(-5.90889970267472,0.35175539283155,0.546820787380347));
#14175=CARTESIAN_POINT('Ctrl Pts',(-5.8932485072967,0.526832605051395,0.538543584968072));
#14176=CARTESIAN_POINT('Ctrl Pts',(-5.89144091145379,0.547052711781432,
0.53758763008348));
#14177=CARTESIAN_POINT('Ctrl Pts',(-5.8895292606626,0.567263397909551,0.536631675198887));
#14178=CARTESIAN_POINT('Ctrl Pts',(-5.88751365503158,0.587463636590923,
0.535675720314295));
#14179=CARTESIAN_POINT('Ctrl Pts',(-5.87109213436944,0.752038805355124,
0.527887374892031));
#14180=CARTESIAN_POINT('Ctrl Pts',(-5.84776274299796,0.915954366421261,
0.520099029469766));
#14181=CARTESIAN_POINT('Ctrl Pts',(-5.81760272669442,1.07862369566856,0.512310684047502));
#14182=CARTESIAN_POINT('Ctrl Pts',(-5.78744863648316,1.24126106228533,0.504523868944495));
#14183=CARTESIAN_POINT('Ctrl Pts',(-5.75046665751305,1.4026523717289,0.496737053841489));
#14184=CARTESIAN_POINT('Ctrl Pts',(-5.70678536019788,1.56222002775893,0.488950238738483));
#14185=CARTESIAN_POINT('Ctrl Pts',(-5.66310240888906,1.72179372582311,0.481163128787486));
#14186=CARTESIAN_POINT('Ctrl Pts',(-5.61271971217538,1.87954332311285,0.473376018836489));
#14187=CARTESIAN_POINT('Ctrl Pts',(-5.55581624327961,2.03490452685388,0.465588908885492));
#14188=CARTESIAN_POINT('Ctrl Pts',(-5.49891655207064,2.1902554165318,0.457802315902319));
#14189=CARTESIAN_POINT('Ctrl Pts',(-5.43549706495836,2.34321792997301,0.450015722919146));
#14190=CARTESIAN_POINT('Ctrl Pts',(-5.36578566692213,2.49324582405207,0.442229129935973));
#14191=CARTESIAN_POINT('Ctrl Pts',(-5.29605597837102,2.64331308167145,0.43444049394694));
#14192=CARTESIAN_POINT('Ctrl Pts',(-5.22003121311526,2.79044389061004,0.426651857957906));
#14193=CARTESIAN_POINT('Ctrl Pts',(-5.13798656155565,2.93411394730564,0.418863221968873));
#14194=CARTESIAN_POINT('Ctrl Pts',(-5.06000943480969,3.07066127863795,0.411460722913175));
#14195=CARTESIAN_POINT('Ctrl Pts',(-4.97659498598521,3.20408246256618,0.404058223857477));
#14196=CARTESIAN_POINT('Ctrl Pts',(-4.88801705550324,3.33394958384338,0.396655724801779));
#14197=CARTESIAN_POINT('Ctrl Pts',(-4.79483107421496,3.47057272538046,0.388868128786187));
#14198=CARTESIAN_POINT('Ctrl Pts',(-4.69589676366777,3.60331097514271,0.381080532770595));
#14199=CARTESIAN_POINT('Ctrl Pts',(-4.59156266393042,3.73168633002564,0.373292936755003));
#14200=CARTESIAN_POINT('Ctrl Pts',(-4.48724907892953,3.86003644305015,0.365506871978769));
#14201=CARTESIAN_POINT('Ctrl Pts',(-4.37753802466603,3.98402512499211,0.357720807202535));
#14202=CARTESIAN_POINT('Ctrl Pts',(-4.26281878373472,4.10320686531138,0.349934742426301));
#14203=CARTESIAN_POINT('Ctrl Pts',(-4.14809511398164,4.22239320673053,0.342148377063235));
#14204=CARTESIAN_POINT('Ctrl Pts',(-4.02836308946995,4.33677200218623,0.33436201170017));
#14205=CARTESIAN_POINT('Ctrl Pts',(-3.90404987928167,4.44593354680216,0.326575646337105));
#14206=CARTESIAN_POINT('Ctrl Pts',(-3.77974484877771,4.55508790869813,0.318789793309057));
#14207=CARTESIAN_POINT('Ctrl Pts',(-3.65085947608667,4.65902549591907,0.311003940281009));
#14208=CARTESIAN_POINT('Ctrl Pts',(-3.51785523433146,4.75737586414892,0.303218087252961));
#14209=CARTESIAN_POINT('Ctrl Pts',(-3.38481584030573,4.85575222582609,0.295430176467895));
#14210=CARTESIAN_POINT('Ctrl Pts',(-3.24765565797162,4.94853822608719,0.287642265682829));
#14211=CARTESIAN_POINT('Ctrl Pts',(-3.1068671924737,5.03540532736249,0.279854354897763));
#14212=CARTESIAN_POINT('Ctrl Pts',(-2.9729790723165,5.11801488526997,0.272448146361596));
#14213=CARTESIAN_POINT('Ctrl Pts',(-2.8358100372979,5.19527170903417,0.265041937825429));
#14214=CARTESIAN_POINT('Ctrl Pts',(-2.69580607650546,5.26693081028945,0.257635729289262));
#14215=CARTESIAN_POINT('Ctrl Pts',(-2.54858704760487,5.34228284489603,0.24984784370118));
#14216=CARTESIAN_POINT('Ctrl Pts',(-2.39818035191975,5.41147200648169,0.242059958113099));
#14217=CARTESIAN_POINT('Ctrl Pts',(-2.24512084427557,5.4742454235355,0.234272072525018));
#14218=CARTESIAN_POINT('Ctrl Pts',(-2.09209149064525,5.53700647369674,0.226485721216078));
#14219=CARTESIAN_POINT('Ctrl Pts',(-1.93641066333322,5.59335418010095,0.218699369907139));
#14220=CARTESIAN_POINT('Ctrl Pts',(-1.77863343642197,5.64308370142972,0.210913018598199));
#14221=CARTESIAN_POINT('Ctrl Pts',(-1.62085026853532,5.69281509528388,0.203126374100423));
#14222=CARTESIAN_POINT('Ctrl Pts',(-1.46097084667463,5.73592770555686,0.195339729602648));
#14223=CARTESIAN_POINT('Ctrl Pts',(-1.29956637043957,5.77226626303071,0.187553085104872));
#14224=CARTESIAN_POINT('Ctrl Pts',(-1.1381726094073,5.80860240808688,0.179766957541179));
#14225=CARTESIAN_POINT('Ctrl Pts',(-0.975254308416725,5.83816533018435,
0.171980829977485));
#14226=CARTESIAN_POINT('Ctrl Pts',(-0.811393994756377,5.86085065052619,
0.164194702413792));
#14227=CARTESIAN_POINT('Ctrl Pts',(-0.647490590330721,5.88354193648468,
0.156406527312241));
#14228=CARTESIAN_POINT('Ctrl Pts',(-0.482644994721619,5.89935196088901,
0.148618352210691));
#14229=CARTESIAN_POINT('Ctrl Pts',(-0.317446922897937,5.90822799269313,
0.14083017710914));
#14230=CARTESIAN_POINT('Ctrl Pts',(-0.160380466066584,5.91666711580639,
0.133425362665008));
#14231=CARTESIAN_POINT('Ctrl Pts',(-0.00299566183749642,5.91883844420629,
0.126020548220876));
#14232=CARTESIAN_POINT('Ctrl Pts',(0.154198948809147,5.91474033637033,0.118615733776744));
#14233=CARTESIAN_POINT('Ctrl Pts',(0.318899201834896,5.91044655432059,0.110857358298474));
#14234=CARTESIAN_POINT('Ctrl Pts',(0.483453641539656,5.89926825531666,0.103098982820203));
#14235=CARTESIAN_POINT('Ctrl Pts',(0.647275897512335,5.88123834536568,0.0953406073419322));
#14236=CARTESIAN_POINT('Ctrl Pts',(0.815029932118198,5.86277571267942,0.087396028745211));
#14237=CARTESIAN_POINT('Ctrl Pts',(0.982015844042426,5.83712845066767,0.0794514501484898));
#14238=CARTESIAN_POINT('Ctrl Pts',(1.14760928393256,5.80438829627479,0.0715068715517686));
#14239=CARTESIAN_POINT('Ctrl Pts',(1.30928459978979,5.77242281016499,0.0637502704760876));
#14240=CARTESIAN_POINT('Ctrl Pts',(1.46963226790649,5.73369638273858,0.0559936694004065));
#14241=CARTESIAN_POINT('Ctrl Pts',(1.62808103688705,5.68834621835106,0.0482370683247255));
#14242=CARTESIAN_POINT('Ctrl Pts',(1.79228970118404,5.64134749461445,0.0401985009674842));
#14243=CARTESIAN_POINT('Ctrl Pts',(1.95445845105966,5.58723448296605,0.0321599336102429));
#14244=CARTESIAN_POINT('Ctrl Pts',(2.11396789947378,5.52621663369202,0.0241213662530017));
#14245=CARTESIAN_POINT('Ctrl Pts',(2.2734773478879,5.465198784418,0.0160827988957604));
#14246=CARTESIAN_POINT('Ctrl Pts',(2.43032713552487,5.39727624296388,0.00804423153851909));
#14247=CARTESIAN_POINT('Ctrl Pts',(2.58392005625187,5.32271431746993,5.66418127782893E-6));
#14248=CARTESIAN_POINT('',(-2.58391981634392,5.32271443393361,2.77555756156289E-16));
#14249=CARTESIAN_POINT('Origin',(0.,0.,0.));
#14250=CARTESIAN_POINT('Ctrl Pts',(-2.58391981634392,5.32271443393361,-4.44089209850063E-15));
#14251=CARTESIAN_POINT('Ctrl Pts',(-3.46903743297636,4.89303274091792,0.0463154617617043));
#14252=CARTESIAN_POINT('Ctrl Pts',(-5.01988689220886,3.58402595494104,0.138946385285122));
#14253=CARTESIAN_POINT('Ctrl Pts',(-5.84431863508223,1.46158823788899,0.24282132121683));
#14254=CARTESIAN_POINT('Ctrl Pts',(-5.91696259478107,0.238957375009801,
0.300380795386831));
#14255=CARTESIAN_POINT('Ctrl Pts',(-5.91671935081961,9.79311290895061E-5,
0.311624807795122));
#14256=CARTESIAN_POINT('Origin',(0.,0.,0.));
#14257=CARTESIAN_POINT('',(-5.91674999805022,-0.000151897061178456,2.3133751922049));
#14258=CARTESIAN_POINT('',(-5.91696061209103,-0.000135486519901937,2.06162480779511));
#14259=CARTESIAN_POINT('',(-5.91675,-7.2459289488551E-16,0.));
#14260=CARTESIAN_POINT('Ctrl Pts',(-5.91674999805022,-0.000151897061178456,
2.3133751922049));
#14261=CARTESIAN_POINT('Ctrl Pts',(-5.91675422850432,0.164634301711275,
2.30561771325954));
#14262=CARTESIAN_POINT('Ctrl Pts',(-5.90986997597158,0.329443911336745,
2.29786023431418));
#14263=CARTESIAN_POINT('Ctrl Pts',(-5.8961174422526,0.493689851692964,2.29010275536882));
#14264=CARTESIAN_POINT('Ctrl Pts',(-5.88236474983525,0.657937687377254,
2.28234518690546));
#14265=CARTESIAN_POINT('Ctrl Pts',(-5.86174364025453,0.821621517221492,
2.2745876184421));
#14266=CARTESIAN_POINT('Ctrl Pts',(-5.83432629786468,0.984158123750763,
2.26683004997874));
#14267=CARTESIAN_POINT('Ctrl Pts',(-5.80691054692563,1.14668529577654,2.2590729318066));
#14268=CARTESIAN_POINT('Ctrl Pts',(-5.77269940695638,1.30806505797604,2.25131581363446));
#14269=CARTESIAN_POINT('Ctrl Pts',(-5.7318164437995,1.46772300421083,2.24355869546232));
#14270=CARTESIAN_POINT('Ctrl Pts',(-5.69092326768429,1.62742083453978,2.23579963948728));
#14271=CARTESIAN_POINT('Ctrl Pts',(-5.64335501802441,1.78539567494315,2.22804058351223));
#14272=CARTESIAN_POINT('Ctrl Pts',(-5.58928574077949,1.94108615739205,2.22028152753719));
#14273=CARTESIAN_POINT('Ctrl Pts',(-5.55127036526057,2.05055002405717,2.21482624051296));
#14274=CARTESIAN_POINT('Ctrl Pts',(-5.5100423893398,2.15888493851147,2.20937095348874));
#14275=CARTESIAN_POINT('Ctrl Pts',(-5.46567681880059,2.2659010293757,2.20391566646451));
#14276=CARTESIAN_POINT('Ctrl Pts',(-5.40234044819479,2.41867739874011,2.19612768861303));
#14277=CARTESIAN_POINT('Ctrl Pts',(-5.332583141542,2.5688238602527,2.18833971076156));
#14278=CARTESIAN_POINT('Ctrl Pts',(-5.25664854959036,2.71580127928932,2.18055173291008));
#14279=CARTESIAN_POINT('Ctrl Pts',(-5.18072888702907,2.86274980130808,2.17276528624167));
#14280=CARTESIAN_POINT('Ctrl Pts',(-5.09863450905242,3.00653024031549,2.16497883957326));
#14281=CARTESIAN_POINT('Ctrl Pts',(-5.01065558369874,3.14662695342944,2.15719239290485));
#14282=CARTESIAN_POINT('Ctrl Pts',(-4.92267330215496,3.28672901090513,2.14940564920172));
#14283=CARTESIAN_POINT('Ctrl Pts',(-4.82880619062974,3.42314678858581,2.14161890549859));
#14284=CARTESIAN_POINT('Ctrl Pts',(-4.72938881488245,3.5553919615374,2.13383216179546));
#14285=CARTESIAN_POINT('Ctrl Pts',(-4.62997801485764,3.68762838745105,2.12604593312772));
#14286=CARTESIAN_POINT('Ctrl Pts',(-4.52501787737567,3.81569250555002,2.11825970445997));
#14287=CARTESIAN_POINT('Ctrl Pts',(-4.4148845648174,3.93912742137609,2.11047347579222));
#14288=CARTESIAN_POINT('Ctrl Pts',(-4.30472226008525,4.06259483097229,2.10268519742951));
#14289=CARTESIAN_POINT('Ctrl Pts',(-4.18938427050191,4.18143036333759,2.0948969190668));
#14290=CARTESIAN_POINT('Ctrl Pts',(-4.0692856919947,4.29521181310389,2.08710864070409));
#14291=CARTESIAN_POINT('Ctrl Pts',(-3.95510786529101,4.4033839398267,2.07970431745339));
#14292=CARTESIAN_POINT('Ctrl Pts',(-3.83662771957441,4.50698812224134,2.07229999420269));
#14293=CARTESIAN_POINT('Ctrl Pts',(-3.71423151376274,4.60569373978251,2.06489567095199));
#14294=CARTESIAN_POINT('Ctrl Pts',(-3.58549335751221,4.70951378166657,2.0571076932344));
#14295=CARTESIAN_POINT('Ctrl Pts',(-3.45237649393933,4.8079512819552,2.04931971551681));
#14296=CARTESIAN_POINT('Ctrl Pts',(-3.31535291362396,4.90064951007773,2.04153173779923));
#14297=CARTESIAN_POINT('Ctrl Pts',(-3.17835627331423,4.99332951293726,2.03374529126455));
#14298=CARTESIAN_POINT('Ctrl Pts',(-3.0374547133458,5.0802723161561,2.02595884472987));
#14299=CARTESIAN_POINT('Ctrl Pts',(-2.89314982158033,5.16116408113419,2.01817239819518));
#14300=CARTESIAN_POINT('Ctrl Pts',(-2.74883942489208,5.24205893195998,2.01038565462423));
#14301=CARTESIAN_POINT('Ctrl Pts',(-2.60112571341439,5.31690212294558,2.00259891105328));
#14302=CARTESIAN_POINT('Ctrl Pts',(-2.45053617983699,5.38542505228788,1.99481216748233));
#14303=CARTESIAN_POINT('Ctrl Pts',(-2.29995660661947,5.45394344935613,1.98702593894563));
#14304=CARTESIAN_POINT('Ctrl Pts',(-2.14650188287439,5.5161422890811,1.97923971040894));
#14305=CARTESIAN_POINT('Ctrl Pts',(-1.99072097823127,5.57180047644654,1.97145348187224));
#14306=CARTESIAN_POINT('Ctrl Pts',(-1.83489906479755,5.62747331563954,1.9636652036375));
#14307=CARTESIAN_POINT('Ctrl Pts',(-1.67675004730577,5.67660195251726,1.95587692540276));
#14308=CARTESIAN_POINT('Ctrl Pts',(-1.516840474363,5.71901438517462,1.94808864716802));
#14309=CARTESIAN_POINT('Ctrl Pts',(-1.36481428338547,5.75933592733331,1.9406843232585));
#14310=CARTESIAN_POINT('Ctrl Pts',(-1.21119719741052,5.79358745044747,1.93327999934899));
#14311=CARTESIAN_POINT('Ctrl Pts',(-1.05648660776257,5.82166356036815,1.92587567543947));
#14312=CARTESIAN_POINT('Ctrl Pts',(-0.893759717818616,5.85119442867854,
1.91808769787003));
#14313=CARTESIAN_POINT('Ctrl Pts',(-0.729764785624142,5.87390350126465,
1.91029972030059));
#14314=CARTESIAN_POINT('Ctrl Pts',(-0.565086972430272,5.88970349644951,
1.90251174273114));
#14315=CARTESIAN_POINT('Ctrl Pts',(-0.400441536339083,5.90550038521672,
1.89472529634641));
#14316=CARTESIAN_POINT('Ctrl Pts',(-0.235113805031662,5.91439087646084,
1.88693884996168));
#14317=CARTESIAN_POINT('Ctrl Pts',(-0.0696943950806309,5.91633951475018,
1.87915240357695));
#14318=CARTESIAN_POINT('Ctrl Pts',(0.0957313252371021,5.91828822737554,
1.87136566015735));
#14319=CARTESIAN_POINT('Ctrl Pts',(0.261248411726427,5.91329454942756,1.86357891673775));
#14320=CARTESIAN_POINT('Ctrl Pts',(0.426265156846195,5.90137514301191,1.85579217331816));
#14321=CARTESIAN_POINT('Ctrl Pts',(0.591270987344642,5.8894565249757,1.84800594493329));
#14322=CARTESIAN_POINT('Ctrl Pts',(0.755776223961052,5.87061311830516,1.84021971654843));
#14323=CARTESIAN_POINT('Ctrl Pts',(0.919193042425616,5.84491357620079,1.83243348816357));
#14324=CARTESIAN_POINT('Ctrl Pts',(1.0826528798253,5.81920726877726,1.82464521007993));
#14325=CARTESIAN_POINT('Ctrl Pts',(1.24502341035624,5.78664126718395,1.81685693199629));
#14326=CARTESIAN_POINT('Ctrl Pts',(1.40572487473833,5.74733574267607,1.80906865391264));
#14327=CARTESIAN_POINT('Ctrl Pts',(1.55850393618787,5.70996793668136,1.80166432925075));
#14328=CARTESIAN_POINT('Ctrl Pts',(1.70977427758417,5.66650916541479,1.79426000458885));
#14329=CARTESIAN_POINT('Ctrl Pts',(1.85904874226642,5.617104978223,1.78685567992696));
#14330=CARTESIAN_POINT('Ctrl Pts',(2.01605784001132,5.56514092079152,1.77906770133967));
#14331=CARTESIAN_POINT('Ctrl Pts',(2.17091490275741,5.50658037955851,1.77127972275238));
#14332=CARTESIAN_POINT('Ctrl Pts',(2.32306438204911,5.44162681919247,1.76349174416509));
#14333=CARTESIAN_POINT('Ctrl Pts',(2.47518394753153,5.37668602921794,1.75570529675692));
#14334=CARTESIAN_POINT('Ctrl Pts',(2.62459669801067,5.30535485341998,1.74791884934875));
#14335=CARTESIAN_POINT('Ctrl Pts',(2.77076710281248,5.22788487100397,1.74013240194059));
#14336=CARTESIAN_POINT('Ctrl Pts',(2.91694308365394,5.1504119332996,1.7323456574987));
#14337=CARTESIAN_POINT('Ctrl Pts',(3.0598761871294,5.06679986652189,1.72455891305681));
#14338=CARTESIAN_POINT('Ctrl Pts',(3.19905487166316,4.97734653109347,1.71677216861491));
#14339=CARTESIAN_POINT('Ctrl Pts',(3.33822435052314,4.88789911236291,1.70898593921043));
#14340=CARTESIAN_POINT('Ctrl Pts',(3.47363963860669,4.79261137102534,1.70119970980595));
#14341=CARTESIAN_POINT('Ctrl Pts',(3.60481749027507,4.69182495669936,1.69341348040147));
#14342=CARTESIAN_POINT('Ctrl Pts',(3.73602987383304,4.59101201087215,1.68562520131245));
#14343=CARTESIAN_POINT('Ctrl Pts',(3.86300233725031,4.4846976929188,1.67783692222343));
#14344=CARTESIAN_POINT('Ctrl Pts',(3.98528337592958,4.37326502467428,1.67004864313442));
#14345=CARTESIAN_POINT('Ctrl Pts',(4.101536000905,4.26732594915319,1.66264432356109));
#14346=CARTESIAN_POINT('Ctrl Pts',(4.21354843483753,4.15676120981883,1.65524000398776));
#14347=CARTESIAN_POINT('Ctrl Pts',(4.32096262643276,4.04193178362417,1.64783568441444));
#14348=CARTESIAN_POINT('Ctrl Pts',(4.43394250280458,3.92115245099925,1.64004770875137));
#14349=CARTESIAN_POINT('Ctrl Pts',(4.54187538315362,3.79561154167765,1.6322597330883));
#14350=CARTESIAN_POINT('Ctrl Pts',(4.64437089005308,3.66575361939773,1.62447175742523));
#14351=CARTESIAN_POINT('Ctrl Pts',(4.74684624534447,3.53592122844142,1.61668531295351));
#14352=CARTESIAN_POINT('Ctrl Pts',(4.84388616237861,3.40177376874398,1.60889886848179));
#14353=CARTESIAN_POINT('Ctrl Pts',(4.93514087011828,3.26378846658115,1.60111242401007));
#14354=CARTESIAN_POINT('Ctrl Pts',(5.02639905910903,3.12579790045449,1.59332568249539));
#14355=CARTESIAN_POINT('Ctrl Pts',(5.11187141762193,2.98396946324121,1.58553894098072));
#14356=CARTESIAN_POINT('Ctrl Pts',(5.19125139026312,2.83880953316548,1.57775219946604));
#14357=CARTESIAN_POINT('Ctrl Pts',(5.27062611259703,2.69365920417944,1.56996597297782));
#14358=CARTESIAN_POINT('Ctrl Pts',(5.34390910221005,2.54517810372957,1.56217974648959));
#14359=CARTESIAN_POINT('Ctrl Pts',(5.41083960789498,2.3938975124543,1.55439352000136));
#14360=CARTESIAN_POINT('Ctrl Pts',(5.47778773309103,2.24257709643796,1.54660524378256));
#14361=CARTESIAN_POINT('Ctrl Pts',(5.53837990159402,2.08845600860906,1.53881696756376));
#14362=CARTESIAN_POINT('Ctrl Pts',(5.59240303424354,1.93208666086271,1.53102869134495));
#14363=CARTESIAN_POINT('Ctrl Pts',(5.64376296481145,1.78342592148457,1.52362435719727));
#14364=CARTESIAN_POINT('Ctrl Pts',(5.6891858457379,1.63273349867491,1.5162200230496));
#14365=CARTESIAN_POINT('Ctrl Pts',(5.72853009638974,1.48049771943661,1.50881568890192));
#14366=CARTESIAN_POINT('Ctrl Pts',(5.76991292733899,1.3203740060027,1.50102770709394));
#14367=CARTESIAN_POINT('Ctrl Pts',(5.80458529230649,1.15848547592686,1.49323972528595));
#14368=CARTESIAN_POINT('Ctrl Pts',(5.83241723947752,0.995409316384714,1.48545174347797));
#14369=CARTESIAN_POINT('Ctrl Pts',(5.86024371469618,0.83236521873785,1.47766529284081));
#14370=CARTESIAN_POINT('Ctrl Pts',(5.88123240180981,0.66813427231966,1.46987884220365));
#14371=CARTESIAN_POINT('Ctrl Pts',(5.89530463575843,0.503302904924223,1.46209239156649));
#14372=CARTESIAN_POINT('Ctrl Pts',(5.90937740649521,0.338465250003518,1.45430564391363));
#14373=CARTESIAN_POINT('Ctrl Pts',(5.91653316501837,0.173027446319633,1.44651889626076));
#14374=CARTESIAN_POINT('Ctrl Pts',(5.91674514353126,0.00758083104048666,
1.43873214860789));
#14375=CARTESIAN_POINT('Ctrl Pts',(5.91695710802284,-0.157854840787371,
1.43094591600874));
#14376=CARTESIAN_POINT('Ctrl Pts',(5.91022621132736,-0.323299003468176,
1.42315968340959));
#14377=CARTESIAN_POINT('Ctrl Pts',(5.89657782152837,-0.488160380571532,
1.41537345081044));
#14378=CARTESIAN_POINT('Ctrl Pts',(5.88292583896394,-0.653065155340592,
1.40758516858435));
#14379=CARTESIAN_POINT('Ctrl Pts',(5.86235274910231,-0.817386519151318,
1.39979688635826));
#14380=CARTESIAN_POINT('Ctrl Pts',(5.83493589075115,-0.980537461458797,
1.39200860413217));
#14381=CARTESIAN_POINT('Ctrl Pts',(5.80887074100773,-1.13564472019569,1.38460430055124));
#14382=CARTESIAN_POINT('Ctrl Pts',(5.77662043409478,-1.28969392584956,1.37719999697032));
#14383=CARTESIAN_POINT('Ctrl Pts',(5.73829440721614,-1.44218856555304,1.3697956933894));
#14384=CARTESIAN_POINT('Ctrl Pts',(5.69798244315146,-1.60258500986096,1.36200772150222));
#14385=CARTESIAN_POINT('Ctrl Pts',(5.65093397087917,-1.76131888155211,1.35421974961504));
#14386=CARTESIAN_POINT('Ctrl Pts',(5.59731117314015,-1.91782121000381,1.34643177772786));
#14387=CARTESIAN_POINT('Ctrl Pts',(5.54369891818946,-2.07429276850332,1.33864533703529));
#14388=CARTESIAN_POINT('Ctrl Pts',(5.48351502036226,-2.22853335707382,1.33085889634273));
#14389=CARTESIAN_POINT('Ctrl Pts',(5.41697111517321,-2.37999044113188,1.32307245565016));
#14390=CARTESIAN_POINT('Ctrl Pts',(5.35042467115252,-2.53145330369116,1.31528571788363));
#14391=CARTESIAN_POINT('Ctrl Pts',(5.27751785913328,-2.6801321550939,1.3074989801171));
#14392=CARTESIAN_POINT('Ctrl Pts',(5.19851023020338,-2.82549499185024,1.29971224235056));
#14393=CARTESIAN_POINT('Ctrl Pts',(5.11950782670809,-2.97084821454768,1.29192601958606));
#14394=CARTESIAN_POINT('Ctrl Pts',(5.03440556647351,-3.1128855807527,1.28413979682155));
#14395=CARTESIAN_POINT('Ctrl Pts',(4.94350874662523,-3.25110009605054,1.27635357405704));
#14396=CARTESIAN_POINT('Ctrl Pts',(4.85258799721329,-3.38935099780336,1.2685653014858));
#14397=CARTESIAN_POINT('Ctrl Pts',(4.75586981402496,-3.52377676939567,1.26077702891456));
#14398=CARTESIAN_POINT('Ctrl Pts',(4.65370308235257,-3.65389903853434,1.25298875634332));
#14399=CARTESIAN_POINT('Ctrl Pts',(4.55657261843156,-3.77760698299929,1.24558440352118));
#14400=CARTESIAN_POINT('Ctrl Pts',(4.45451799830206,-3.89742527725001,1.23818005069903));
#14401=CARTESIAN_POINT('Ctrl Pts',(4.34787297933363,-4.01297036097708,1.23077569787689));
#14402=CARTESIAN_POINT('Ctrl Pts',(4.23570253591715,-4.13450199369306,1.2229877153972));
#14403=CARTESIAN_POINT('Ctrl Pts',(4.11841326941338,-4.25134933402431,1.21519973291751));
#14404=CARTESIAN_POINT('Ctrl Pts',(3.99641992455798,-4.36309045850485,1.20741175043782));
#14405=CARTESIAN_POINT('Ctrl Pts',(3.8744505647518,-4.47480961361996,1.19962529914939));
#14406=CARTESIAN_POINT('Ctrl Pts',(3.7477792074702,-4.58142434031684,1.19183884786096));
#14407=CARTESIAN_POINT('Ctrl Pts',(3.61685614939428,-4.68255081735253,1.18405239657253));
#14408=CARTESIAN_POINT('Ctrl Pts',(3.4859280978638,-4.78368115138998,1.17626564830593));
#14409=CARTESIAN_POINT('Ctrl Pts',(3.35074827151816,-4.8793226184451,1.16847890003933));
#14410=CARTESIAN_POINT('Ctrl Pts',(3.21179920916008,-4.96913235912857,1.16069215177272));
#14411=CARTESIAN_POINT('Ctrl Pts',(3.0728593379622,-5.05893615910471,1.15290591858157));
#14412=CARTESIAN_POINT('Ctrl Pts',(2.93015099814565,-5.14290883128224,1.14511968539041));
#14413=CARTESIAN_POINT('Ctrl Pts',(2.78418492235192,-5.22075137127293,1.13733345219926));
#14414=CARTESIAN_POINT('Ctrl Pts',(2.63818042362199,-5.29861440190799,1.12954516942268));
#14415=CARTESIAN_POINT('Ctrl Pts',(2.48891675659648,-5.37034392375692,1.12175688664611));
#14416=CARTESIAN_POINT('Ctrl Pts',(2.3369292236997,-5.43568692677552,1.11396860386953));
#14417=CARTESIAN_POINT('Ctrl Pts',(2.19243506518412,-5.49780835250106,1.10656430336781));
#14418=CARTESIAN_POINT('Ctrl Pts',(2.04547939960954,-5.55415772801522,1.09916000286609));
#14419=CARTESIAN_POINT('Ctrl Pts',(1.89653885159617,-5.60455805098728,1.09175570236437));
#14420=CARTESIAN_POINT('Ctrl Pts',(1.73988035291167,-5.65757006843538,1.08396771839439));
#14421=CARTESIAN_POINT('Ctrl Pts',(1.58096976410852,-5.70401907735309,1.0761797344244));
#14422=CARTESIAN_POINT('Ctrl Pts',(1.42037319087769,-5.74373315546047,1.06839175045442));
#14423=CARTESIAN_POINT('Ctrl Pts',(1.25980819081974,-5.78343942580814,1.06060529759659));
#14424=CARTESIAN_POINT('Ctrl Pts',(1.09755817771552,-5.81641333061659,1.05281884473876));
#14425=CARTESIAN_POINT('Ctrl Pts',(0.934202233413419,-5.84253341878208,
1.04503239188092));
#14426=CARTESIAN_POINT('Ctrl Pts',(0.770840056423254,-5.86865450353426,
1.03724564193851));
#14427=CARTESIAN_POINT('Ctrl Pts',(0.606372178706276,-5.88792119401931,
1.0294588919961));
#14428=CARTESIAN_POINT('Ctrl Pts',(0.441386383453259,-5.90026343674603,
1.02167214205369));
#14429=CARTESIAN_POINT('Ctrl Pts',(0.276411500469021,-5.91260486314871,
1.01388590713203));
#14430=CARTESIAN_POINT('Ctrl Pts',(0.110919087192631,-5.91802273456761,
1.00609967221037));
#14431=CARTESIAN_POINT('Ctrl Pts',(-0.0544993110831236,-5.91649899751462,
0.998313437288713));
#14432=CARTESIAN_POINT('Ctrl Pts',(-0.219961254320349,-5.91497485935104,
0.990525152708109));
#14433=CARTESIAN_POINT('Ctrl Pts',(-0.385348823857749,-5.90650546233805,
0.982736868127505));
#14434=CARTESIAN_POINT('Ctrl Pts',(-0.550070918233379,-5.89112489660624,
0.974948583546901));
#14435=CARTESIAN_POINT('Ctrl Pts',(-0.706671580567881,-5.87650265185025,
0.967544291315217));
#14436=CARTESIAN_POINT('Ctrl Pts',(-0.862670545487099,-5.85563433930647,
0.960139999083533));
#14437=CARTESIAN_POINT('Ctrl Pts',(-1.01756461492942,-5.82859269609256,
0.952735706851849));
#14438=CARTESIAN_POINT('Ctrl Pts',(-1.18048437152111,-5.80014991615843,
0.944947768343532));
#14439=CARTESIAN_POINT('Ctrl Pts',(-1.34223998014971,-5.76486691519121,
0.937159829835215));
#14440=CARTESIAN_POINT('Ctrl Pts',(-1.50225211465874,-5.72286371902244,
0.929371891326898));
#14441=CARTESIAN_POINT('Ctrl Pts',(-1.66223278487941,-5.6808687822315,0.921585484214583));
#14442=CARTESIAN_POINT('Ctrl Pts',(-1.82047035613447,-5.63215636798189,
0.913799077102268));
#14443=CARTESIAN_POINT('Ctrl Pts',(-1.97639826796814,-5.5768970269203,0.906012669989952));
#14444=CARTESIAN_POINT('Ctrl Pts',(-2.13233212911768,-5.52163557747882,
0.898225965792947));
#14445=CARTESIAN_POINT('Ctrl Pts',(-2.28595585199728,-5.45982680439626,
0.890439261595941));
#14446=CARTESIAN_POINT('Ctrl Pts',(-2.43671983863289,-5.39169055032954,
0.882652557398935));
#14447=CARTESIAN_POINT('Ctrl Pts',(-2.5874738553676,-5.32355880205838,0.874866368130401));
#14448=CARTESIAN_POINT('Ctrl Pts',(-2.73536822312365,-5.24910054186575,
0.867080178861867));
#14449=CARTESIAN_POINT('Ctrl Pts',(-2.87987493147773,-5.16858306903799,
0.859293989593333));
#14450=CARTESIAN_POINT('Ctrl Pts',(-3.02441969116596,-5.08804439444529,
0.851505750074724));
#14451=CARTESIAN_POINT('Ctrl Pts',(-3.16557472869233,-5.00144347299672,
0.843717510556114));
#14452=CARTESIAN_POINT('Ctrl Pts',(-3.30283738272883,-4.90909317346381,
0.835929271037505));
#14453=CARTESIAN_POINT('Ctrl Pts',(-3.43333722814679,-4.82129289087463,
0.828524751138114));
#14454=CARTESIAN_POINT('Ctrl Pts',(-3.56031878657049,-4.72829627227522,
0.821120231238722));
#14455=CARTESIAN_POINT('Ctrl Pts',(-3.68337502978592,-4.63040807623362,
0.813715711339331));
#14456=CARTESIAN_POINT('Ctrl Pts',(-3.812805829406,-4.52744907833173,0.805927622687028));
#14457=CARTESIAN_POINT('Ctrl Pts',(-3.93794013521075,-4.41904143915328,
0.798139534034725));
#14458=CARTESIAN_POINT('Ctrl Pts',(-4.05832674032956,-4.30556786396708,
0.790351445382422));
#14459=CARTESIAN_POINT('Ctrl Pts',(-4.17868968384183,-4.19211659165325,
0.782564887454315));
#14460=CARTESIAN_POINT('Ctrl Pts',(-4.29430655619166,-4.0736015890688,0.774778329526209));
#14461=CARTESIAN_POINT('Ctrl Pts',(-4.40476154371107,-3.95044381121211,
0.766991771598102));
#14462=CARTESIAN_POINT('Ctrl Pts',(-4.51522073971969,-3.82728134087217,
0.759204916991269));
#14463=CARTESIAN_POINT('Ctrl Pts',(-4.62051744106989,-3.69947597651694,
0.751418062384436));
#14464=CARTESIAN_POINT('Ctrl Pts',(-4.72027432182029,-3.56748383167521,
0.743631207777603));
#14465=CARTESIAN_POINT('Ctrl Pts',(-4.82002459913294,-3.43550042409455,
0.735844868624032));
#14466=CARTESIAN_POINT('Ctrl Pts',(-4.91423559709953,-3.29933104564105,
0.728058529470462));
#14467=CARTESIAN_POINT('Ctrl Pts',(-5.00257165952262,-3.15946314329525,
0.720272190316891));
#14468=CARTESIAN_POINT('Ctrl Pts',(-5.09093095587724,-3.0195584532415,0.712483803219754));
#14469=CARTESIAN_POINT('Ctrl Pts',(-5.17341205663834,-2.87595356478015,
0.704695416122617));
#14470=CARTESIAN_POINT('Ctrl Pts',(-5.24972337465897,-2.72916380088467,
0.69690702902548));
#14471=CARTESIAN_POINT('Ctrl Pts',(-5.32226619017904,-2.58962299568426,
0.689503257959258));
#14472=CARTESIAN_POINT('Ctrl Pts',(-5.3892337649721,-2.44720451728423,0.682099486893036));
#14473=CARTESIAN_POINT('Ctrl Pts',(-5.45041467059078,-2.30237062201307,
0.674695715826813));
#14474=CARTESIAN_POINT('Ctrl Pts',(-5.51451855214798,-2.15061714968302,
0.66693822255818));
#14475=CARTESIAN_POINT('Ctrl Pts',(-5.57229381698287,-1.99615353593203,
0.659180729289547));
#14476=CARTESIAN_POINT('Ctrl Pts',(-5.62352825526249,-1.83952725578189,
0.651423236020914));
#14477=CARTESIAN_POINT('Ctrl Pts',(-5.67475659161283,-1.68291962953947,
0.64366666665575));
#14478=CARTESIAN_POINT('Ctrl Pts',(-5.71944555125269,-1.52415015800134,
0.635910097290585));
#14479=CARTESIAN_POINT('Ctrl Pts',(-5.75743223964334,-1.36378318233344,
0.628153527925421));
#14480=CARTESIAN_POINT('Ctrl Pts',(-5.79541379850369,-1.20343786181091,
0.620398005968157));
#14481=CARTESIAN_POINT('Ctrl Pts',(-5.82669481876659,-1.04149578374859,
0.612642484010893));
#14482=CARTESIAN_POINT('Ctrl Pts',(-5.85116309175147,-0.878533457658481,
0.604886962053629));
#14483=CARTESIAN_POINT('Ctrl Pts',(-5.87563494937356,-0.715547257353048,
0.597130303901236));
#14484=CARTESIAN_POINT('Ctrl Pts',(-5.89329201504539,-0.551540831112721,
0.589373645748843));
#14485=CARTESIAN_POINT('Ctrl Pts',(-5.90407361576536,-0.38709856900187,
0.58161698759645));
#14486=CARTESIAN_POINT('Ctrl Pts',(-5.9125255268044,-0.258189012200728,
0.57553638914294));
#14487=CARTESIAN_POINT('Ctrl Pts',(-5.91675327563298,-0.129011823564914,
0.56945579068943));
#14488=CARTESIAN_POINT('Ctrl Pts',(-5.91674999809507,0.000150139963021254,
0.56337519223592));
#14489=CARTESIAN_POINT('Ctrl Pts',(-5.91671935081961,9.79311290895061E-5,
0.311624807795122));
#14490=CARTESIAN_POINT('Ctrl Pts',(-5.9159606431657,-0.744933876419475,
0.34669625714854));
#14491=CARTESIAN_POINT('Ctrl Pts',(-5.58832513159245,-2.47438543481707,
0.428083168263666));
#14492=CARTESIAN_POINT('Ctrl Pts',(-3.94583161690989,-4.74057417199595,
0.5557855411405));
#14493=CARTESIAN_POINT('Ctrl Pts',(-1.19688167165833,-6.05056333833174,
0.694731926425626));
#14494=CARTESIAN_POINT('Ctrl Pts',(1.84380127964053,-5.8858030207415,0.833678311710752));
#14495=CARTESIAN_POINT('Ctrl Pts',(4.43505585547799,-4.28630058757937,0.972624696995877));
#14496=CARTESIAN_POINT('Ctrl Pts',(5.94524311070241,-1.64202041018131,1.111571082281));
#14497=CARTESIAN_POINT('Ctrl Pts',(6.00625314087822,1.40252303398188,1.25051746756613));
#14498=CARTESIAN_POINT('Ctrl Pts',(4.6032120253118,4.10518839802672,1.38946385285126));
#14499=CARTESIAN_POINT('Ctrl Pts',(2.07811839533017,5.80719982717728,1.52841023813638));
#14500=CARTESIAN_POINT('Ctrl Pts',(-0.953525845772481,6.09367921958054,
1.66735662342151));
#14501=CARTESIAN_POINT('Ctrl Pts',(-3.75274390497941,4.89479875289577,1.80630300870662));
#14502=CARTESIAN_POINT('Ctrl Pts',(-5.53517423299281,2.63231165564186,1.93772573683117));
#14503=CARTESIAN_POINT('Ctrl Pts',(-5.91614959567988,0.823835166170361,
2.022833003194));
#14504=CARTESIAN_POINT('Ctrl Pts',(-5.91696061209103,-0.000135486519901937,
2.06162480779511));
#14505=CARTESIAN_POINT('Origin',(0.,0.,0.));
#14506=CARTESIAN_POINT('',(-5.9167499990742,0.000104668362501446,4.0633751922049));
#14507=CARTESIAN_POINT('',(-5.91671854102846,6.05288050462508E-5,3.81162480733001));
#14508=CARTESIAN_POINT('',(-5.91675,-7.2459289488551E-16,0.));
#14509=CARTESIAN_POINT('Ctrl Pts',(-5.91636571888598,0.000104875761786346,
4.0633751821236));
#14510=CARTESIAN_POINT('Ctrl Pts',(-5.91659904124727,0.369799356614414,
4.04597532412481));
#14511=CARTESIAN_POINT('Ctrl Pts',(-5.79166172450625,1.72392321031336,3.98223546762185));
#14512=CARTESIAN_POINT('Ctrl Pts',(-4.77062984080853,3.9098068260098,3.87215561261471));
#14513=CARTESIAN_POINT('Ctrl Pts',(-2.31709881191985,5.71634075178491,3.73313561710221));
#14514=CARTESIAN_POINT('Ctrl Pts',(0.701821240062036,6.12804580937004,3.59411562158967));
#14515=CARTESIAN_POINT('Ctrl Pts',(3.54949178673034,5.04446295958584,3.45509562607715));
#14516=CARTESIAN_POINT('Ctrl Pts',(5.5310604289586,2.7299943270923,3.31607563056466));
#14517=CARTESIAN_POINT('Ctrl Pts',(6.16300995416518,-0.250612848028229,
3.17705563505213));
#14518=CARTESIAN_POINT('Ctrl Pts',(5.29114006546501,-3.17006865891296,3.03803563953961));
#14519=CARTESIAN_POINT('Ctrl Pts',(3.12819337966652,-5.31600457811581,2.89901564402709));
#14520=CARTESIAN_POINT('Ctrl Pts',(0.201944675889461,-6.16479657747871,
2.75999564851458));
#14521=CARTESIAN_POINT('Ctrl Pts',(-2.7735800028256,-5.50933321411907,2.62097565300206));
#14522=CARTESIAN_POINT('Ctrl Pts',(-5.07233091594555,-3.50955233214131,
2.48195565748954));
#14523=CARTESIAN_POINT('Ctrl Pts',(-5.85491408923019,-1.40302289339775,
2.37942217055716));
#14524=CARTESIAN_POINT('Ctrl Pts',(-5.91702306393301,-0.209464058491032,
2.32322868212894));
#14525=CARTESIAN_POINT('Ctrl Pts',(-5.91680640865236,-0.000151898509373194,
2.3133751922049));
#14526=CARTESIAN_POINT('Ctrl Pts',(-5.91696061209103,-0.000135486519901937,
2.06162480779511));
#14527=CARTESIAN_POINT('Ctrl Pts',(-5.91711790844504,-0.159944311218166,
2.0691484649557));
#14528=CARTESIAN_POINT('Ctrl Pts',(-5.8717187617454,-1.30344349398301,2.12298758387799));
#14529=CARTESIAN_POINT('Ctrl Pts',(-5.15946265009878,-3.37965766280873,
2.22314216456201));
#14530=CARTESIAN_POINT('Ctrl Pts',(-2.91369452509655,-5.43622339098344,
2.36208854984714));
#14531=CARTESIAN_POINT('Ctrl Pts',(0.0422993022801887,-6.16768606948156,
2.50103493513227));
#14532=CARTESIAN_POINT('Ctrl Pts',(2.987982492874,-5.39574844063278,2.63998132041738));
#14533=CARTESIAN_POINT('Ctrl Pts',(5.20533196103198,-3.30857368275367,2.77892770570252));
#14534=CARTESIAN_POINT('Ctrl Pts',(6.15385913663824,-0.414919702877659,
2.91787409098763));
#14535=CARTESIAN_POINT('Ctrl Pts',(5.60235639658781,2.57987275594974,3.05682047627278));
#14536=CARTESIAN_POINT('Ctrl Pts',(3.68525493156209,4.94581001697408,3.19576686155787));
#14537=CARTESIAN_POINT('Ctrl Pts',(0.869856557091352,6.10618458632405,3.33471324684302));
#14538=CARTESIAN_POINT('Ctrl Pts',(-2.15757313440082,5.77815011947596,3.47365963212813));
#14539=CARTESIAN_POINT('Ctrl Pts',(-4.65908499542979,4.04166644322682,3.61260601741327));
#14540=CARTESIAN_POINT('Ctrl Pts',(-5.76648150081493,1.83499894741018,3.72526107365585));
#14541=CARTESIAN_POINT('Ctrl Pts',(-5.9164332113239,0.425530598565133,3.7916006681367));
#14542=CARTESIAN_POINT('Ctrl Pts',(-5.91628064325804,6.06618882952148E-5,
3.81162480085584));
#14543=CARTESIAN_POINT('Origin',(0.,0.,0.));
#14544=CARTESIAN_POINT('',(-5.91674999987984,-3.77088797724088E-5,5.81337519217928));
#14545=CARTESIAN_POINT('',(-5.91674999993288,2.81822667955784E-5,5.56162480783485));
#14546=CARTESIAN_POINT('',(-5.91675,-7.2459289488551E-16,0.));
#14547=CARTESIAN_POINT('Ctrl Pts',(-5.91674999987984,-3.7708879784822E-5,
5.81337519217929));
#14548=CARTESIAN_POINT('Ctrl Pts',(-5.91675105226619,0.165088037798311,
5.8055995119159));
#14549=CARTESIAN_POINT('Ctrl Pts',(-5.90983522173606,0.330244822975408,
5.79782383165252));
#14550=CARTESIAN_POINT('Ctrl Pts',(-5.8960207664832,0.494843089977935,5.79004815138914));
#14551=CARTESIAN_POINT('Ctrl Pts',(-5.88220905787429,0.659408630909986,
5.78227401711688));
#14552=CARTESIAN_POINT('Ctrl Pts',(-5.8615014880818,0.823415554973462,5.77449988284463));
#14553=CARTESIAN_POINT('Ctrl Pts',(-5.83396828371955,0.986278169207031,
5.76672574857237));
#14554=CARTESIAN_POINT('Ctrl Pts',(-5.80643420898685,1.14914593179905,5.75895136854678));
#14555=CARTESIAN_POINT('Ctrl Pts',(-5.77207411781776,1.3108689944891,5.7511769885212));
#14556=CARTESIAN_POINT('Ctrl Pts',(-5.73100970695798,1.47086991309681,5.74340260849561));
#14557=CARTESIAN_POINT('Ctrl Pts',(-5.68994750990974,1.63086220594139,5.73562864759237));
#14558=CARTESIAN_POINT('Ctrl Pts',(-5.64218179703028,1.78913222916042,5.72785468668913));
#14559=CARTESIAN_POINT('Ctrl Pts',(-5.5878847206219,1.94511565505508,5.72008072578589));
#14560=CARTESIAN_POINT('Ctrl Pts',(-5.53357411629539,2.10113794365016,5.71230482802871));
#14561=CARTESIAN_POINT('Ctrl Pts',(-5.47272900192084,2.25487219245781,5.70452893027153));
#14562=CARTESIAN_POINT('Ctrl Pts',(-5.40557074228287,2.40577129267839,5.69675303251435));
#14563=CARTESIAN_POINT('Ctrl Pts',(-5.35565775468702,2.51792168129976,5.69097387310204));
#14564=CARTESIAN_POINT('Ctrl Pts',(-5.30225861598434,2.62850636722495,5.68519471368974));
#14565=CARTESIAN_POINT('Ctrl Pts',(-5.24548115676519,2.73730853148149,5.67941555427743));
#14566=CARTESIAN_POINT('Ctrl Pts',(-5.16896802428216,2.88392999927327,5.67162757651591));
#14567=CARTESIAN_POINT('Ctrl Pts',(-5.08628982356809,3.02736763814977,5.6638395987544));
#14568=CARTESIAN_POINT('Ctrl Pts',(-4.99773662714317,3.16710580312872,5.65605162099288));
#14569=CARTESIAN_POINT('Ctrl Pts',(-4.90920084103584,3.30681649438646,5.64826517441456));
#14570=CARTESIAN_POINT('Ctrl Pts',(-4.81479253487457,3.44282889327005,5.64047872783624));
#14571=CARTESIAN_POINT('Ctrl Pts',(-4.71484605482713,3.57465484232828,5.63269228125791));
#14572=CARTESIAN_POINT('Ctrl Pts',(-4.61489576204672,3.70648582024938,5.6249055376442));
#14573=CARTESIAN_POINT('Ctrl Pts',(-4.5094070625286,3.83412977175722,5.61711879403049));
#14574=CARTESIAN_POINT('Ctrl Pts',(-4.39875612857577,3.9571296521364,5.60933205041678));
#14575=CARTESIAN_POINT('Ctrl Pts',(-4.28811251335451,4.08012139699356,5.60154582183791));
#14576=CARTESIAN_POINT('Ctrl Pts',(-4.17230756079509,4.19846944790559,5.59375959325904));
#14577=CARTESIAN_POINT('Ctrl Pts',(-4.05175611777413,4.31175172343908,5.58597336468017));
#14578=CARTESIAN_POINT('Ctrl Pts',(-3.93117294001901,4.42506382012453,5.57818508640461));
#14579=CARTESIAN_POINT('Ctrl Pts',(-3.80584100672858,4.53330725632599,5.57039680812905));
#14580=CARTESIAN_POINT('Ctrl Pts',(-3.67621090030028,4.63609792595167,5.56260852985349));
#14581=CARTESIAN_POINT('Ctrl Pts',(-3.55297143262765,4.73382111507355,5.5552042061573));
#14582=CARTESIAN_POINT('Ctrl Pts',(-3.42584758127257,4.82661605532041,5.54779988246111));
#14583=CARTESIAN_POINT('Ctrl Pts',(-3.29525315733809,4.91418733785693,5.54039555876493));
#14584=CARTESIAN_POINT('Ctrl Pts',(-3.1578920003824,5.00629611496172,5.53260758100339));
#14585=CARTESIAN_POINT('Ctrl Pts',(-3.01664193089225,5.09265848517566,5.52481960324185));
#14586=CARTESIAN_POINT('Ctrl Pts',(-2.8720044538864,5.17296056232374,5.51703162548031));
#14587=CARTESIAN_POINT('Ctrl Pts',(-2.72739541384842,5.25324685139507,5.50924517890196));
#14588=CARTESIAN_POINT('Ctrl Pts',(-2.57940057435582,5.32747506978982,5.50145873232361));
#14589=CARTESIAN_POINT('Ctrl Pts',(-2.42854715514535,5.39537665763341,5.49367228574526));
#14590=CARTESIAN_POINT('Ctrl Pts',(-2.27768798121713,5.46328083576944,5.48588554213153));
#14591=CARTESIAN_POINT('Ctrl Pts',(-2.12397029912205,5.52485776565383,5.4780987985178));
#14592=CARTESIAN_POINT('Ctrl Pts',(-1.96794315914089,5.57988622508475,5.47031205490407));
#14593=CARTESIAN_POINT('Ctrl Pts',(-1.81192633918796,5.6349110447947,5.46252582632519));
#14594=CARTESIAN_POINT('Ctrl Pts',(-1.653600668451,5.68338815462775,5.45473959774631));
#14595=CARTESIAN_POINT('Ctrl Pts',(-1.49353241756466,5.72514554227082,5.44695336916743));
#14596=CARTESIAN_POINT('Ctrl Pts',(-1.33342202928609,5.76691392239624,5.43916509089183));
#14597=CARTESIAN_POINT('Ctrl Pts',(-1.17156845313732,5.80195896300279,5.43137681261624));
#14598=CARTESIAN_POINT('Ctrl Pts',(-1.00855115785462,5.83015909941488,5.42358853434064));
#14599=CARTESIAN_POINT('Ctrl Pts',(-0.853570457419871,5.8569689964011,5.41618421064456));
#14600=CARTESIAN_POINT('Ctrl Pts',(-0.697538273997836,5.87759258131212,
5.40877988694848));
#14601=CARTESIAN_POINT('Ctrl Pts',(-0.540959334783866,5.89196856412271,
5.4013755632524));
#14602=CARTESIAN_POINT('Ctrl Pts',(-0.37626727828091,5.90708943660538,5.39358758549088));
#14603=CARTESIAN_POINT('Ctrl Pts',(-0.210911387984493,5.91530348944729,
5.38579960772936));
#14604=CARTESIAN_POINT('Ctrl Pts',(-0.0454822305267683,5.91657518579848,
5.37801162996784));
#14605=CARTESIAN_POINT('Ctrl Pts',(0.119914402140894,5.91784663212327,5.37022518338949));
#14606=CARTESIAN_POINT('Ctrl Pts',(0.285383953883248,5.91217844293329,5.36243873681113));
#14607=CARTESIAN_POINT('Ctrl Pts',(0.450334976858607,5.89958718650024,5.35465229023278));
#14608=CARTESIAN_POINT('Ctrl Pts',(0.615292292343057,5.88699544973917,5.34686554661908));
#14609=CARTESIAN_POINT('Ctrl Pts',(0.779730720565956,5.86748013764543,5.33907880300537));
#14610=CARTESIAN_POINT('Ctrl Pts',(0.943062305544855,5.84110983036276,5.33129205939166));
#14611=CARTESIAN_POINT('Ctrl Pts',(1.10638308736111,5.81474126727867,5.3235058308128));
#14612=CARTESIAN_POINT('Ctrl Pts',(1.26859685696312,5.78151866738902,5.31571960223394));
#14613=CARTESIAN_POINT('Ctrl Pts',(1.42912409412647,5.74156205976102,5.30793337365508));
#14614=CARTESIAN_POINT('Ctrl Pts',(1.5896935895086,5.70159493369953,5.3001450953795));
#14615=CARTESIAN_POINT('Ctrl Pts',(1.74857535453158,5.65489033300201,5.29235681710392));
#14616=CARTESIAN_POINT('Ctrl Pts',(1.90520242872164,5.60161889707727,5.28456853882834));
#14617=CARTESIAN_POINT('Ctrl Pts',(2.05410793977932,5.5509736913734,5.27716421513219));
#14618=CARTESIAN_POINT('Ctrl Pts',(2.20097546360534,5.49439361569545,5.26975989143604));
#14619=CARTESIAN_POINT('Ctrl Pts',(2.34533251403175,5.43206645404173,5.26235556773989));
#14620=CARTESIAN_POINT('Ctrl Pts',(2.49716940617415,5.36650981864635,5.25456758997836));
#14621=CARTESIAN_POINT('Ctrl Pts',(2.64628307307795,5.2945712652669,5.24677961221684));
#14622=CARTESIAN_POINT('Ctrl Pts',(2.79213798906654,5.21650227762928,5.23899163445532));
#14623=CARTESIAN_POINT('Ctrl Pts',(2.93796422872813,5.13844863902397,5.23120518787699));
#14624=CARTESIAN_POINT('Ctrl Pts',(3.08053271429802,5.05426712178518,5.22341874129867));
#14625=CARTESIAN_POINT('Ctrl Pts',(3.21933208742007,4.96425537955165,5.21563229472034));
#14626=CARTESIAN_POINT('Ctrl Pts',(3.35813675542532,4.87424020357306,5.20784555110663));
#14627=CARTESIAN_POINT('Ctrl Pts',(3.49317175301991,4.7783945280985,5.20005880749292));
#14628=CARTESIAN_POINT('Ctrl Pts',(3.62395368407104,4.67706000156166,5.19227206387922));
#14629=CARTESIAN_POINT('Ctrl Pts',(3.75472696487569,4.57573217754575,5.18448583530035));
#14630=CARTESIAN_POINT('Ctrl Pts',(3.88124748952844,4.4689164248052,5.17669960672149));
#14631=CARTESIAN_POINT('Ctrl Pts',(4.00306389537987,4.35699552581893,5.16891337814262));
#14632=CARTESIAN_POINT('Ctrl Pts',(4.12491236896257,4.24504516405803,5.16112509986705));
#14633=CARTESIAN_POINT('Ctrl Pts',(4.24205401248351,4.12798718553333,5.15333682159148));
#14634=CARTESIAN_POINT('Ctrl Pts',(4.35407271622536,4.00624279647675,5.14554854331591));
#14635=CARTESIAN_POINT('Ctrl Pts',(4.4605690063147,3.89050028794358,5.13814421961973));
#14636=CARTESIAN_POINT('Ctrl Pts',(4.56243512271358,3.77052250313101,5.13073989592355));
#14637=CARTESIAN_POINT('Ctrl Pts',(4.65934611035522,3.64670047939473,5.12333557222737));
#14638=CARTESIAN_POINT('Ctrl Pts',(4.76127852816528,3.51646263366925,5.11554759446585));
#14639=CARTESIAN_POINT('Ctrl Pts',(4.85776514854029,3.38192500618747,5.10775961670433));
#14640=CARTESIAN_POINT('Ctrl Pts',(4.94845615893317,3.24356473738639,5.0999716389428));
#14641=CARTESIAN_POINT('Ctrl Pts',(5.03912933869608,3.10523167140004,5.09218519236446));
#14642=CARTESIAN_POINT('Ctrl Pts',(5.12400900697827,2.96307773077667,5.08439874578612));
#14643=CARTESIAN_POINT('Ctrl Pts',(5.20278867008055,2.81760902486159,5.07661229920778));
#14644=CARTESIAN_POINT('Ctrl Pts',(5.2815713384494,2.67213476964327,5.06882555559405));
#14645=CARTESIAN_POINT('Ctrl Pts',(5.35425338035422,2.52334577520074,5.06103881198032));
#14646=CARTESIAN_POINT('Ctrl Pts',(5.42057391169674,2.37177339354601,5.05325206836659));
#14647=CARTESIAN_POINT('Ctrl Pts',(5.48689005643205,2.22021103727085,5.04546583978773));
#14648=CARTESIAN_POINT('Ctrl Pts',(5.54684540462062,2.06586595501828,5.03767961120886));
#14649=CARTESIAN_POINT('Ctrl Pts',(5.60022688696906,1.90929028096014,5.02989338262999));
#14650=CARTESIAN_POINT('Ctrl Pts',(5.65362242180102,1.75267338891812,5.02210510435441));
#14651=CARTESIAN_POINT('Ctrl Pts',(5.70044052775977,1.59382503375644,5.01431682607883));
#14652=CARTESIAN_POINT('Ctrl Pts',(5.74051747969277,1.43331421113507,5.00652854780326));
#14653=CARTESIAN_POINT('Ctrl Pts',(5.77861867669246,1.28071641668446,4.99912422410712));
#14654=CARTESIAN_POINT('Ctrl Pts',(5.81062730972007,1.12661637797558,4.991719900411));
#14655=CARTESIAN_POINT('Ctrl Pts',(5.8364452462182,0.971512969752345,4.98431557671486));
#14656=CARTESIAN_POINT('Ctrl Pts',(5.86360093572451,0.808372898686376,4.97652759895332));
#14657=CARTESIAN_POINT('Ctrl Pts',(5.88391706992344,0.644064360225406,4.96873962119177));
#14658=CARTESIAN_POINT('Ctrl Pts',(5.89731490621227,0.479173725768137,4.96095164343023));
#14659=CARTESIAN_POINT('Ctrl Pts',(5.91071010837164,0.314315510223223,4.95316519685188));
#14660=CARTESIAN_POINT('Ctrl Pts',(5.91718970075061,0.148875745338547,4.94537875027353));
#14661=CARTESIAN_POINT('Ctrl Pts',(5.9167268410067,-0.0165544982084554,
4.93759230369518));
#14662=CARTESIAN_POINT('Ctrl Pts',(5.91626396360573,-0.181991052546074,
4.92980556008146));
#14663=CARTESIAN_POINT('Ctrl Pts',(5.90885810107439,-0.347417765270474,
4.92201881646774));
#14664=CARTESIAN_POINT('Ctrl Pts',(5.8945345389731,-0.512243234560655,4.91423207285402));
#14665=CARTESIAN_POINT('Ctrl Pts',(5.88021192426822,-0.677057801879899,
4.90644584427509));
#14666=CARTESIAN_POINT('Ctrl Pts',(5.85897255340783,-0.841270886979092,
4.89865961569617));
#14667=CARTESIAN_POINT('Ctrl Pts',(5.83089364091742,-1.00429572876161,4.89087338711725));
#14668=CARTESIAN_POINT('Ctrl Pts',(5.80280733675431,-1.1673634862472,4.88308510884167));
#14669=CARTESIAN_POINT('Ctrl Pts',(5.76787794556166,-1.3292420599192,4.87529683056608));
#14670=CARTESIAN_POINT('Ctrl Pts',(5.72623407688394,-1.48935350378381,4.8675085522905));
#14671=CARTESIAN_POINT('Ctrl Pts',(5.68664321061859,-1.64157160846214,4.86010422859445));
#14672=CARTESIAN_POINT('Ctrl Pts',(5.64098402017967,-1.79219236681351,4.85269990489839));
#14673=CARTESIAN_POINT('Ctrl Pts',(5.58940914057945,-1.94073079578464,4.84529558120233));
#14674=CARTESIAN_POINT('Ctrl Pts',(5.53516191532728,-2.0969657240571,4.8375076034408));
#14675=CARTESIAN_POINT('Ctrl Pts',(5.47435027831378,-2.25095269078999,4.82971962567928));
#14676=CARTESIAN_POINT('Ctrl Pts',(5.40718577065045,-2.40213917252422,4.82193164791775));
#14677=CARTESIAN_POINT('Ctrl Pts',(5.34003446810493,-2.55329592970046,4.81414520133939));
#14678=CARTESIAN_POINT('Ctrl Pts',(5.26653291674423,-2.70165300863541,4.80635875476103));
#14679=CARTESIAN_POINT('Ctrl Pts',(5.18694047531005,-2.84667860287921,4.79857230818268));
#14680=CARTESIAN_POINT('Ctrl Pts',(5.10734499760404,-2.99170972952181,4.79078556456897));
#14681=CARTESIAN_POINT('Ctrl Pts',(5.02165831515141,-3.13340883513923,4.78299882095527));
#14682=CARTESIAN_POINT('Ctrl Pts',(4.93018571331,-3.27126877446259,4.77521207734156));
#14683=CARTESIAN_POINT('Ctrl Pts',(4.8387191616968,-3.40911959538244,4.76742584876269));
#14684=CARTESIAN_POINT('Ctrl Pts',(4.74146763330826,-3.54313149193686,4.75963962018381));
#14685=CARTESIAN_POINT('Ctrl Pts',(4.63877978558092,-3.67282625009486,4.75185339160494));
#14686=CARTESIAN_POINT('Ctrl Pts',(4.53606490564644,-3.80255514993217,4.74406511332935));
#14687=CARTESIAN_POINT('Ctrl Pts',(4.42791104371039,-3.92796438855324,4.73627683505376));
#14688=CARTESIAN_POINT('Ctrl Pts',(4.31470776234669,-4.04860809267151,4.72848855677818));
#14689=CARTESIAN_POINT('Ctrl Pts',(4.20708529316667,-4.16330417896707,4.72108423308206));
#14690=CARTESIAN_POINT('Ctrl Pts',(4.0948994550037,-4.27369309251353,4.71367990938594));
#14691=CARTESIAN_POINT('Ctrl Pts',(3.97851640638261,-4.37942208135325,4.70627558568982));
#14692=CARTESIAN_POINT('Ctrl Pts',(3.85610298529545,-4.49062940394276,4.6984876079283));
#14693=CARTESIAN_POINT('Ctrl Pts',(3.72900206037776,-4.59672085508215,4.69069963016678));
#14694=CARTESIAN_POINT('Ctrl Pts',(3.59766383887997,-4.69731257900892,4.68291165240526));
#14695=CARTESIAN_POINT('Ctrl Pts',(3.46635143960298,-4.79788452574001,4.67512520582697));
#14696=CARTESIAN_POINT('Ctrl Pts',(3.33080365953879,-4.89295870857519,4.66733875924867));
#14697=CARTESIAN_POINT('Ctrl Pts',(3.1915027730872,-4.98219234994763,4.65955231267038));
#14698=CARTESIAN_POINT('Ctrl Pts',(3.05219657262047,-5.07142939538256,4.65176556905668));
#14699=CARTESIAN_POINT('Ctrl Pts',(2.90913724621,-5.15482527783159,4.64397882544298));
#14700=CARTESIAN_POINT('Ctrl Pts',(2.76283558715538,-5.23208085572536,4.63619208182928));
#14701=CARTESIAN_POINT('Ctrl Pts',(2.61654360486111,-5.30933132374055,4.62840585325042));
#14702=CARTESIAN_POINT('Ctrl Pts',(2.46701000173054,-5.3804421508112,4.62061962467157));
#14703=CARTESIAN_POINT('Ctrl Pts',(2.31476980315181,-5.44516035768613,4.61283339609271));
#14704=CARTESIAN_POINT('Ctrl Pts',(2.1624895278877,-5.50989560139653,4.60504511781715));
#14705=CARTESIAN_POINT('Ctrl Pts',(2.00750152695864,-5.56823473535495,4.59725683954159));
#14706=CARTESIAN_POINT('Ctrl Pts',(1.85036125985648,-5.61997275531851,4.58946856126603));
#14707=CARTESIAN_POINT('Ctrl Pts',(1.70096785579821,-5.66916014098438,4.58206423756979));
#14708=CARTESIAN_POINT('Ctrl Pts',(1.54962953328846,-5.71238150906856,4.57465991387354));
#14709=CARTESIAN_POINT('Ctrl Pts',(1.39683662901192,-5.74950241276153,4.5672555901773));
#14710=CARTESIAN_POINT('Ctrl Pts',(1.23612678035569,-5.78854673123119,4.55946761241577));
#14711=CARTESIAN_POINT('Ctrl Pts',(1.07375012094943,-5.82085557831578,4.55167963465424));
#14712=CARTESIAN_POINT('Ctrl Pts',(0.910285670327234,-5.8463074295573,4.54389165689271));
#14713=CARTESIAN_POINT('Ctrl Pts',(0.746853358215883,-5.87175427674691,
4.5361052103143));
#14714=CARTESIAN_POINT('Ctrl Pts',(0.582333997172172,-5.89034676890564,
4.5283187637359));
#14715=CARTESIAN_POINT('Ctrl Pts',(0.41731509878028,-5.90201479757803,4.52053231715749));
#14716=CARTESIAN_POINT('Ctrl Pts',(0.252289905290521,-5.91368327135933,
4.51274557354375));
#14717=CARTESIAN_POINT('Ctrl Pts',(0.0867654547850066,-5.91842672659838,
4.50495882993001));
#14718=CARTESIAN_POINT('Ctrl Pts',(-0.0786665887883952,-5.91622701815172,
4.49717208631627));
#14719=CARTESIAN_POINT('Ctrl Pts',(-0.244087690269642,-5.91402745519931,
4.48938585773737));
#14720=CARTESIAN_POINT('Ctrl Pts',(-0.409416077502845,-5.90488565192815,
4.48159962915847));
#14721=CARTESIAN_POINT('Ctrl Pts',(-0.574060907248223,-5.88883559265067,
4.47381340057958));
#14722=CARTESIAN_POINT('Ctrl Pts',(-0.738749079153502,-5.87278130825275,
4.46602512230398));
#14723=CARTESIAN_POINT('Ctrl Pts',(-0.902753015560587,-5.84981516303304,
4.45823684402838));
#14724=CARTESIAN_POINT('Ctrl Pts',(-1.06548689623019,-5.82002304432394,
4.45044856575278));
#14725=CARTESIAN_POINT('Ctrl Pts',(-1.22019815411625,-5.79169964822715,
4.44304424205678));
#14726=CARTESIAN_POINT('Ctrl Pts',(-1.37376130562372,-5.75720714155376,
4.43563991836078));
#14727=CARTESIAN_POINT('Ctrl Pts',(-1.52568148163822,-5.71666218864524,
4.42823559466477));
#14728=CARTESIAN_POINT('Ctrl Pts',(-1.68547338173633,-5.67401640429582,
4.42044761690326));
#14729=CARTESIAN_POINT('Ctrl Pts',(-1.84350468551456,-5.62465905280796,
4.41265963914175));
#14730=CARTESIAN_POINT('Ctrl Pts',(-1.99920884614788,-5.56876059388299,
4.40487166138024));
#14731=CARTESIAN_POINT('Ctrl Pts',(-2.1548823940093,-5.51287312507393,4.39708521480188));
#14732=CARTESIAN_POINT('Ctrl Pts',(-2.30822941107405,-5.45044722275815,
4.38929876822352));
#14733=CARTESIAN_POINT('Ctrl Pts',(-2.45870050568853,-5.38170255456644,
4.38151232164515));
#14734=CARTESIAN_POINT('Ctrl Pts',(-2.60917734043562,-5.31295526392082,
4.37372557803143));
#14735=CARTESIAN_POINT('Ctrl Pts',(-2.75677774091444,-5.23788885424812,
4.3659388344177));
#14736=CARTESIAN_POINT('Ctrl Pts',(-2.9009735428508,-5.15677060437825,4.35815209080398));
#14737=CARTESIAN_POINT('Ctrl Pts',(-3.04515980731366,-5.07565771987373,
4.35036586222509));
#14738=CARTESIAN_POINT('Ctrl Pts',(-3.18594164539739,-4.98849395298694,
4.34257963364619));
#14739=CARTESIAN_POINT('Ctrl Pts',(-3.32281656607375,-4.89559195917366,
4.3347934050673));
#14740=CARTESIAN_POINT('Ctrl Pts',(-3.45972751858079,-4.80266550924459,
4.32700512679174));
#14741=CARTESIAN_POINT('Ctrl Pts',(-3.59272923288249,-4.70399799191563,
4.31921684851617));
#14742=CARTESIAN_POINT('Ctrl Pts',(-3.72134847240647,-4.5999452289585,4.31142857024061));
#14743=CARTESIAN_POINT('Ctrl Pts',(-3.84362690793325,-4.50102216648567,
4.3040242465445));
#14744=CARTESIAN_POINT('Ctrl Pts',(-3.96194435858801,-4.39723220845113,
4.29661992284838));
#14745=CARTESIAN_POINT('Ctrl Pts',(-4.07592217450273,-4.28891466339643,
4.28921559915227));
#14746=CARTESIAN_POINT('Ctrl Pts',(-4.19580573606494,-4.1749846588897,4.28142762139076));
#14747=CARTESIAN_POINT('Ctrl Pts',(-4.31093089259036,-4.05600466286206,
4.27363964362924));
#14748=CARTESIAN_POINT('Ctrl Pts',(-4.42088181152369,-3.93239552576276,
4.26585166586773));
#14749=CARTESIAN_POINT('Ctrl Pts',(-4.53081111316369,-3.80881069127959,
4.25806521928942));
#14750=CARTESIAN_POINT('Ctrl Pts',(-4.63556799477428,-3.68059877031486,
4.25027877271111));
#14751=CARTESIAN_POINT('Ctrl Pts',(-4.73477524020605,-3.5482156060803,4.24249232613279));
#14752=CARTESIAN_POINT('Ctrl Pts',(-4.83398627017057,-3.41582739172646,
4.2347055825191));
#14753=CARTESIAN_POINT('Ctrl Pts',(-4.92764704553999,-3.27926786902791,
4.2269188389054));
#14754=CARTESIAN_POINT('Ctrl Pts',(-5.01542177765188,-3.13902452280247,
4.2191320952917));
#14755=CARTESIAN_POINT('Ctrl Pts',(-5.10319070412162,-2.99879045262564,
4.21134586671287));
#14756=CARTESIAN_POINT('Ctrl Pts',(-5.18507419696735,-2.85487331747097,
4.20355963813403));
#14757=CARTESIAN_POINT('Ctrl Pts',(-5.26078072885105,-2.70778815372426,
4.19577340955519));
#14758=CARTESIAN_POINT('Ctrl Pts',(-5.33650719020755,-2.56066427033609,
4.18798513127963));
#14759=CARTESIAN_POINT('Ctrl Pts',(-5.40605329330799,-2.41037097532072,
4.18019685300407));
#14760=CARTESIAN_POINT('Ctrl Pts',(-5.46917385842482,-2.25744720177959,
4.1724085747285));
#14761=CARTESIAN_POINT('Ctrl Pts',(-5.52918264078712,-2.11206242223167,
4.16500425103225));
#14762=CARTESIAN_POINT('Ctrl Pts',(-5.58338406900463,-1.96430052017851,
4.157599927336));
#14763=CARTESIAN_POINT('Ctrl Pts',(-5.6316081057873,-1.81464065460103,4.15019560363975));
#14764=CARTESIAN_POINT('Ctrl Pts',(-5.68244884304267,-1.65686004536271,
4.1423895114768));
#14765=CARTESIAN_POINT('Ctrl Pts',(-5.7266635347264,-1.49691390443455,4.13458341931385));
#14766=CARTESIAN_POINT('Ctrl Pts',(-5.7640878260625,-1.33537339195374,4.12677732715091));
#14767=CARTESIAN_POINT('Ctrl Pts',(-5.80150366642566,-1.17386935777223,
4.11897299772204));
#14768=CARTESIAN_POINT('Ctrl Pts',(-5.83213209537172,-1.01077197874193,
4.11116866829317));
#14769=CARTESIAN_POINT('Ctrl Pts',(-5.85585942190165,-0.846664628661034,
4.1033643388643));
#14770=CARTESIAN_POINT('Ctrl Pts',(-5.87958536060331,-0.68256687733616,
4.09556046591623));
#14771=CARTESIAN_POINT('Ctrl Pts',(-5.89641095468099,-0.517459585638993,
4.08775659296816));
#14772=CARTESIAN_POINT('Ctrl Pts',(-5.90627404008611,-0.351933979469085,
4.07995272002008));
#14773=CARTESIAN_POINT('Ctrl Pts',(-5.91325798996735,-0.234726990979063,
4.07442687741502));
#14774=CARTESIAN_POINT('Ctrl Pts',(-5.91675207616837,-0.117310438061947,
4.06890103480996));
#14775=CARTESIAN_POINT('Ctrl Pts',(-5.9167499990742,0.000104668362501446,
4.0633751922049));
#14776=CARTESIAN_POINT('Ctrl Pts',(-5.91674999969049,6.05192443194444E-5,
3.81162480779512));
#14777=CARTESIAN_POINT('Ctrl Pts',(-5.91675170265655,-0.166432379585355,
3.81945993587964));
#14778=CARTESIAN_POINT('Ctrl Pts',(-5.90972158488872,-0.332919670560517,
3.82729506396416));
#14779=CARTESIAN_POINT('Ctrl Pts',(-5.89568710169516,-0.498802727944986,
3.83513019204868));
#14780=CARTESIAN_POINT('Ctrl Pts',(-5.88165217523655,-0.66469102457914,
3.84296556759785));
#14781=CARTESIAN_POINT('Ctrl Pts',(-5.86061247156367,-0.829974739898137,
3.85080094314702));
#14782=CARTESIAN_POINT('Ctrl Pts',(-5.83264735018096,-0.994060084163459,
3.85863631869618));
#14783=CARTESIAN_POINT('Ctrl Pts',(-5.80467542214537,-1.15818536646322,
3.8664736013596));
#14784=CARTESIAN_POINT('Ctrl Pts',(-5.76977476205297,-1.32111138849058,
3.87431088402302));
#14785=CARTESIAN_POINT('Ctrl Pts',(-5.72807605569632,-1.48225344076459,
3.88214816668644));
#14786=CARTESIAN_POINT('Ctrl Pts',(-5.7132660711512,-1.53948570315986,3.8849317071188));
#14787=CARTESIAN_POINT('Ctrl Pts',(-5.69759902536455,-1.59649303911082,
3.88771524755117));
#14788=CARTESIAN_POINT('Ctrl Pts',(-5.68108230430109,-1.65324965273157,
3.89049878798353));
#14789=CARTESIAN_POINT('Ctrl Pts',(-5.63486991162358,-1.81204987134696,
3.89828689937681));
#14790=CARTESIAN_POINT('Ctrl Pts',(-5.58198681330044,-1.96893960167442,
3.9060750107701));
#14791=CARTESIAN_POINT('Ctrl Pts',(-5.52261612359663,-2.12335623810292,
3.91386312216338));
#14792=CARTESIAN_POINT('Ctrl Pts',(-5.46325709029263,-2.27774255751705,
3.92164970449678));
#14793=CARTESIAN_POINT('Ctrl Pts',(-5.39741312166799,-2.4296564537871,3.92943628683017));
#14794=CARTESIAN_POINT('Ctrl Pts',(-5.32531614323966,-2.57855357459392,
3.93722286916356));
#14795=CARTESIAN_POINT('Ctrl Pts',(-5.25321641576972,-2.72745637281455,
3.9450097483976));
#14796=CARTESIAN_POINT('Ctrl Pts',(-5.17486333709895,-2.87334187610095,
3.95279662763163));
#14797=CARTESIAN_POINT('Ctrl Pts',(-5.09053595632954,-3.01568802096903,
3.96058350686566));
#14798=CARTESIAN_POINT('Ctrl Pts',(-5.00621414111842,-3.15802477107398,
3.96836987217018));
#14799=CARTESIAN_POINT('Ctrl Pts',(-4.915918975838,-3.29682235535044,3.97615623747469));
#14800=CARTESIAN_POINT('Ctrl Pts',(-4.81997429984372,-3.43158539327613,
3.9839426027792));
#14801=CARTESIAN_POINT('Ctrl Pts',(-4.72400443072594,-3.56638381723883,
3.99173101262512));
#14802=CARTESIAN_POINT('Ctrl Pts',(-4.62238227051841,-3.69714531637354,
3.99951942247104));
#14803=CARTESIAN_POINT('Ctrl Pts',(-4.5154741581875,-3.82340472475003,4.00730783231695));
#14804=CARTESIAN_POINT('Ctrl Pts',(-4.41418427659883,-3.94302895386678,
4.01468694596752));
#14805=CARTESIAN_POINT('Ctrl Pts',(-4.30814989558855,-4.05861191050198,
4.02206605961808));
#14806=CARTESIAN_POINT('Ctrl Pts',(-4.19771511701581,-4.16978636849383,
4.02944517326865));
#14807=CARTESIAN_POINT('Ctrl Pts',(-4.08115933567149,-4.28712282702836,
4.0372332846615));
#14808=CARTESIAN_POINT('Ctrl Pts',(-3.95965990039923,-4.39959014137331,
4.04502139605436));
#14809=CARTESIAN_POINT('Ctrl Pts',(-3.83364677837878,-4.50678188302096,
4.05280950744722));
#14810=CARTESIAN_POINT('Ctrl Pts',(-3.70765839683829,-4.61395257943862,
4.06059608978016));
#14811=CARTESIAN_POINT('Ctrl Pts',(-3.57715833998378,-4.71584956291699,
4.0683826721131));
#14812=CARTESIAN_POINT('Ctrl Pts',(-3.44261070425107,-4.81210578660486,
4.07616925444604));
#14813=CARTESIAN_POINT('Ctrl Pts',(-3.30805793824688,-4.90836568052116,
4.08395613367964));
#14814=CARTESIAN_POINT('Ctrl Pts',(-3.16945754210906,-4.99898419515117,
4.09174301291324));
#14815=CARTESIAN_POINT('Ctrl Pts',(-3.02730432880461,-5.08363640156344,
4.09952989214684));
#14816=CARTESIAN_POINT('Ctrl Pts',(-2.88516049752988,-5.16828302097913,
4.10731625745092));
#14817=CARTESIAN_POINT('Ctrl Pts',(-2.73946459294543,-5.246963956779,4.115102622755));
#14818=CARTESIAN_POINT('Ctrl Pts',(-2.59073799329216,-5.31939914018609,
4.12288898805908));
#14819=CARTESIAN_POINT('Ctrl Pts',(-2.441972341054,-5.3918533436014,4.13067739790457));
#14820=CARTESIAN_POINT('Ctrl Pts',(-2.29017469018288,-5.4580583757989,4.13846580775006));
#14821=CARTESIAN_POINT('Ctrl Pts',(-2.13588928307182,-5.51778103343717,
4.14625421759555));
#14822=CARTESIAN_POINT('Ctrl Pts',(-1.98971187630749,-5.57436514843614,
4.15363333124829));
#14823=CARTESIAN_POINT('Ctrl Pts',(-1.84130170356482,-5.62513059398553,
4.16101244490103));
#14824=CARTESIAN_POINT('Ctrl Pts',(-1.691136622487,-5.66991953087372,4.16839155855377));
#14825=CARTESIAN_POINT('Ctrl Pts',(-1.53264843084162,-5.71719095750752,
4.17617966994674));
#14826=CARTESIAN_POINT('Ctrl Pts',(-1.37214867412026,-5.75782145911191,
4.18396778133971));
#14827=CARTESIAN_POINT('Ctrl Pts',(-1.21020936604839,-5.791659852998,4.19175589273268));
#14828=CARTESIAN_POINT('Ctrl Pts',(-1.04830185193705,-5.82549160330525,
4.19954247506573));
#14829=CARTESIAN_POINT('Ctrl Pts',(-0.884955662987656,-5.85253384133118,
4.20732905739877));
#14830=CARTESIAN_POINT('Ctrl Pts',(-0.720753941031261,-5.87268629495803,
4.21511563973182));
#14831=CARTESIAN_POINT('Ctrl Pts',(-0.556545958099245,-5.89283951699352,
4.22290251896554));
#14832=CARTESIAN_POINT('Ctrl Pts',(-0.391482693540322,-5.90610238611409,
4.23068939819926));
#14833=CARTESIAN_POINT('Ctrl Pts',(-0.22615411137466,-5.9124263107804,4.23847627743298));
#14834=CARTESIAN_POINT('Ctrl Pts',(-0.0608364408003028,-5.91874981807133,
4.24626264273715));
#14835=CARTESIAN_POINT('Ctrl Pts',(0.104746193014632,-5.91813528527265,
4.25404900804133));
#14836=CARTESIAN_POINT('Ctrl Pts',(0.270001961156384,-5.91058622333451,
4.2618353733455));
#14837=CARTESIAN_POINT('Ctrl Pts',(0.435301122107437,-5.90303517916598,
4.2696237831911));
#14838=CARTESIAN_POINT('Ctrl Pts',(0.600272926388305,-5.8885459800386,4.2774121930367));
#14839=CARTESIAN_POINT('Ctrl Pts',(0.764327889628312,-5.8671742295279,4.28520060288231));
#14840=CARTESIAN_POINT('Ctrl Pts',(0.919761443197456,-5.84692560636975,
4.2925797165345));
#14841=CARTESIAN_POINT('Ctrl Pts',(1.07437178288583,-5.82049924276928,4.2999588301867));
#14842=CARTESIAN_POINT('Ctrl Pts',(1.22766377514444,-5.78798516045939,4.30733794383889));
#14843=CARTESIAN_POINT('Ctrl Pts',(1.3894521914279,-5.75366893945971,4.31512605523189));
#14844=CARTESIAN_POINT('Ctrl Pts',(1.54982975620371,-5.71255876693495,4.32291416662489));
#14845=CARTESIAN_POINT('Ctrl Pts',(1.70822184003281,-5.66479555745262,4.33070227801789));
#14846=CARTESIAN_POINT('Ctrl Pts',(1.86658282633796,-5.61704172544368,4.338488860351));
#14847=CARTESIAN_POINT('Ctrl Pts',(2.02295880375937,-5.56263755494402,4.34627544268412));
#14848=CARTESIAN_POINT('Ctrl Pts',(2.17678972842697,-5.50177399033392,4.35406202501724));
#14849=CARTESIAN_POINT('Ctrl Pts',(2.33062651863303,-5.44090810500983,4.36184890425099));
#14850=CARTESIAN_POINT('Ctrl Pts',(2.48191776334469,-5.37358244661775,4.36963578348473));
#14851=CARTESIAN_POINT('Ctrl Pts',(2.63012215378309,-5.30003660540938,4.37742266271847));
#14852=CARTESIAN_POINT('Ctrl Pts',(2.77831676281692,-5.22649561818426,4.38520902802267));
#14853=CARTESIAN_POINT('Ctrl Pts',(2.92342463908043,-5.14673541182737,4.39299539332686));
#14854=CARTESIAN_POINT('Ctrl Pts',(3.06492776385741,-5.06104222120662,4.40078175863105));
#14855=CARTESIAN_POINT('Ctrl Pts',(3.20646804448182,-4.97532652929395,4.40857016847668));
#14856=CARTESIAN_POINT('Ctrl Pts',(3.34440140774417,-4.88367490411294,4.4163585783223));
#14857=CARTESIAN_POINT('Ctrl Pts',(3.47823681667403,-4.78641820254283,4.42414698816793));
#14858=CARTESIAN_POINT('Ctrl Pts',(3.60503891270324,-4.69427253114999,4.43152610181996));
#14859=CARTESIAN_POINT('Ctrl Pts',(3.72816247695504,-4.59709589940894,4.43890521547199));
#14860=CARTESIAN_POINT('Ctrl Pts',(3.84721579092943,-4.49520424680829,4.44628432912403));
#14861=CARTESIAN_POINT('Ctrl Pts',(3.97286780208609,-4.38766510621703,4.45407244051697));
#14862=CARTESIAN_POINT('Ctrl Pts',(4.09403044633948,-4.27483504282268,4.46186055190991));
#14863=CARTESIAN_POINT('Ctrl Pts',(4.21026654696066,-4.15711271991077,4.46964866330286));
#14864=CARTESIAN_POINT('Ctrl Pts',(4.32647982664957,-4.03941350972498,4.47743524563588));
#14865=CARTESIAN_POINT('Ctrl Pts',(4.43776826827729,-3.91682418375546,4.4852218279689));
#14866=CARTESIAN_POINT('Ctrl Pts',(4.54373143906263,-3.78978035935776,4.49300841030193));
#14867=CARTESIAN_POINT('Ctrl Pts',(4.64969865020016,-3.66273169080723,4.50079528953561));
#14868=CARTESIAN_POINT('Ctrl Pts',(4.75033997650185,-3.53122842680167,4.50858216876929));
#14869=CARTESIAN_POINT('Ctrl Pts',(4.84529471079806,-3.39573993821852,4.51636904800297));
#14870=CARTESIAN_POINT('Ctrl Pts',(4.94024317813675,-3.26026039179723,4.52415541330713));
#14871=CARTESIAN_POINT('Ctrl Pts',(5.02950562122506,-3.1207964089004,4.53194177861128));
#14872=CARTESIAN_POINT('Ctrl Pts',(5.11276410085828,-2.97784717732035,4.53972814391544));
#14873=CARTESIAN_POINT('Ctrl Pts',(5.19604444247748,-2.83486041017504,4.547516553761));
#14874=CARTESIAN_POINT('Ctrl Pts',(5.27331750782913,-2.6883868409896,4.55530496360657));
#14875=CARTESIAN_POINT('Ctrl Pts',(5.34431039973913,-2.53895193214448,4.56309337345213));
#14876=CARTESIAN_POINT('Ctrl Pts',(5.4115724761193,-2.39737012047034,4.57047248710447));
#14877=CARTESIAN_POINT('Ctrl Pts',(5.47319736093624,-2.25313044699605,4.57785160075682));
#14878=CARTESIAN_POINT('Ctrl Pts',(5.52899223382608,-2.10669775734226,4.58523071440916));
#14879=CARTESIAN_POINT('Ctrl Pts',(5.58787961592861,-1.95214883015016,4.59301882580214));
#14880=CARTESIAN_POINT('Ctrl Pts',(5.6402934184301,-1.79510169430975,4.60080693719513));
#14881=CARTESIAN_POINT('Ctrl Pts',(5.68604048103982,-1.63611558591575,4.60859504858811));
#14882=CARTESIAN_POINT('Ctrl Pts',(5.73177856201124,-1.47716069167274,4.61638163092118));
#14883=CARTESIAN_POINT('Ctrl Pts',(5.77085242642958,-1.31626789133242,4.62416821325426));
#14884=CARTESIAN_POINT('Ctrl Pts',(5.80311885983356,-1.15401129160161,4.63195479558733));
#14885=CARTESIAN_POINT('Ctrl Pts',(5.83538652354945,-0.991748505062883,
4.63974167482105));
#14886=CARTESIAN_POINT('Ctrl Pts',(5.86084617066828,-0.828122127688309,
4.64752855405476));
#14887=CARTESIAN_POINT('Ctrl Pts',(5.87940561957024,-0.663716899789279,
4.65531543328848));
#14888=CARTESIAN_POINT('Ctrl Pts',(5.89796384355929,-0.499322522540363,
4.66310179859267));
#14889=CARTESIAN_POINT('Ctrl Pts',(5.90962274494601,-0.334149715183336,
4.67088816389685));
#14890=CARTESIAN_POINT('Ctrl Pts',(5.91434196310038,-0.168788939240627,
4.67867452920103));
#14891=CARTESIAN_POINT('Ctrl Pts',(5.9190624204256,-0.00338474291599597,
4.68646293904664));
#14892=CARTESIAN_POINT('Ctrl Pts',(5.91683954228149,0.162207201066173,4.69425134889224));
#14893=CARTESIAN_POINT('Ctrl Pts',(5.90768509116275,0.327394908563692,4.70203975873784));
#14894=CARTESIAN_POINT('Ctrl Pts',(5.89901172438219,0.483901678459688,4.70941887238999));
#14895=CARTESIAN_POINT('Ctrl Pts',(5.88411659620163,0.64004534623984,4.71679798604213));
#14896=CARTESIAN_POINT('Ctrl Pts',(5.86305278519524,0.795325468292249,4.72417709969428));
#14897=CARTESIAN_POINT('Ctrl Pts',(5.84082148287208,0.959212209256606,4.73196521108723));
#14898=CARTESIAN_POINT('Ctrl Pts',(5.81171035141862,1.12219549549672,4.73975332248018));
#14899=CARTESIAN_POINT('Ctrl Pts',(5.77581733064287,1.28369183433777,4.74754143387314));
#14900=CARTESIAN_POINT('Ctrl Pts',(5.73993135683605,1.44515646618796,4.75532801620618));
#14901=CARTESIAN_POINT('Ctrl Pts',(5.69726621973851,1.6051344214137,4.76311459853923));
#14902=CARTESIAN_POINT('Ctrl Pts',(5.64797083235644,1.76305304496234,4.77090118087228));
#14903=CARTESIAN_POINT('Ctrl Pts',(5.59867356535214,1.92097768991315,4.77868806010599));
#14904=CARTESIAN_POINT('Ctrl Pts',(5.54274563362964,2.07684253988684,4.7864749393397));
#14905=CARTESIAN_POINT('Ctrl Pts',(5.48038585078946,2.23009001813082,4.79426181857341));
#14906=CARTESIAN_POINT('Ctrl Pts',(5.41803018365886,2.38332738212992,4.80204818387759));
#14907=CARTESIAN_POINT('Ctrl Pts',(5.3492436354497,2.53394742414701,4.80983454918178));
#14908=CARTESIAN_POINT('Ctrl Pts',(5.27427326218566,2.68141233649236,4.81762091448596));
#14909=CARTESIAN_POINT('Ctrl Pts',(5.19928320322401,2.82891597012916,4.82540932433156));
#14910=CARTESIAN_POINT('Ctrl Pts',(5.11810621779466,2.97326253273323,4.83319773417716));
#14911=CARTESIAN_POINT('Ctrl Pts',(5.03103586090187,3.11393781710865,4.84098614402276));
#14912=CARTESIAN_POINT('Ctrl Pts',(4.94854122181793,3.24722033973423,4.84836525767497));
#14913=CARTESIAN_POINT('Ctrl Pts',(4.86075683288408,3.37720730404721,4.85574437132718));
#14914=CARTESIAN_POINT('Ctrl Pts',(4.76796873347935,3.50348465375023,4.8631234849794));
#14915=CARTESIAN_POINT('Ctrl Pts',(4.67003772331103,3.63676110296223,4.87091159637238));
#14916=CARTESIAN_POINT('Ctrl Pts',(4.56649762274021,3.76595265509376,4.87869970776537));
#14917=CARTESIAN_POINT('Ctrl Pts',(4.45771359841966,3.89059378976583,4.88648781915836));
#14918=CARTESIAN_POINT('Ctrl Pts',(4.34895093194651,4.01521045332322,4.8942744014914));
#14919=CARTESIAN_POINT('Ctrl Pts',(4.23494660596614,4.13527824142421,4.90206098382444));
#14920=CARTESIAN_POINT('Ctrl Pts',(4.11610536275955,4.25036553782873,4.90984756615748));
#14921=CARTESIAN_POINT('Ctrl Pts',(3.99725958816233,4.3654572224867,4.9176344453912));
#14922=CARTESIAN_POINT('Ctrl Pts',(3.87357675407428,4.47556781033418,4.92542132462493));
#14923=CARTESIAN_POINT('Ctrl Pts',(3.74549820763692,4.58030279993459,4.93320820385865));
#14924=CARTESIAN_POINT('Ctrl Pts',(3.61742811430956,4.68503087708625,4.94099456916284));
#14925=CARTESIAN_POINT('Ctrl Pts',(3.48496313664534,4.78438386377635,4.94878093446704));
#14926=CARTESIAN_POINT('Ctrl Pts',(3.34857752634194,4.87800769911013,4.95656729977124));
#14927=CARTESIAN_POINT('Ctrl Pts',(3.21215610394682,4.97165611816187,4.96435570961684));
#14928=CARTESIAN_POINT('Ctrl Pts',(3.07181225430668,5.05957219727864,4.97214411946245));
#14929=CARTESIAN_POINT('Ctrl Pts',(2.92804976962699,5.14144484645001,4.97993252930806));
#14930=CARTESIAN_POINT('Ctrl Pts',(2.79184228512156,5.21901492753392,4.98731164296022));
#14931=CARTESIAN_POINT('Ctrl Pts',(2.65256646183692,5.29116030077305,4.99469075661238));
#14932=CARTESIAN_POINT('Ctrl Pts',(2.51067157661488,5.35765422520697,5.00206987026453));
#14933=CARTESIAN_POINT('Ctrl Pts',(2.360911968037,5.42783366881729,5.00985798165748));
#14934=CARTESIAN_POINT('Ctrl Pts',(2.20818124795279,5.4917424844114,5.01764609305043));
#14935=CARTESIAN_POINT('Ctrl Pts',(2.05302279890085,5.54914659652215,5.02543420444338));
#14936=CARTESIAN_POINT('Ctrl Pts',(1.89789481250508,5.60653943833637,5.03322078677644));
#14937=CARTESIAN_POINT('Ctrl Pts',(1.74034034767591,5.65743001402864,5.04100736910951));
#14938=CARTESIAN_POINT('Ctrl Pts',(1.5809213182788,5.70163295450625,5.04879395144258));
#14939=CARTESIAN_POINT('Ctrl Pts',(1.42149621026995,5.74583758043203,5.05658083067628));
#14940=CARTESIAN_POINT('Ctrl Pts',(1.26020670227525,5.78335397171438,5.06436770990998));
#14941=CARTESIAN_POINT('Ctrl Pts',(1.09762909469295,5.8140468636728,5.07215458914368));
#14942=CARTESIAN_POINT('Ctrl Pts',(0.935062217138572,5.84473772991813,5.07994095444787));
#14943=CARTESIAN_POINT('Ctrl Pts',(0.771207724150727,5.86860593888792,5.08772731975205));
#14944=CARTESIAN_POINT('Ctrl Pts',(0.606651462188195,5.88556748036457,5.09551368505623));
#14945=CARTESIAN_POINT('Ctrl Pts',(0.442051991092846,5.90253347559757,5.10330209490183));
#14946=CARTESIAN_POINT('Ctrl Pts',(0.276750700666946,5.912589144771,5.11109050474743));
#14947=CARTESIAN_POINT('Ctrl Pts',(0.111338818777101,5.91570234460232,5.11887891459302));
#14948=CARTESIAN_POINT('Ctrl Pts',(-0.0453803447093223,5.91865193968433,
5.12625802824523));
#14949=CARTESIAN_POINT('Ctrl Pts',(-0.202198514988835,5.91536997350762,
5.13363714189745));
#14950=CARTESIAN_POINT('Ctrl Pts',(-0.358612690940003,5.90587228954341,
5.14101625554966));
#14951=CARTESIAN_POINT('Ctrl Pts',(-0.523696342332037,5.89584818310266,
5.14880436694261));
#14952=CARTESIAN_POINT('Ctrl Pts',(-0.688388904989159,5.87889621054729,
5.15659247833555));
#14953=CARTESIAN_POINT('Ctrl Pts',(-0.852101232342855,5.85507079823462,
5.1643805897285));
#14954=CARTESIAN_POINT('Ctrl Pts',(-1.01578141763601,5.83125006362617,5.17216717206159));
#14955=CARTESIAN_POINT('Ctrl Pts',(-1.17848143562264,5.80055862786281,5.17995375439468));
#14956=CARTESIAN_POINT('Ctrl Pts',(-1.3396191698002,5.76310255352131,5.18774033672778));
#14957=CARTESIAN_POINT('Ctrl Pts',(-1.50076304812304,5.72564505098818,5.19552721596149));
#14958=CARTESIAN_POINT('Ctrl Pts',(-1.66034421132565,5.68142246224671,5.2033140951952));
#14959=CARTESIAN_POINT('Ctrl Pts',(-1.81779188148033,5.63059173072637,5.21110097442891));
#14960=CARTESIAN_POINT('Ctrl Pts',(-1.97522916017909,5.57976435400516,5.21888733973306));
#14961=CARTESIAN_POINT('Ctrl Pts',(-2.13053292354879,5.52232980556348,5.2266737050372));
#14962=CARTESIAN_POINT('Ctrl Pts',(-2.28314853299054,5.45849460371659,5.23446007034135));
#14963=CARTESIAN_POINT('Ctrl Pts',(-2.43580421619259,5.39464264004182,5.24224848018693));
#14964=CARTESIAN_POINT('Ctrl Pts',(-2.58577003929812,5.3243867861991,5.25003689003252));
#14965=CARTESIAN_POINT('Ctrl Pts',(-2.73251145314194,5.2479816806986,5.2578252998781));
#14966=CARTESIAN_POINT('Ctrl Pts',(-2.87154131825056,5.1755918131548,5.26520441353032));
#14967=CARTESIAN_POINT('Ctrl Pts',(-3.0076767248299,5.09768250108378,5.27258352718255));
#14968=CARTESIAN_POINT('Ctrl Pts',(-3.1404835561888,5.0145083104735,5.27996264083478));
#14969=CARTESIAN_POINT('Ctrl Pts',(-3.28065139275001,4.92672407350102,5.28775075222776));
#14970=CARTESIAN_POINT('Ctrl Pts',(-3.41716126991424,4.83304342979636,5.29553886362074));
#14971=CARTESIAN_POINT('Ctrl Pts',(-3.54952188412015,4.73379604088011,5.30332697501372));
#14972=CARTESIAN_POINT('Ctrl Pts',(-3.6818565116268,4.63456813745856,5.31111355734679));
#14973=CARTESIAN_POINT('Ctrl Pts',(-3.81004324612876,4.52977586112265,5.31890013967987));
#14974=CARTESIAN_POINT('Ctrl Pts',(-3.93362166191435,4.41979085290449,5.32668672201294));
#14975=CARTESIAN_POINT('Ctrl Pts',(-4.05720478971704,4.30980165098279,5.33447360124664));
#14976=CARTESIAN_POINT('Ctrl Pts',(-4.17617900589712,4.194619530459,5.34226048048034));
#14977=CARTESIAN_POINT('Ctrl Pts',(-4.29011818459847,4.07465538722939,5.35004735971404));
#14978=CARTESIAN_POINT('Ctrl Pts',(-4.40404984337992,3.95469916156387,5.35783372501822));
#14979=CARTESIAN_POINT('Ctrl Pts',(-4.5129469097056,3.82996177656109,5.36562009032239));
#14980=CARTESIAN_POINT('Ctrl Pts',(-4.616421148406,3.70088993933213,5.37340645562657));
#14981=CARTESIAN_POINT('Ctrl Pts',(-4.71992255734045,3.57178421045952,5.38119486547217));
#14982=CARTESIAN_POINT('Ctrl Pts',(-4.81799809184262,3.43834200337669,5.38898327531777));
#14983=CARTESIAN_POINT('Ctrl Pts',(-4.91030018013144,3.30104266914275,5.39677168516337));
#14984=CARTESIAN_POINT('Ctrl Pts',(-4.99775161287817,3.17095868386651,5.40415079881555));
#14985=CARTESIAN_POINT('Ctrl Pts',(-5.08002065862202,3.03741275939119,5.41152991246773));
#14986=CARTESIAN_POINT('Ctrl Pts',(-5.15684790293272,2.90083613265528,5.4189090261199));
#14987=CARTESIAN_POINT('Ctrl Pts',(-5.23793340519082,2.75668955451155,5.42669713751287));
#14988=CARTESIAN_POINT('Ctrl Pts',(-5.31298572089407,2.60911530379078,5.43448524890584));
#14989=CARTESIAN_POINT('Ctrl Pts',(-5.38173114686707,2.45863792074817,5.44227336029881));
#14990=CARTESIAN_POINT('Ctrl Pts',(-5.45046307587361,2.30819008131754,5.45005994263181));
#14991=CARTESIAN_POINT('Ctrl Pts',(-5.51289045312819,2.15484053729931,5.45784652496482));
#14992=CARTESIAN_POINT('Ctrl Pts',(-5.56878677447868,1.99913591906386,5.46563310729783));
#14993=CARTESIAN_POINT('Ctrl Pts',(-5.62468522714398,1.84342536384454,5.47341998653156));
#14994=CARTESIAN_POINT('Ctrl Pts',(-5.67405201392717,1.68535985411224,5.48120686576529));
#14995=CARTESIAN_POINT('Ctrl Pts',(-5.71670953107353,1.52550408056912,5.48899374499902));
#14996=CARTESIAN_POINT('Ctrl Pts',(-5.75936423284837,1.36565885741484,5.49678011030321));
#14997=CARTESIAN_POINT('Ctrl Pts',(-5.79531046883721,1.20402391567871,5.5045664756074));
#14998=CARTESIAN_POINT('Ctrl Pts',(-5.82442104131012,1.04117726446746,5.5123528409116));
#14999=CARTESIAN_POINT('Ctrl Pts',(-5.85353925762824,0.878287853032396,
5.52014125075721));
#15000=CARTESIAN_POINT('Ctrl Pts',(-5.87581816565748,0.714186410759292,
5.52792966060282));
#15001=CARTESIAN_POINT('Ctrl Pts',(-5.89118189313341,0.549460157351797,
5.53571807044843));
#15002=CARTESIAN_POINT('Ctrl Pts',(-5.90573822663585,0.393390591228442,
5.54309718410063));
#15003=CARTESIAN_POINT('Ctrl Pts',(-5.91408747402153,0.236760453962896,
5.55047629775283));
#15004=CARTESIAN_POINT('Ctrl Pts',(-5.91620815651611,0.0800725375658166,
5.55785541140503));
#15005=CARTESIAN_POINT('Ctrl Pts',(-5.91656925195911,0.0533927810586914,
5.5591118768684));
#15006=CARTESIAN_POINT('Ctrl Pts',(-5.91674987283727,0.0267105792375199,
5.56036834233176));
#15007=CARTESIAN_POINT('Ctrl Pts',(-5.91674999993288,2.81831104758398E-5,
5.56162480779512));
#15008=CARTESIAN_POINT('Origin',(0.,0.,0.));
#15009=CARTESIAN_POINT('',(-5.91674999981411,-4.69009224444681E-5,7.56337519225006));
#15010=CARTESIAN_POINT('',(-5.91674999911038,-0.000102602491467883,7.31162480779513));
#15011=CARTESIAN_POINT('',(-5.91675,-7.2459289488551E-16,0.));
#15012=CARTESIAN_POINT('Ctrl Pts',(-5.91674999981412,-4.68999629195391E-5,
7.5633751922049));
#15013=CARTESIAN_POINT('Ctrl Pts',(-5.91675132125532,0.166661914366294,
7.55552998692111));
#15014=CARTESIAN_POINT('Ctrl Pts',(-5.90970258340904,0.333362748204337,
7.54768478163732));
#15015=CARTESIAN_POINT('Ctrl Pts',(-5.89563183882621,0.499455487024331,
7.53983957635354));
#15016=CARTESIAN_POINT('Ctrl Pts',(-5.88156043435222,0.665556015277763,
7.53199400314455));
#15017=CARTESIAN_POINT('Ctrl Pts',(-5.86046639555703,0.831048083761738,
7.52414842993556));
#15018=CARTESIAN_POINT('Ctrl Pts',(-5.83242967323381,0.995336460339776,
7.51630285672658));
#15019=CARTESIAN_POINT('Ctrl Pts',(-5.80438623858568,1.15966416950993,7.50845540519401));
#15020=CARTESIAN_POINT('Ctrl Pts',(-5.76939685314964,1.32278730643484,7.50060795366145));
#15021=CARTESIAN_POINT('Ctrl Pts',(-5.7275927811386,1.48411977142985,7.49276050212888));
#15022=CARTESIAN_POINT('Ctrl Pts',(-5.71678765814867,1.52581946819813,7.49073216673264));
#15023=CARTESIAN_POINT('Ctrl Pts',(-5.70552752957678,1.56739959843692,7.48870383133641));
#15024=CARTESIAN_POINT('Ctrl Pts',(-5.69381521029775,1.60885018366597,7.48667549594017));
#15025=CARTESIAN_POINT('Ctrl Pts',(-5.64884469790125,1.76800346599001,7.47888751817866));
#15026=CARTESIAN_POINT('Ctrl Pts',(-5.59718899536415,1.92529850569285,7.47109954041715));
#15027=CARTESIAN_POINT('Ctrl Pts',(-5.53902680273251,2.08017130090548,7.46331156265564));
#15028=CARTESIAN_POINT('Ctrl Pts',(-5.4808760452867,2.23501364679852,7.45552511607734));
#15029=CARTESIAN_POINT('Ctrl Pts',(-5.41622146246665,2.38743439946199,7.44773866949905));
#15030=CARTESIAN_POINT('Ctrl Pts',(-5.34529070695169,2.53688742767114,7.43995222292075));
#15031=CARTESIAN_POINT('Ctrl Pts',(-5.27435724558821,2.68634615717662,7.43216547930705));
#15032=CARTESIAN_POINT('Ctrl Pts',(-5.19714726587681,2.83283664531632,7.42437873569336));
#15033=CARTESIAN_POINT('Ctrl Pts',(-5.1139357172095,2.97583468000979,7.41659199207966));
#15034=CARTESIAN_POINT('Ctrl Pts',(-5.03072967236351,3.11882325645324,7.40880576350079));
#15035=CARTESIAN_POINT('Ctrl Pts',(-4.94152301376513,3.25831956555739,7.40101953492192));
#15036=CARTESIAN_POINT('Ctrl Pts',(-4.8466356883766,3.39382572720732,7.39323330634305));
#15037=CARTESIAN_POINT('Ctrl Pts',(-4.75172338424075,3.52936756036721,7.38544502806749));
#15038=CARTESIAN_POINT('Ctrl Pts',(-4.651127606973,3.66091688411636,7.37765674979194));
#15039=CARTESIAN_POINT('Ctrl Pts',(-4.54521103882801,3.78800569891546,7.36986847151638));
#15040=CARTESIAN_POINT('Ctrl Pts',(-4.4445160549568,3.90882915817717,7.36246414782013));
#15041=CARTESIAN_POINT('Ctrl Pts',(-4.33901243121526,4.02562110951189,7.35505982412388));
#15042=CARTESIAN_POINT('Ctrl Pts',(-4.2290449596083,4.13800788932448,7.34765550042763));
#15043=CARTESIAN_POINT('Ctrl Pts',(-4.11337953782229,4.25621797545483,7.3398675226661));
#15044=CARTESIAN_POINT('Ctrl Pts',(-3.99273402351709,4.36959654925919,7.33207954490457));
#15045=CARTESIAN_POINT('Ctrl Pts',(-3.86753528394729,4.47773395702812,7.32429156714304));
#15046=CARTESIAN_POINT('Ctrl Pts',(-3.74236115952358,4.58585010405514,7.31650512056474));
#15047=CARTESIAN_POINT('Ctrl Pts',(-3.6126358377128,4.68872693236575,7.30871867398644));
#15048=CARTESIAN_POINT('Ctrl Pts',(-3.47882061190941,4.78599391063698,7.30093222740814));
#15049=CARTESIAN_POINT('Ctrl Pts',(-3.34500028135622,4.88326459942459,7.29314548379442));
#15050=CARTESIAN_POINT('Ctrl Pts',(-3.20708999075695,4.97492481887361,7.2853587401807));
#15051=CARTESIAN_POINT('Ctrl Pts',(-3.06558206786894,5.06064592198075,7.27757199656698));
#15052=CARTESIAN_POINT('Ctrl Pts',(-2.92408350467152,5.14636135527814,7.26978576798811));
#15053=CARTESIAN_POINT('Ctrl Pts',(-2.77898805876728,5.22613829285959,7.26199953940923));
#15054=CARTESIAN_POINT('Ctrl Pts',(-2.63081496136454,5.29969274595806,7.25421331083036));
#15055=CARTESIAN_POINT('Ctrl Pts',(-2.48260285792614,5.3732665620021,7.24642503255478));
#15056=CARTESIAN_POINT('Ctrl Pts',(-2.33131176962279,5.44061447646983,7.2386367542792));
#15057=CARTESIAN_POINT('Ctrl Pts',(-2.17748414623837,5.50149919161864,7.23084847600361));
#15058=CARTESIAN_POINT('Ctrl Pts',(-2.03124007577153,5.55938234925103,7.22344415230745));
#15059=CARTESIAN_POINT('Ctrl Pts',(-1.88270378816617,5.61142411885008,7.21603982861129));
#15060=CARTESIAN_POINT('Ctrl Pts',(-1.73235687009803,5.65746146580992,7.20863550491513));
#15061=CARTESIAN_POINT('Ctrl Pts',(-1.57421974610455,5.7058842318903,7.20084752715361));
#15062=CARTESIAN_POINT('Ctrl Pts',(-1.41402280613875,5.7476811402137,7.1930595493921));
#15063=CARTESIAN_POINT('Ctrl Pts',(-1.25233692593782,5.78269684372548,7.18527157163058));
#15064=CARTESIAN_POINT('Ctrl Pts',(-1.09068283456665,5.81770566284985,7.17748512505223));
#15065=CARTESIAN_POINT('Ctrl Pts',(-0.927540699178164,5.84593586978058,
7.16969867847388));
#15066=CARTESIAN_POINT('Ctrl Pts',(-0.76349289492658,5.86728294544388,7.16191223189554));
#15067=CARTESIAN_POINT('Ctrl Pts',(-0.59943883262148,5.88863083544994,7.15412548828183));
#15068=CARTESIAN_POINT('Ctrl Pts',(-0.434479348676863,5.90309502361526,
7.14633874466812));
#15069=CARTESIAN_POINT('Ctrl Pts',(-0.269204017649051,5.91062262028135,
7.13855200105441));
#15070=CARTESIAN_POINT('Ctrl Pts',(-0.103939618347989,5.91814971905324,
7.13076577247554));
#15071=CARTESIAN_POINT('Ctrl Pts',(0.0616402669794469,5.91874113003358,
7.12297954389666));
#15072=CARTESIAN_POINT('Ctrl Pts',(0.226943819083687,5.91239605113525,7.11519331531779));
#15073=CARTESIAN_POINT('Ctrl Pts',(0.392290886754298,5.90604930191769,7.10740503704221));
#15074=CARTESIAN_POINT('Ctrl Pts',(0.557361156241647,5.89276242438704,7.09961675876663));
#15075=CARTESIAN_POINT('Ctrl Pts',(0.721564771939402,5.8725867249787,7.09182848049105));
#15076=CARTESIAN_POINT('Ctrl Pts',(0.87767330834284,5.85340566801983,7.08442415679491));
#15077=CARTESIAN_POINT('Ctrl Pts',(1.03299832143993,5.82799868423886,7.07701983309876));
#15078=CARTESIAN_POINT('Ctrl Pts',(1.1870389405482,5.796453149653,7.06961550940262));
#15079=CARTESIAN_POINT('Ctrl Pts',(1.34906115421956,5.76327308731208,7.06182753164108));
#15080=CARTESIAN_POINT('Ctrl Pts',(1.50972029718412,5.72328957943936,7.05403955387955));
#15081=CARTESIAN_POINT('Ctrl Pts',(1.66844078306887,5.67663949145025,7.04625157611801));
#15082=CARTESIAN_POINT('Ctrl Pts',(1.8271300631457,5.62999857526827,7.03846512953965));
#15083=CARTESIAN_POINT('Ctrl Pts',(1.98388114026828,5.57669378426923,7.0306786829613));
#15084=CARTESIAN_POINT('Ctrl Pts',(2.13813266131111,5.5169121150454,7.02289223638294));
#15085=CARTESIAN_POINT('Ctrl Pts',(2.29239006670133,5.45712816528581,7.01510549276922));
#15086=CARTESIAN_POINT('Ctrl Pts',(2.44414742583559,5.390866954678,7.0073187491555));
#15087=CARTESIAN_POINT('Ctrl Pts',(2.59286177785379,5.31836425637102,6.99953200554178));
#15088=CARTESIAN_POINT('Ctrl Pts',(2.74156629353028,5.24586635357508,6.99174577696289));
#15089=CARTESIAN_POINT('Ctrl Pts',(2.88722791765946,5.16712792935809,6.98395954838401));
#15090=CARTESIAN_POINT('Ctrl Pts',(3.02932665116721,5.082431564028,6.97617331980512));
#15091=CARTESIAN_POINT('Ctrl Pts',(3.17146279165612,4.99771290268396,6.96838504152952));
#15092=CARTESIAN_POINT('Ctrl Pts',(3.3100338916907,4.90703332825587,6.96059676325393));
#15093=CARTESIAN_POINT('Ctrl Pts',(3.44454661891554,4.81072023221238,6.95280848497833));
#15094=CARTESIAN_POINT('Ctrl Pts',(3.57242799890372,4.7191552785676,6.94540416128225));
#15095=CARTESIAN_POINT('Ctrl Pts',(3.69664130054661,4.62249903090095,6.93799983758617));
#15096=CARTESIAN_POINT('Ctrl Pts',(3.8167885852575,4.52106795546673,6.93059551389009));
#15097=CARTESIAN_POINT('Ctrl Pts',(3.94316128583654,4.414381242104,6.92280753612858));
#15098=CARTESIAN_POINT('Ctrl Pts',(4.06508062823147,4.30237358580423,6.91501955836706));
#15099=CARTESIAN_POINT('Ctrl Pts',(4.18210676270983,4.1854406682925,6.90723158060554));
#15100=CARTESIAN_POINT('Ctrl Pts',(4.29910988884662,4.06853074079507,6.89944513402724));
#15101=CARTESIAN_POINT('Ctrl Pts',(4.41122150072586,3.94669770995357,6.89165868744893));
#15102=CARTESIAN_POINT('Ctrl Pts',(4.5180382415108,3.82037445949294,6.88387224087063));
#15103=CARTESIAN_POINT('Ctrl Pts',(4.62485905711387,3.69404639008477,6.87608549725692));
#15104=CARTESIAN_POINT('Ctrl Pts',(4.72638438810034,3.56322799974676,6.86829875364321));
#15105=CARTESIAN_POINT('Ctrl Pts',(4.82225037371936,3.42838619406617,6.8605120100295));
#15106=CARTESIAN_POINT('Ctrl Pts',(4.91811001852061,3.29355330716227,6.85272578145063));
#15107=CARTESIAN_POINT('Ctrl Pts',(5.00831088194913,3.15469779798549,6.84493955287175));
#15108=CARTESIAN_POINT('Ctrl Pts',(5.09253166867592,3.01231667758104,6.83715332429288));
#15109=CARTESIAN_POINT('Ctrl Pts',(5.17677462622219,2.86989807585825,6.82936504601731));
#15110=CARTESIAN_POINT('Ctrl Pts',(5.25503419693593,2.72395228258291,6.82157676774175));
#15111=CARTESIAN_POINT('Ctrl Pts',(5.32703394840831,2.57500288834894,6.81378848946618));
#15112=CARTESIAN_POINT('Ctrl Pts',(5.39548418183408,2.43339655505688,6.80638416576998));
#15113=CARTESIAN_POINT('Ctrl Pts',(5.45827681976575,2.28907587344672,6.79897984207378));
#15114=CARTESIAN_POINT('Ctrl Pts',(5.51521395563209,2.14250917993389,6.79157551837758));
#15115=CARTESIAN_POINT('Ctrl Pts',(5.57510128175738,1.98834815233828,6.78378754061606));
#15116=CARTESIAN_POINT('Ctrl Pts',(5.62853161412413,1.83164703331563,6.77599956285455));
#15117=CARTESIAN_POINT('Ctrl Pts',(5.67530816618571,1.67296377167165,6.76821158509303));
#15118=CARTESIAN_POINT('Ctrl Pts',(5.72207552157626,1.51431170851687,6.76042513851469));
#15119=CARTESIAN_POINT('Ctrl Pts',(5.76219161658887,1.35367858664164,6.75263869193635));
#15120=CARTESIAN_POINT('Ctrl Pts',(5.79550951268791,1.19163755011494,6.74485224535801));
#15121=CARTESIAN_POINT('Ctrl Pts',(5.82882867978955,1.02959033208814,6.73706550174429));
#15122=CARTESIAN_POINT('Ctrl Pts',(5.85534906081321,0.866135404132536,6.72927875813057));
#15123=CARTESIAN_POINT('Ctrl Pts',(5.87497467979639,0.701856875902259,6.72149201451685));
#15124=CARTESIAN_POINT('Ctrl Pts',(5.89459900069162,0.537589213468304,6.713705785938));
#15125=CARTESIAN_POINT('Ctrl Pts',(5.90732943434829,0.372498377106149,6.70591955735915));
#15126=CARTESIAN_POINT('Ctrl Pts',(5.91312178758799,0.207174534275467,6.6981333287803));
#15127=CARTESIAN_POINT('Ctrl Pts',(5.91891566564388,0.041807170536806,6.69034505050474));
#15128=CARTESIAN_POINT('Ctrl Pts',(5.91776780055012,-0.123793002738391,
6.68255677222917));
#15129=CARTESIAN_POINT('Ctrl Pts',(5.90968611136997,-0.289033955757698,
6.67476849395361));
#15130=CARTESIAN_POINT('Ctrl Pts',(5.90200284164276,-0.446128689757979,
6.66736417025743));
#15131=CARTESIAN_POINT('Ctrl Pts',(5.8880529538693,-0.602898505570204,6.65995984656125));
#15132=CARTESIAN_POINT('Ctrl Pts',(5.86788686414186,-0.75883747412171,6.65255552286507));
#15133=CARTESIAN_POINT('Ctrl Pts',(5.84667587110872,-0.922856399964292,
6.64476754510352));
#15134=CARTESIAN_POINT('Ctrl Pts',(5.81857980235061,-1.08601476487503,6.63697956734197));
#15135=CARTESIAN_POINT('Ctrl Pts',(5.78369295186044,-1.24772849654879,6.62919158958042));
#15136=CARTESIAN_POINT('Ctrl Pts',(5.74881296042417,-1.40941043391649,6.62140514300207));
#15137=CARTESIAN_POINT('Ctrl Pts',(5.70714491857074,-1.56964799259304,6.61361869642372));
#15138=CARTESIAN_POINT('Ctrl Pts',(5.65883416014089,-1.72786761950172,6.60583224984536));
#15139=CARTESIAN_POINT('Ctrl Pts',(5.61052155876456,-1.88609328213233,6.59804550623163));
#15140=CARTESIAN_POINT('Ctrl Pts',(5.55556582327765,-2.04230055219289,6.5902587626179));
#15141=CARTESIAN_POINT('Ctrl Pts',(5.49416228134141,-2.19593064298156,6.58247201900417));
#15142=CARTESIAN_POINT('Ctrl Pts',(5.43276280078999,-2.3495505722893,6.57468579042527));
#15143=CARTESIAN_POINT('Ctrl Pts',(5.36491648594019,-2.50059336673357,6.56689956184636));
#15144=CARTESIAN_POINT('Ctrl Pts',(5.29086702922229,-2.6485197076081,6.55911333326745));
#15145=CARTESIAN_POINT('Ctrl Pts',(5.21679807925105,-2.79648498956021,6.55132505499186));
#15146=CARTESIAN_POINT('Ctrl Pts',(5.13652286581074,-2.94133189180655,6.54353677671626));
#15147=CARTESIAN_POINT('Ctrl Pts',(5.05033172712747,-3.08254440494694,6.53574849844067));
#15148=CARTESIAN_POINT('Ctrl Pts',(4.96838972814401,-3.21679527789017,6.52834417474462));
#15149=CARTESIAN_POINT('Ctrl Pts',(4.88110118910696,-3.34776124854887,6.52093985104858));
#15150=CARTESIAN_POINT('Ctrl Pts',(4.78875254687753,-3.47502224557973,6.51353552735253));
#15151=CARTESIAN_POINT('Ctrl Pts',(4.6916188718097,-3.60887725455423,6.50574754959102));
#15152=CARTESIAN_POINT('Ctrl Pts',(4.58885204778303,-3.7386810333868,6.49795957182951));
#15153=CARTESIAN_POINT('Ctrl Pts',(4.48081444090749,-3.86396590417862,6.490171594068));
#15154=CARTESIAN_POINT('Ctrl Pts',(4.37279807515156,-3.9892261428909,6.48238514748967));
#15155=CARTESIAN_POINT('Ctrl Pts',(4.25951320278849,-4.1099690044439,6.47459870091135));
#15156=CARTESIAN_POINT('Ctrl Pts',(4.14136196751739,-4.22576047789039,6.46681225433302));
#15157=CARTESIAN_POINT('Ctrl Pts',(4.023206225043,-4.3415563685206,6.45902551071931));
#15158=CARTESIAN_POINT('Ctrl Pts',(3.90018397363803,-4.45240026660171,6.4512387671056));
#15159=CARTESIAN_POINT('Ctrl Pts',(3.77273418321245,-4.55789505641807,6.44345202349189));
#15160=CARTESIAN_POINT('Ctrl Pts',(3.64529282263673,-4.66338286854356,6.435665794913));
#15161=CARTESIAN_POINT('Ctrl Pts',(3.5134247553285,-4.76352207673162,6.42787956633411));
#15162=CARTESIAN_POINT('Ctrl Pts',(3.37760209659498,-4.85795580873038,6.42009333775521));
#15163=CARTESIAN_POINT('Ctrl Pts',(3.24174368303502,-4.95241440006946,6.41230505947965));
#15164=CARTESIAN_POINT('Ctrl Pts',(3.1019288592739,-5.04116432987048,6.40451678120409));
#15165=CARTESIAN_POINT('Ctrl Pts',(2.95865953805417,-5.1238915191855,6.39672850292853));
#15166=CARTESIAN_POINT('Ctrl Pts',(2.82245325567606,-5.20254033815288,6.38932417923236));
#15167=CARTESIAN_POINT('Ctrl Pts',(2.68312510603525,-5.27574581087367,6.3819198555362));
#15168=CARTESIAN_POINT('Ctrl Pts',(2.54112765407703,-5.34327622420786,6.37451553184003));
#15169=CARTESIAN_POINT('Ctrl Pts',(2.39177262268947,-5.41430571708996,6.3667275540785));
#15170=CARTESIAN_POINT('Ctrl Pts',(2.23941089857263,-5.47908184034542,6.35893957631697));
#15171=CARTESIAN_POINT('Ctrl Pts',(2.08458449997768,-5.53736742730269,6.35115159855545));
#15172=CARTESIAN_POINT('Ctrl Pts',(1.92978854157962,-5.59564155481403,6.34336515197709));
#15173=CARTESIAN_POINT('Ctrl Pts',(1.77252917445244,-5.64742757969805,6.33557870539874));
#15174=CARTESIAN_POINT('Ctrl Pts',(1.61336722615573,-5.69253693497605,6.32779225882038));
#15175=CARTESIAN_POINT('Ctrl Pts',(1.45419920619022,-5.73764801107407,6.32000551520668));
#15176=CARTESIAN_POINT('Ctrl Pts',(1.29312876617486,-5.77608181697151,6.31221877159298));
#15177=CARTESIAN_POINT('Ctrl Pts',(1.13073140640612,-5.80769980707223,6.30443202797927));
#15178=CARTESIAN_POINT('Ctrl Pts',(0.968344788007374,-5.83931570587953,
6.29664579940038));
#15179=CARTESIAN_POINT('Ctrl Pts',(0.804631739196146,-5.86411663007676,
6.2888595708215));
#15180=CARTESIAN_POINT('Ctrl Pts',(0.640177598575581,-5.88201523330074,
6.28107334224261));
#15181=CARTESIAN_POINT('Ctrl Pts',(0.475680165993559,-5.8999185482677,6.27328506396704));
#15182=CARTESIAN_POINT('Ctrl Pts',(0.310441569445996,-5.91091587494821,
6.26549678569146));
#15183=CARTESIAN_POINT('Ctrl Pts',(0.145052825819117,-5.91497170240246,
6.25770850741588));
#15184=CARTESIAN_POINT('Ctrl Pts',(-0.0121824128534097,-5.91882758148951,
6.25030418371976));
#15185=CARTESIAN_POINT('Ctrl Pts',(-0.169553087598295,-5.91640988658437,
6.24289986002364));
#15186=CARTESIAN_POINT('Ctrl Pts',(-0.32655093453622,-5.90773180244783,
6.23549553632751));
#15187=CARTESIAN_POINT('Ctrl Pts',(-0.49168360441094,-5.89860406451503,
6.22770755856601));
#15188=CARTESIAN_POINT('Ctrl Pts',(-0.656462855812958,-5.88254668530447,
6.2199195808045));
#15189=CARTESIAN_POINT('Ctrl Pts',(-0.820299274759474,-5.85961087977086,
6.21213160304299));
#15190=CARTESIAN_POINT('Ctrl Pts',(-0.984103482061949,-5.83667958361319,
6.20434515646465));
#15191=CARTESIAN_POINT('Ctrl Pts',(-1.14696491050467,-5.80687260375928,
6.19655870988631));
#15192=CARTESIAN_POINT('Ctrl Pts',(-1.30830089468569,-5.77029282891819,
6.18877226330797));
#15193=CARTESIAN_POINT('Ctrl Pts',(-1.46964303347078,-5.73371165864114,
6.18098551969425));
#15194=CARTESIAN_POINT('Ctrl Pts',(-1.62945929904668,-5.69035724317976,
6.17319877608053));
#15195=CARTESIAN_POINT('Ctrl Pts',(-1.78717808700344,-5.64038341319406,
6.16541203246681));
#15196=CARTESIAN_POINT('Ctrl Pts',(-1.94488644304213,-5.59041288860342,
6.15762580388793));
#15197=CARTESIAN_POINT('Ctrl Pts',(-2.10049729447075,-5.53382392227884,
6.14983957530906));
#15198=CARTESIAN_POINT('Ctrl Pts',(-2.2534549062819,-5.47082000689604,6.14205334673018));
#15199=CARTESIAN_POINT('Ctrl Pts',(-2.40645278363498,-5.40779950595881,
6.1342650684546));
#15200=CARTESIAN_POINT('Ctrl Pts',(-2.55679572930045,-5.33836080153691,
6.12647679017901));
#15201=CARTESIAN_POINT('Ctrl Pts',(-2.70394783468263,-5.26275561562715,
6.11868851190343));
#15202=CARTESIAN_POINT('Ctrl Pts',(-2.84384548372208,-5.19087769219211,
6.11128418820728));
#15203=CARTESIAN_POINT('Ctrl Pts',(-2.98085909025334,-5.11342676486538,
6.10387986451114));
#15204=CARTESIAN_POINT('Ctrl Pts',(-3.11454871155952,-5.03065769913069,
6.09647554081499));
#15205=CARTESIAN_POINT('Ctrl Pts',(-3.25516544313584,-4.94359996506336,
6.08868756305342));
#15206=CARTESIAN_POINT('Ctrl Pts',(-3.39215488172444,-4.85062720111968,
6.08089958529185));
#15207=CARTESIAN_POINT('Ctrl Pts',(-3.52502403892494,-4.75206650705788,
6.07311160753028));
#15208=CARTESIAN_POINT('Ctrl Pts',(-3.65786707291078,-4.65352519087295,
6.06532516095187));
#15209=CARTESIAN_POINT('Ctrl Pts',(-3.78659118537121,-4.54939832693168,
6.05753871437345));
#15210=CARTESIAN_POINT('Ctrl Pts',(-3.91073404767302,-4.44005515403481,
6.04975226779503));
#15211=CARTESIAN_POINT('Ctrl Pts',(-4.03488164574422,-4.33070780994321,
6.04196552418129));
#15212=CARTESIAN_POINT('Ctrl Pts',(-4.15444740154787,-4.2161439669478,6.03417878056755));
#15213=CARTESIAN_POINT('Ctrl Pts',(-4.26900308220881,-4.09677229616093,
6.02639203695381));
#15214=CARTESIAN_POINT('Ctrl Pts',(-4.38355118586876,-3.97740852091676,
6.01860580837488));
#15215=CARTESIAN_POINT('Ctrl Pts',(-4.49308965633097,-3.85323778490719,
6.01081957979596));
#15216=CARTESIAN_POINT('Ctrl Pts',(-4.59722796558208,-3.7247047661486,6.00303335121704));
#15217=CARTESIAN_POINT('Ctrl Pts',(-4.70139368886861,-3.59613791153502,
5.99524507294144));
#15218=CARTESIAN_POINT('Ctrl Pts',(-4.80015620752505,-3.4632067267366,5.98745679466584));
#15219=CARTESIAN_POINT('Ctrl Pts',(-4.89316548685527,-3.32638874468219,
5.97966851639024));
#15220=CARTESIAN_POINT('Ctrl Pts',(-4.98158949875062,-3.19631575669867,
5.97226419269431));
#15221=CARTESIAN_POINT('Ctrl Pts',(-5.06481371698075,-3.06273018855232,
5.96485986899839));
#15222=CARTESIAN_POINT('Ctrl Pts',(-5.14257386922539,-2.92606639741141,
5.95745554530246));
#15223=CARTESIAN_POINT('Ctrl Pts',(-5.22436315360635,-2.78232138977514,
5.94966756754093));
#15224=CARTESIAN_POINT('Ctrl Pts',(-5.30013635645,-2.63511927412894,5.9418795897794));
#15225=CARTESIAN_POINT('Ctrl Pts',(-5.36961720770652,-2.48498322030593,
5.93409161201786));
#15226=CARTESIAN_POINT('Ctrl Pts',(-5.43908439843228,-2.33487668451767,
5.9263051654395));
#15227=CARTESIAN_POINT('Ctrl Pts',(-5.50226157188416,-2.18183765133573,
5.91851871886113));
#15228=CARTESIAN_POINT('Ctrl Pts',(-5.55891954775881,-2.02641161269004,
5.91073227228276));
#15229=CARTESIAN_POINT('Ctrl Pts',(-5.61557968500736,-1.87097964489175,
5.90294552866902));
#15230=CARTESIAN_POINT('Ctrl Pts',(-5.66572001388714,-1.71316078827903,
5.89515878505529));
#15231=CARTESIAN_POINT('Ctrl Pts',(-5.70916016500507,-1.55351883568219,
5.88737204144156));
#15232=CARTESIAN_POINT('Ctrl Pts',(-5.75259744288209,-1.39388744220579,
5.87958581286264));
#15233=CARTESIAN_POINT('Ctrl Pts',(-5.78933534604039,-1.23243350244636,
5.87179958428373));
#15234=CARTESIAN_POINT('Ctrl Pts',(-5.81924384514638,-1.06973437507913,
5.86401335570481));
#15235=CARTESIAN_POINT('Ctrl Pts',(-5.84916021755721,-0.906992417751686,
5.85622507742922));
#15236=CARTESIAN_POINT('Ctrl Pts',(-5.87224353376436,-0.743004931960494,
5.84843679915363));
#15237=CARTESIAN_POINT('Ctrl Pts',(-5.88841504399207,-0.578358740046192,
5.84064852087803));
#15238=CARTESIAN_POINT('Ctrl Pts',(-5.90378931442035,-0.421829446007969,
5.83324419718201));
#15239=CARTESIAN_POINT('Ctrl Pts',(-5.91291682763475,-0.264705090734196,
5.82583987348598));
#15240=CARTESIAN_POINT('Ctrl Pts',(-5.91577346608668,-0.107493536758192,
5.81843554978995));
#15241=CARTESIAN_POINT('Ctrl Pts',(-5.91642423954695,-0.0716790265576193,
5.81674876392827));
#15242=CARTESIAN_POINT('Ctrl Pts',(-5.91674977158135,-0.0358585978170884,
5.81506197806659));
#15243=CARTESIAN_POINT('Ctrl Pts',(-5.91674999987983,-3.77094237526255E-5,
5.8133751922049));
#15244=CARTESIAN_POINT('Ctrl Pts',(-5.91674999993288,2.81822668001089E-5,
5.56162480783485));
#15245=CARTESIAN_POINT('Ctrl Pts',(-5.91675078674804,-0.165160396169148,
5.56940348493561));
#15246=CARTESIAN_POINT('Ctrl Pts',(-5.90982942903261,-0.330379709080826,
5.57718216203637));
#15247=CARTESIAN_POINT('Ctrl Pts',(-5.89600425644402,-0.495039766578426,
5.58496083913712));
#15248=CARTESIAN_POINT('Ctrl Pts',(-5.88218183123642,-0.659667102320903,
5.59273797043515));
#15249=CARTESIAN_POINT('Ctrl Pts',(-5.86145835535694,-0.823735084627806,
5.60051510173317));
#15250=CARTESIAN_POINT('Ctrl Pts',(-5.83390412672512,-0.986657591406252,
5.60829223303119));
#15251=CARTESIAN_POINT('Ctrl Pts',(-5.80634900165882,-1.14958539861808,
5.61606961734623));
#15252=CARTESIAN_POINT('Ctrl Pts',(-5.77196272892421,-1.31136733851814,
5.62384700166127));
#15253=CARTESIAN_POINT('Ctrl Pts',(-5.73086707782368,-1.47142553288187,
5.6316243859763));
#15254=CARTESIAN_POINT('Ctrl Pts',(-5.68977377739136,-1.63147457192868,
5.63940132542553));
#15255=CARTESIAN_POINT('Ctrl Pts',(-5.64197194692404,-1.78979975185782,
5.64717826487476));
#15256=CARTESIAN_POINT('Ctrl Pts',(-5.58763381326402,-1.9458363064165,5.65495520432399));
#15257=CARTESIAN_POINT('Ctrl Pts',(-5.53328198897035,-2.10191217478963,
5.66273410319327));
#15258=CARTESIAN_POINT('Ctrl Pts',(-5.47239067544521,-2.2556979618502,5.67051300206256));
#15259=CARTESIAN_POINT('Ctrl Pts',(-5.40518132146314,-2.40664609874531,
5.67829190093184));
#15260=CARTESIAN_POINT('Ctrl Pts',(-5.35187308520774,-2.52637316748137,
5.68446186618461));
#15261=CARTESIAN_POINT('Ctrl Pts',(-5.29459106575013,-2.64431532354144,
5.69063183143738));
#15262=CARTESIAN_POINT('Ctrl Pts',(-5.23346695418843,-2.76020908663051,
5.69680179669016));
#15263=CARTESIAN_POINT('Ctrl Pts',(-5.15631232362956,-2.90649735564182,
5.70458990808312));
#15264=CARTESIAN_POINT('Ctrl Pts',(-5.0730064015835,-3.04957472254615,5.71237801947609));
#15265=CARTESIAN_POINT('Ctrl Pts',(-4.9838415312255,-3.18892680288086,5.72016613086906));
#15266=CARTESIAN_POINT('Ctrl Pts',(-4.89469416683538,-3.32825152386391,
5.72795271320213));
#15267=CARTESIAN_POINT('Ctrl Pts',(-4.79969032143716,-3.46385214864654,
5.73573929553519));
#15268=CARTESIAN_POINT('Ctrl Pts',(-4.69916649070406,-3.5952419744913,5.74352587786826));
#15269=CARTESIAN_POINT('Ctrl Pts',(-4.59863882701976,-3.72663681020075,
5.75131275710197));
#15270=CARTESIAN_POINT('Ctrl Pts',(-4.49259094785246,-3.85382026953491,
5.75909963633568));
#15271=CARTESIAN_POINT('Ctrl Pts',(-4.38140103783249,-3.97633694600701,
5.76688651556939));
#15272=CARTESIAN_POINT('Ctrl Pts',(-4.27021846628216,-4.09884553644945,
5.77467288087358));
#15273=CARTESIAN_POINT('Ctrl Pts',(-4.15389475785512,-4.21668772384252,
5.78245924617778));
#15274=CARTESIAN_POINT('Ctrl Pts',(-4.03284661808541,-4.32944323412342,
5.79024561148197));
#15275=CARTESIAN_POINT('Ctrl Pts',(-3.91176669353232,-4.4422283517116,5.79803402132757));
#15276=CARTESIAN_POINT('Ctrl Pts',(-3.78596009141773,-4.54992390391047,
5.80582243117318));
#15277=CARTESIAN_POINT('Ctrl Pts',(-3.6558790851148,-4.65214774889192,5.81361084101878));
#15278=CARTESIAN_POINT('Ctrl Pts',(-3.53263409049762,-4.74899953058208,
5.82098995467095));
#15279=CARTESIAN_POINT('Ctrl Pts',(-3.40555259771247,-4.84093975041548,
5.82836906832312));
#15280=CARTESIAN_POINT('Ctrl Pts',(-3.2750454318935,-4.92767774733023,5.83574818197529));
#15281=CARTESIAN_POINT('Ctrl Pts',(-3.13730472306474,-5.0192233195787,5.84353629336825));
#15282=CARTESIAN_POINT('Ctrl Pts',(-2.99569863356498,-5.10500633062844,
5.85132440476121));
#15283=CARTESIAN_POINT('Ctrl Pts',(-2.85072997627565,-5.18471495502534,
5.85911251615417));
#15284=CARTESIAN_POINT('Ctrl Pts',(-2.70578978105447,-5.26440793002367,
5.86689909848725));
#15285=CARTESIAN_POINT('Ctrl Pts',(-2.55748861512491,-5.33802874410464,
5.87468568082034));
#15286=CARTESIAN_POINT('Ctrl Pts',(-2.40635481877118,-5.40531100388097,
5.88247226315342));
#15287=CARTESIAN_POINT('Ctrl Pts',(-2.25521525972003,-5.47259582911463,
5.89025914238712));
#15288=CARTESIAN_POINT('Ctrl Pts',(-2.10124314441283,-5.53354148287171,
5.89804602162083));
#15289=CARTESIAN_POINT('Ctrl Pts',(-1.94498844792873,-5.5879289991842,5.90583290085453));
#15290=CARTESIAN_POINT('Ctrl Pts',(-1.78874406416405,-5.64231292595214,
5.91361926615872));
#15291=CARTESIAN_POINT('Ctrl Pts',(-1.63021770252737,-5.6901394765073,5.92140563146291));
#15292=CARTESIAN_POINT('Ctrl Pts',(-1.46997635559212,-5.73123896522385,
5.92919199676709));
#15293=CARTESIAN_POINT('Ctrl Pts',(-1.30969293253327,-5.7723492458315,5.93698040661269));
#15294=CARTESIAN_POINT('Ctrl Pts',(-1.14769393357346,-5.80672885366815,
5.94476881645828));
#15295=CARTESIAN_POINT('Ctrl Pts',(-0.984559340411803,-5.83425860480215,
5.95255722630388));
#15296=CARTESIAN_POINT('Ctrl Pts',(-0.829997789670841,-5.86034161358844,
5.95993633995606));
#15297=CARTESIAN_POINT('Ctrl Pts',(-0.674417186707035,-5.88027615178174,
5.96731545360823));
#15298=CARTESIAN_POINT('Ctrl Pts',(-0.518317348950165,-5.89400353650024,
5.97469456726041));
#15299=CARTESIAN_POINT('Ctrl Pts',(-0.353565458387484,-5.90849178080178,
5.98248267865336));
#15300=CARTESIAN_POINT('Ctrl Pts',(-0.188176301311359,-5.91607045415487,
5.99027079004632));
#15301=CARTESIAN_POINT('Ctrl Pts',(-0.0227405974838046,-5.91670629892393,
5.99805890143928));
#15302=CARTESIAN_POINT('Ctrl Pts',(0.14266262592742,-5.91734201885594,6.00584548377234));
#15303=CARTESIAN_POINT('Ctrl Pts',(0.308112058526976,-5.91103762877306,
6.01363206610539));
#15304=CARTESIAN_POINT('Ctrl Pts',(0.473016300660618,-5.89781197918426,
6.02141864843845));
#15305=CARTESIAN_POINT('Ctrl Pts',(0.637926830556203,-5.8845858253044,6.02920552767216));
#15306=CARTESIAN_POINT('Ctrl Pts',(0.802291809580338,-5.86443790545047,
6.03699240690586));
#15307=CARTESIAN_POINT('Ctrl Pts',(0.965523531021385,-5.83743906807977,
6.04477928613957));
#15308=CARTESIAN_POINT('Ctrl Pts',(1.12874447926359,-5.81044201261666,6.05256565144376));
#15309=CARTESIAN_POINT('Ctrl Pts',(1.290832004347,-5.77659499673414,6.06035201674796));
#15310=CARTESIAN_POINT('Ctrl Pts',(1.45120703356333,-5.73602028485224,6.06813838205215));
#15311=CARTESIAN_POINT('Ctrl Pts',(1.61162417400521,-5.69543491887504,6.07592679189774));
#15312=CARTESIAN_POINT('Ctrl Pts',(1.77032760960406,-5.6481184034913,6.08371520174333));
#15313=CARTESIAN_POINT('Ctrl Pts',(1.92675102339513,-5.59424356426727,6.09150361158892));
#15314=CARTESIAN_POINT('Ctrl Pts',(2.07495408038808,-5.54319995337493,6.09888272524113));
#15315=CARTESIAN_POINT('Ctrl Pts',(2.2211103452496,-5.48626967958779,6.10626183889333));
#15316=CARTESIAN_POINT('Ctrl Pts',(2.36475284092546,-5.42364034241163,6.11364095254553));
#15317=CARTESIAN_POINT('Ctrl Pts',(2.51635692372114,-5.3575396862373,6.1214290639385));
#15318=CARTESIAN_POINT('Ctrl Pts',(2.66521482238985,-5.28506668731938,6.12921717533147));
#15319=CARTESIAN_POINT('Ctrl Pts',(2.81079190079884,-5.20647476253402,6.13700528672444));
#15320=CARTESIAN_POINT('Ctrl Pts',(2.95634039768654,-5.12789826790288,6.14479186905751));
#15321=CARTESIAN_POINT('Ctrl Pts',(3.09860907855198,-5.04320539614401,6.15257845139059));
#15322=CARTESIAN_POINT('Ctrl Pts',(3.23708764060745,-4.95269564676919,6.16036503372366));
#15323=CARTESIAN_POINT('Ctrl Pts',(3.37557148281972,-4.86218244627774,6.16815191295739));
#15324=CARTESIAN_POINT('Ctrl Pts',(3.51026464742944,-4.7658520958598,6.17593879219112));
#15325=CARTESIAN_POINT('Ctrl Pts',(3.64068495215819,-4.66404798877852,6.18372567142485));
#15326=CARTESIAN_POINT('Ctrl Pts',(3.77109664922213,-4.56225060070952,6.19151203672905));
#15327=CARTESIAN_POINT('Ctrl Pts',(3.89723579891847,-4.45498037564351,6.19929840203324));
#15328=CARTESIAN_POINT('Ctrl Pts',(4.01865239989385,-4.3426217255625,6.20708476733744));
#15329=CARTESIAN_POINT('Ctrl Pts',(4.14010088240309,-4.23023357238159,6.21487317718305));
#15330=CARTESIAN_POINT('Ctrl Pts',(4.25682410233023,-4.11275454008674,6.22266158702866));
#15331=CARTESIAN_POINT('Ctrl Pts',(4.36840744966687,-3.99060733675904,6.23044999687427));
#15332=CARTESIAN_POINT('Ctrl Pts',(4.47412687352927,-3.87487920823059,6.2378291105264));
#15333=CARTESIAN_POINT('Ctrl Pts',(4.5752325753855,-3.75496112417559,6.24520822417853));
#15334=CARTESIAN_POINT('Ctrl Pts',(4.67140424624382,-3.63124123829239,6.25258733783066));
#15335=CARTESIAN_POINT('Ctrl Pts',(4.77290636706753,-3.50066400392456,6.26037544922361));
#15336=CARTESIAN_POINT('Ctrl Pts',(4.8689482474425,-3.36580494126235,6.26816356061656));
#15337=CARTESIAN_POINT('Ctrl Pts',(4.95918165474667,-3.22714237022851,6.27595167200951));
#15338=CARTESIAN_POINT('Ctrl Pts',(5.04939734629465,-3.08850702317273,6.28373825434258));
#15339=CARTESIAN_POINT('Ctrl Pts',(5.13380666602261,-2.94606992538918,6.29152483667566));
#15340=CARTESIAN_POINT('Ctrl Pts',(5.21210479653212,-2.80033822108454,6.29931141900873));
#15341=CARTESIAN_POINT('Ctrl Pts',(5.29040591253172,-2.65460096006279,6.30709829824243));
#15342=CARTESIAN_POINT('Ctrl Pts',(5.36259521834144,-2.50556912074392,6.31488517747614));
#15343=CARTESIAN_POINT('Ctrl Pts',(5.42841359014247,-2.35377493759632,6.32267205670985));
#15344=CARTESIAN_POINT('Ctrl Pts',(5.4942276179692,-2.2019907727766,6.33045842201405));
#15345=CARTESIAN_POINT('Ctrl Pts',(5.55367142621311,-2.0474449221907,6.33824478731825));
#15346=CARTESIAN_POINT('Ctrl Pts',(5.60653377466187,-1.89069024329097,6.34603115262245));
#15347=CARTESIAN_POINT('Ctrl Pts',(5.65941000368975,-1.73389440379613,6.35381956246805));
#15348=CARTESIAN_POINT('Ctrl Pts',(5.70570121569159,-1.57488887939405,6.36160797231364));
#15349=CARTESIAN_POINT('Ctrl Pts',(5.74524557060721,-1.41424322374839,6.36939638215924));
#15350=CARTESIAN_POINT('Ctrl Pts',(5.78271179221209,-1.26203981198143,6.37677549581142));
#15351=CARTESIAN_POINT('Ctrl Pts',(5.81412197673077,-1.10836447192937,6.3841546094636));
#15352=CARTESIAN_POINT('Ctrl Pts',(5.83938055994312,-0.953711297331862,
6.39153372311579));
#15353=CARTESIAN_POINT('Ctrl Pts',(5.86603913561472,-0.790486253266605,
6.39932183450875));
#15354=CARTESIAN_POINT('Ctrl Pts',(5.88585437186082,-0.626113609616027,
6.40710994590171));
#15355=CARTESIAN_POINT('Ctrl Pts',(5.89874932278544,-0.46117999678903,6.41489805729467));
#15356=CARTESIAN_POINT('Ctrl Pts',(5.91164174201125,-0.296278765801521,
6.42268463962773));
#15357=CARTESIAN_POINT('Ctrl Pts',(5.9176165619907,-0.130817103752322,6.4304712219608));
#15358=CARTESIAN_POINT('Ctrl Pts',(5.91664875128057,0.0346138190619499,
6.43825780429386));
#15359=CARTESIAN_POINT('Ctrl Pts',(5.91568090366804,0.200051049720641,6.44604468352758));
#15360=CARTESIAN_POINT('Ctrl Pts',(5.90776989358004,0.365457219265649,6.45383156276131));
#15361=CARTESIAN_POINT('Ctrl Pts',(5.89294281821464,0.530240986488662,6.46161844199503));
#15362=CARTESIAN_POINT('Ctrl Pts',(5.87811672142768,0.695013878077948,6.46940480729921));
#15363=CARTESIAN_POINT('Ctrl Pts',(5.85637550155739,0.859164131292016,6.47719117260338));
#15364=CARTESIAN_POINT('Ctrl Pts',(5.82779817025247,1.02210520461546,6.48497753790756));
#15365=CARTESIAN_POINT('Ctrl Pts',(5.79921333512064,1.18508906295607,6.49276594775315));
#15366=CARTESIAN_POINT('Ctrl Pts',(5.76378885504401,1.34686279169558,6.50055435759875));
#15367=CARTESIAN_POINT('Ctrl Pts',(5.72165510912876,1.50684882276914,6.50834276744434));
#15368=CARTESIAN_POINT('Ctrl Pts',(5.68173557409338,1.65842727452749,6.51572188109654));
#15369=CARTESIAN_POINT('Ctrl Pts',(5.63579387225719,1.80840083841147,6.52310099474873));
#15370=CARTESIAN_POINT('Ctrl Pts',(5.58398247836574,1.95628991813698,6.53048010840092));
#15371=CARTESIAN_POINT('Ctrl Pts',(5.52929936518024,2.11237595786933,6.53826821979388));
#15372=CARTESIAN_POINT('Ctrl Pts',(5.46805790732545,2.2661956360904,6.54605633118685));
#15373=CARTESIAN_POINT('Ctrl Pts',(5.40047120152811,2.41719700561737,6.55384444257982));
#15374=CARTESIAN_POINT('Ctrl Pts',(5.33289776520245,2.56816872865729,6.56163102491285));
#15375=CARTESIAN_POINT('Ctrl Pts',(5.25898169709123,2.71632295558537,6.56941760724589));
#15376=CARTESIAN_POINT('Ctrl Pts',(5.17898385322954,2.86112859034467,6.57720418957892));
#15377=CARTESIAN_POINT('Ctrl Pts',(5.0989829590676,3.00593974651109,6.58499106881264));
#15378=CARTESIAN_POINT('Ctrl Pts',(5.01289997617998,3.14740177343452,6.59277794804635));
#15379=CARTESIAN_POINT('Ctrl Pts',(4.92104161772181,3.28500836515677,6.60056482728006));
#15380=CARTESIAN_POINT('Ctrl Pts',(4.82918932186224,3.42260587492343,6.60835119258425));
#15381=CARTESIAN_POINT('Ctrl Pts',(4.73156259073039,3.55634819298406,6.61613755788843));
#15382=CARTESIAN_POINT('Ctrl Pts',(4.62851142840317,3.68575806580427,6.62392392319261));
#15383=CARTESIAN_POINT('Ctrl Pts',(4.52543320693327,3.81520191902929,6.63171233303821));
#15384=CARTESIAN_POINT('Ctrl Pts',(4.41692790578704,3.94031080249557,6.6395007428838));
#15385=CARTESIAN_POINT('Ctrl Pts',(4.30338634276314,4.06063991846356,6.6472891527294));
#15386=CARTESIAN_POINT('Ctrl Pts',(4.19581161128232,4.17464550368573,6.65466826638161));
#15387=CARTESIAN_POINT('Ctrl Pts',(4.08371651262214,4.28436058326985,6.66204738003382));
#15388=CARTESIAN_POINT('Ctrl Pts',(3.96746439411179,4.38943696206645,6.66942649368603));
#15389=CARTESIAN_POINT('Ctrl Pts',(3.84476883861533,4.50033734677521,6.67721460507902));
#15390=CARTESIAN_POINT('Ctrl Pts',(3.71739855822804,4.60610984434629,6.68500271647201));
#15391=CARTESIAN_POINT('Ctrl Pts',(3.58580474904591,4.70637173034811,6.69279082786499));
#15392=CARTESIAN_POINT('Ctrl Pts',(3.45423677601469,4.80661393167605,6.70057741019805));
#15393=CARTESIAN_POINT('Ctrl Pts',(3.31844718272779,4.90134748664351,6.7083639925311));
#15394=CARTESIAN_POINT('Ctrl Pts',(3.17891912790614,4.99023083040579,6.71615057486415));
#15395=CARTESIAN_POINT('Ctrl Pts',(3.03938575291036,5.07911756327047,6.72393745409788));
#15396=CARTESIAN_POINT('Ctrl Pts',(2.8961138985044,5.16215346357446,6.73172433333161));
#15397=CARTESIAN_POINT('Ctrl Pts',(2.74961513113557,5.23904067488795,6.73951121256533));
#15398=CARTESIAN_POINT('Ctrl Pts',(2.60312603260058,5.31592281168999,6.74729757786954));
#15399=CARTESIAN_POINT('Ctrl Pts',(2.45341073030344,5.38665692319201,6.75508394317375));
#15400=CARTESIAN_POINT('Ctrl Pts',(2.30100490573404,5.45099137646427,6.76287030847796));
#15401=CARTESIAN_POINT('Ctrl Pts',(2.14855906248999,5.51534272265753,6.77065871832358));
#15402=CARTESIAN_POINT('Ctrl Pts',(1.99342157910068,5.5732909266572,6.7784471281692));
#15403=CARTESIAN_POINT('Ctrl Pts',(1.83614844851996,5.62463238243156,6.78623553801482));
#15404=CARTESIAN_POINT('Ctrl Pts',(1.68714032902148,5.67327574413616,6.79361465166693));
#15405=CARTESIAN_POINT('Ctrl Pts',(1.53621550111517,5.71598881183929,6.80099376531905));
#15406=CARTESIAN_POINT('Ctrl Pts',(1.38385961722288,5.75263966560741,6.80837287897116));
#15407=CARTESIAN_POINT('Ctrl Pts',(1.22305919442603,5.79132194443522,6.81616099036413));
#15408=CARTESIAN_POINT('Ctrl Pts',(1.06060715103004,5.82326475527976,6.82394910175709));
#15409=CARTESIAN_POINT('Ctrl Pts',(0.897082801490368,5.84834788720457,6.83173721315005));
#15410=CARTESIAN_POINT('Ctrl Pts',(0.733590557106401,5.87342609449364,6.83952379548309));
#15411=CARTESIAN_POINT('Ctrl Pts',(0.56902674228538,5.89164726167009,6.84731037781613));
#15412=CARTESIAN_POINT('Ctrl Pts',(0.403979046395523,5.90294261301712,6.85509696014918));
#15413=CARTESIAN_POINT('Ctrl Pts',(0.238925057273242,5.91423839505341,6.86288383938289));
#15414=CARTESIAN_POINT('Ctrl Pts',(0.0733874686636907,5.9186078070816,6.87067071861661));
#15415=CARTESIAN_POINT('Ctrl Pts',(-0.0920419962389234,5.91603404599977,
6.87845759785033));
#15416=CARTESIAN_POINT('Ctrl Pts',(-0.257460542892226,5.91346045478468,
6.88624396315451));
#15417=CARTESIAN_POINT('Ctrl Pts',(-0.422770660606182,5.90394461256802,
6.89403032845869));
#15418=CARTESIAN_POINT('Ctrl Pts',(-0.587381565169692,5.88752184364515,
6.90181669376286));
#15419=CARTESIAN_POINT('Ctrl Pts',(-0.752035693214231,5.87109476243664,
6.90960510360846));
#15420=CARTESIAN_POINT('Ctrl Pts',(-0.915989922886949,5.84775716034388,
6.91739351345406));
#15421=CARTESIAN_POINT('Ctrl Pts',(-1.07865861177825,5.81759625289833,6.92518192329966));
#15422=CARTESIAN_POINT('Ctrl Pts',(-1.23277874243144,5.78902036021849,6.93256103695187));
#15423=CARTESIAN_POINT('Ctrl Pts',(-1.38574471671469,5.75431992011536,6.93994015060408));
#15424=CARTESIAN_POINT('Ctrl Pts',(-1.53706695700239,5.71361144392856,6.94731926425629));
#15425=CARTESIAN_POINT('Ctrl Pts',(-1.69677644504388,5.67064664325959,6.95510737564926));
#15426=CARTESIAN_POINT('Ctrl Pts',(-1.85471185969222,5.62097356837911,6.96289548704222));
#15427=CARTESIAN_POINT('Ctrl Pts',(-2.01030697854925,5.5647638237841,6.97068359843519));
#15428=CARTESIAN_POINT('Ctrl Pts',(-2.16587154901762,5.50856511499237,6.97847018076828));
#15429=CARTESIAN_POINT('Ctrl Pts',(-2.31909644015226,5.44583240567079,6.98625676310137));
#15430=CARTESIAN_POINT('Ctrl Pts',(-2.46943268377581,5.3767864736104,6.99404334543446));
#15431=CARTESIAN_POINT('Ctrl Pts',(-2.61977465968635,5.30773790884424,7.00183022466817));
#15432=CARTESIAN_POINT('Ctrl Pts',(-2.76722747568402,5.23237576942095,7.00961710390188));
#15433=CARTESIAN_POINT('Ctrl Pts',(-2.91126348692853,5.15096840139568,7.01740398313559));
#15434=CARTESIAN_POINT('Ctrl Pts',(-3.05528999187953,5.06956640620965,7.02519034843977));
#15435=CARTESIAN_POINT('Ctrl Pts',(-3.195899865215,4.98212013818004,7.03297671374395));
#15436=CARTESIAN_POINT('Ctrl Pts',(-3.33259122622223,4.88894326837678,7.04076307904814));
#15437=CARTESIAN_POINT('Ctrl Pts',(-3.46931847960501,4.79574193221969,7.04855148889372));
#15438=CARTESIAN_POINT('Ctrl Pts',(-3.60212489936952,4.69680716599325,7.05633989873932));
#15439=CARTESIAN_POINT('Ctrl Pts',(-3.73053794653349,4.59249574762717,7.06412830858491));
#15440=CARTESIAN_POINT('Ctrl Pts',(-3.85220263653191,4.49366609862274,7.07150742223707));
#15441=CARTESIAN_POINT('Ctrl Pts',(-3.96992363601487,4.39001053383125,7.07888653588924));
#15442=CARTESIAN_POINT('Ctrl Pts',(-4.08332677882751,4.28186559571995,7.08626564954141));
#15443=CARTESIAN_POINT('Ctrl Pts',(-4.20301545014583,4.16772657248557,7.09405376093436));
#15444=CARTESIAN_POINT('Ctrl Pts',(-4.31793679218021,4.0485456398114,7.1018418723273));
#15445=CARTESIAN_POINT('Ctrl Pts',(-4.42767569376072,3.92474438828576,7.10962998372025));
#15446=CARTESIAN_POINT('Ctrl Pts',(-4.53739305002053,3.80096744297813,7.11741656605326));
#15447=CARTESIAN_POINT('Ctrl Pts',(-4.64192978418409,3.67257222775606,7.12520314838627));
#15448=CARTESIAN_POINT('Ctrl Pts',(-4.74090946264455,3.54001525837211,7.13298973071929));
#15449=CARTESIAN_POINT('Ctrl Pts',(-4.83989291517847,3.40745323461996,7.14077660995298));
#15450=CARTESIAN_POINT('Ctrl Pts',(-4.93331869368738,3.27072939282946,7.14856348918667));
#15451=CARTESIAN_POINT('Ctrl Pts',(-5.02085184740838,3.13033181769535,7.15635036842036));
#15452=CARTESIAN_POINT('Ctrl Pts',(-5.10837922399208,2.98994350871965,7.16413673372455));
#15453=CARTESIAN_POINT('Ctrl Pts',(-5.19001458509246,2.84588222283844,7.17192309902873));
#15454=CARTESIAN_POINT('Ctrl Pts',(-5.26546728910059,2.6986635192094,7.17970946433292));
#15455=CARTESIAN_POINT('Ctrl Pts',(-5.34093980545652,2.55140615893846,7.18749787417851));
#15456=CARTESIAN_POINT('Ctrl Pts',(-5.41022627318604,2.40099000791569,7.19528628402409));
#15457=CARTESIAN_POINT('Ctrl Pts',(-5.47308244016529,2.24795444029774,7.20307469386968));
#15458=CARTESIAN_POINT('Ctrl Pts',(-5.53263539244729,2.10296119152379,7.21045380752197));
#15459=CARTESIAN_POINT('Ctrl Pts',(-5.58641641177452,1.95561699655019,7.21783292117426));
#15460=CARTESIAN_POINT('Ctrl Pts',(-5.63425794808955,1.80639639528254,7.22521203482654));
#15461=CARTESIAN_POINT('Ctrl Pts',(-5.68487660239283,1.64851379760097,7.23301949319431));
#15462=CARTESIAN_POINT('Ctrl Pts',(-5.72886366753598,1.48847477281738,7.24082695156208));
#15463=CARTESIAN_POINT('Ctrl Pts',(-5.76605560025257,1.32685092504622,7.24863440992985));
#15464=CARTESIAN_POINT('Ctrl Pts',(-5.80323914575064,1.16526352535476,7.25644010762387));
#15465=CARTESIAN_POINT('Ctrl Pts',(-5.83363054628982,1.00209232399418,7.2642458053179));
#15466=CARTESIAN_POINT('Ctrl Pts',(-5.85711694061192,0.837921062211063,
7.27205150301192));
#15467=CARTESIAN_POINT('Ctrl Pts',(-5.88060187927665,0.673759975557509,
7.27985671691856));
#15468=CARTESIAN_POINT('Ctrl Pts',(-5.89718261864945,0.508599264814231,
7.2876619308252));
#15469=CARTESIAN_POINT('Ctrl Pts',(-5.90679783623067,0.34303044238191,7.29546714473184));
#15470=CARTESIAN_POINT('Ctrl Pts',(-5.91343269372531,0.22878180129641,7.30085303241961));
#15471=CARTESIAN_POINT('Ctrl Pts',(-5.91675198364477,0.1143390029343,7.30623892010737));
#15472=CARTESIAN_POINT('Ctrl Pts',(-5.91674999911038,-0.000102602491467883,
7.31162480779513));
#15473=CARTESIAN_POINT('Origin',(0.,0.,0.));
#15474=CARTESIAN_POINT('',(-5.91674999870471,0.000123805739447762,9.3133751922049));
#15475=CARTESIAN_POINT('',(-5.91674999804438,0.000152124367665733,9.06162480779513));
#15476=CARTESIAN_POINT('',(-5.91675,-7.2459289488551E-16,0.));
#15477=CARTESIAN_POINT('Ctrl Pts',(-5.91674999870471,0.000123805739447762,
9.3133751922049));
#15478=CARTESIAN_POINT('Ctrl Pts',(-5.91674711889009,0.137751860954763,
9.30689527400423));
#15479=CARTESIAN_POINT('Ctrl Pts',(-5.91194070528015,0.275360352934919,
9.30041535580356));
#15480=CARTESIAN_POINT('Ctrl Pts',(-5.90234404326611,0.412632230225794,
9.29393543760289));
#15481=CARTESIAN_POINT('Ctrl Pts',(-5.89081016459092,0.577614301686852,
9.28614745984122));
#15482=CARTESIAN_POINT('Ctrl Pts',(-5.87235253261579,0.74214198003531,9.27835948207955));
#15483=CARTESIAN_POINT('Ctrl Pts',(-5.84703094864028,0.905626660463758,
9.27057150431788));
#15484=CARTESIAN_POINT('Ctrl Pts',(-5.82171434310529,1.06907919840233,9.26278505773942));
#15485=CARTESIAN_POINT('Ctrl Pts',(-5.78953652712413,1.23148883198974,9.25499861116095));
#15486=CARTESIAN_POINT('Ctrl Pts',(-5.75060887188758,1.39227445752188,9.24721216458248));
#15487=CARTESIAN_POINT('Ctrl Pts',(-5.71167973164869,1.55306621666338,9.23942542096862));
#15488=CARTESIAN_POINT('Ctrl Pts',(-5.66600030825776,1.71223353228523,9.23163867735477));
#15489=CARTESIAN_POINT('Ctrl Pts',(-5.61373274820993,1.86920710307216,9.22385193374091));
#15490=CARTESIAN_POINT('Ctrl Pts',(-5.56146864527017,2.02617029123174,9.21606570516189));
#15491=CARTESIAN_POINT('Ctrl Pts',(-5.50261737875396,2.18093972174852,9.20827947658287));
#15492=CARTESIAN_POINT('Ctrl Pts',(-5.43739052057007,2.33296268493835,9.20049324800385));
#15493=CARTESIAN_POINT('Ctrl Pts',(-5.37214649165009,2.48502566762711,9.19270496972813));
#15494=CARTESIAN_POINT('Ctrl Pts',(-5.30052364164677,2.63434044365937,9.1849166914524));
#15495=CARTESIAN_POINT('Ctrl Pts',(-5.22278147765959,2.78037483068667,9.17712841317668));
#15496=CARTESIAN_POINT('Ctrl Pts',(-5.14887192710607,2.9192098637882,9.16972408948125));
#15497=CARTESIAN_POINT('Ctrl Pts',(-5.06943200497215,3.05507992408495,9.16231976578582));
#15498=CARTESIAN_POINT('Ctrl Pts',(-4.98472296263196,3.18754883073337,9.15491544209038));
#15499=CARTESIAN_POINT('Ctrl Pts',(-4.89562473231721,3.32688159649295,9.14712746432892));
#15500=CARTESIAN_POINT('Ctrl Pts',(-4.80066497501037,3.46250123228239,9.13933948656745));
#15501=CARTESIAN_POINT('Ctrl Pts',(-4.70017794192323,3.59391957015712,9.13155150880598));
#15502=CARTESIAN_POINT('Ctrl Pts',(-4.59971066544827,3.72531207005997,9.1237650622277));
#15503=CARTESIAN_POINT('Ctrl Pts',(-4.49371847547923,3.85250466649364,9.11597861564943));
#15504=CARTESIAN_POINT('Ctrl Pts',(-4.38257731087115,3.97504046227676,9.10819216907115));
#15505=CARTESIAN_POINT('Ctrl Pts',(-4.27143190647816,4.09758093252428,9.10040542545749));
#15506=CARTESIAN_POINT('Ctrl Pts',(-4.15513734614906,4.2154640073063,9.09261868184383));
#15507=CARTESIAN_POINT('Ctrl Pts',(-4.03410849985289,4.32826745637497,9.08483193823017));
#15508=CARTESIAN_POINT('Ctrl Pts',(-3.91308765870954,4.44106344433932,9.07704570965135));
#15509=CARTESIAN_POINT('Ctrl Pts',(-3.78733339209091,4.54878026112686,9.06925948107253));
#15510=CARTESIAN_POINT('Ctrl Pts',(-3.65729602342713,4.65103390221187,9.06147325249371));
#15511=CARTESIAN_POINT('Ctrl Pts',(-3.52722442289306,4.75331446120066,9.05368497421818));
#15512=CARTESIAN_POINT('Ctrl Pts',(-3.3928677174589,4.85012877154615,9.04589669594264));
#15513=CARTESIAN_POINT('Ctrl Pts',(-3.25470849171235,4.94113379665796,9.03810841766711));
#15514=CARTESIAN_POINT('Ctrl Pts',(-3.1233603820424,5.02765236213423,9.03070409397069));
#15515=CARTESIAN_POINT('Ctrl Pts',(-2.98857586191077,5.108920484133,9.02329977027427));
#15516=CARTESIAN_POINT('Ctrl Pts',(-2.85079309458859,5.184680249962,9.01589544657785));
#15517=CARTESIAN_POINT('Ctrl Pts',(-2.70587113117589,5.26436549816109,9.00810746881631));
#15518=CARTESIAN_POINT('Ctrl Pts',(-2.5575801224491,5.33798491034792,9.00031949105477));
#15519=CARTESIAN_POINT('Ctrl Pts',(-2.40644720979684,5.40526987198243,8.99253151329323));
#15520=CARTESIAN_POINT('Ctrl Pts',(-2.25534401117084,5.47254160481666,8.98474506671488));
#15521=CARTESIAN_POINT('Ctrl Pts',(-2.10140031522255,5.53348124216589,8.97695862013653));
#15522=CARTESIAN_POINT('Ctrl Pts',(-1.94516489664656,5.58786757961872,8.96917217355819));
#15523=CARTESIAN_POINT('Ctrl Pts',(-1.78892351804169,5.64225599178768,8.96138542994446));
#15524=CARTESIAN_POINT('Ctrl Pts',(-1.63039054234946,5.69009049503393,8.95359868633074));
#15525=CARTESIAN_POINT('Ctrl Pts',(-1.47013233171216,5.73119895743941,8.94581194271702));
#15526=CARTESIAN_POINT('Ctrl Pts',(-1.30988472095649,5.77230470082766,8.93802571413813));
#15527=CARTESIAN_POINT('Ctrl Pts',(-1.14791241319261,5.80668521434587,8.93023948555924));
#15528=CARTESIAN_POINT('Ctrl Pts',(-0.98479460116806,5.83421889853391,8.92245325698035));
#15529=CARTESIAN_POINT('Ctrl Pts',(-0.821633848965534,5.86175983086539,
8.91466497870476));
#15530=CARTESIAN_POINT('Ctrl Pts',(-0.657327304919354,5.88245027713472,
8.90687670042917));
#15531=CARTESIAN_POINT('Ctrl Pts',(-0.492462876943627,5.89622004994152,
8.89908842215358));
#15532=CARTESIAN_POINT('Ctrl Pts',(-0.335726105669414,5.90931098627883,
8.8916840984575));
#15533=CARTESIAN_POINT('Ctrl Pts',(-0.178485394289553,5.91614715499982,
8.88427977476142));
#15534=CARTESIAN_POINT('Ctrl Pts',(-0.0212489029355745,5.91671184414317,
8.87687545106534));
#15535=CARTESIAN_POINT('Ctrl Pts',(0.144134776685753,5.91730579258074,8.86908747330382));
#15536=CARTESIAN_POINT('Ctrl Pts',(0.309572948295051,5.91096130722683,8.86129949554229));
#15537=CARTESIAN_POINT('Ctrl Pts',(0.474474206673456,5.89769487085434,8.85351151778077));
#15538=CARTESIAN_POINT('Ctrl Pts',(0.639343044050709,5.88443104277698,8.84572507120244));
#15539=CARTESIAN_POINT('Ctrl Pts',(0.803674860498382,5.86424800471654,8.83793862462411));
#15540=CARTESIAN_POINT('Ctrl Pts',(0.966881950513395,5.83721422052261,8.83015217804578));
#15541=CARTESIAN_POINT('Ctrl Pts',(1.13009526651102,5.81017940505075,8.82236543443207));
#15542=CARTESIAN_POINT('Ctrl Pts',(1.29218345433104,5.77629336881456,8.81457869081835));
#15543=CARTESIAN_POINT('Ctrl Pts',(1.45256685615463,5.73567607967021,8.80679194720464));
#15544=CARTESIAN_POINT('Ctrl Pts',(1.612939649816,5.69506147705569,8.79900571862576));
#15545=CARTESIAN_POINT('Ctrl Pts',(1.77160757335952,5.64771659105516,8.79121949004688));
#15546=CARTESIAN_POINT('Ctrl Pts',(1.92800389197832,5.59381189842995,8.78343326146801));
#15547=CARTESIAN_POINT('Ctrl Pts',(2.08444138136616,5.53989301558805,8.77564498319243));
#15548=CARTESIAN_POINT('Ctrl Pts',(2.23860576796796,5.47941097786755,8.76785670491686));
#15549=CARTESIAN_POINT('Ctrl Pts',(2.38994727436551,5.41258557329608,8.76006842664128));
#15550=CARTESIAN_POINT('Ctrl Pts',(2.53382779100609,5.34905459647865,8.75266410294513));
#15551=CARTESIAN_POINT('Ctrl Pts',(2.67515681233243,5.27979073685871,8.74525977924897));
#15552=CARTESIAN_POINT('Ctrl Pts',(2.81348017613379,5.20502256104642,8.73785545555282));
#15553=CARTESIAN_POINT('Ctrl Pts',(2.95897074696685,5.1263802819684,8.73006747779129));
#15554=CARTESIAN_POINT('Ctrl Pts',(3.10118796001897,5.04161999980981,8.72227950002975));
#15555=CARTESIAN_POINT('Ctrl Pts',(3.2396204534312,4.95103927273964,8.71449152226821));
#15556=CARTESIAN_POINT('Ctrl Pts',(3.37802572982839,4.86047635461699,8.70670507568987));
#15557=CARTESIAN_POINT('Ctrl Pts',(3.51264750407078,4.76409544975376,8.69891862911154));
#15558=CARTESIAN_POINT('Ctrl Pts',(3.64300254427932,4.66223798458148,8.6911321825332));
#15559=CARTESIAN_POINT('Ctrl Pts',(3.77336255723879,4.56037663377653,8.68334543891948));
#15560=CARTESIAN_POINT('Ctrl Pts',(3.89945525624355,4.45303849824056,8.67555869530575));
#15561=CARTESIAN_POINT('Ctrl Pts',(4.02082912853708,4.34060637257143,8.66777195169203));
#15562=CARTESIAN_POINT('Ctrl Pts',(4.14219497285695,4.22818168344632,8.65998572311315));
#15563=CARTESIAN_POINT('Ctrl Pts',(4.25884238068587,4.11066389569112,8.65219949453426));
#15564=CARTESIAN_POINT('Ctrl Pts',(4.37035536258719,3.9884739647145,8.64441326595538));
#15565=CARTESIAN_POINT('Ctrl Pts',(4.48189769988042,3.86625186767748,8.63662498767979));
#15566=CARTESIAN_POINT('Ctrl Pts',(4.58830269342953,3.73935540464159,8.62883670940421));
#15567=CARTESIAN_POINT('Ctrl Pts',(4.68919284601521,3.60824070917944,8.62104843112862));
#15568=CARTESIAN_POINT('Ctrl Pts',(4.78510921174593,3.48358984127697,8.61364410743252));
#15569=CARTESIAN_POINT('Ctrl Pts',(4.87604123022314,3.35512684063529,8.60623978373641));
#15570=CARTESIAN_POINT('Ctrl Pts',(4.96169955605135,3.22326978051479,8.5988354600403));
#15571=CARTESIAN_POINT('Ctrl Pts',(5.05179625684668,3.08458056404265,8.59104748227878));
#15572=CARTESIAN_POINT('Ctrl Pts',(5.13609047328364,2.94208661260913,8.58325950451725));
#15573=CARTESIAN_POINT('Ctrl Pts',(5.2142756628893,2.79629395341411,8.57547152675572));
#15574=CARTESIAN_POINT('Ctrl Pts',(5.29244548061638,2.65052995830582,8.56768508017739));
#15575=CARTESIAN_POINT('Ctrl Pts',(5.36450851710577,2.50146883093088,8.55989863359906));
#15576=CARTESIAN_POINT('Ctrl Pts',(5.4302039262082,2.34964164976131,8.55211218702073));
#15577=CARTESIAN_POINT('Ctrl Pts',(5.49590184144239,2.19780867672704,8.54432544340701));
#15578=CARTESIAN_POINT('Ctrl Pts',(5.55523151269775,2.04320973044566,8.5365386997933));
#15579=CARTESIAN_POINT('Ctrl Pts',(5.60797974468834,1.88639702758071,8.52875195617958));
#15580=CARTESIAN_POINT('Ctrl Pts',(5.66072448777801,1.72959469670288,8.5209657276007));
#15581=CARTESIAN_POINT('Ctrl Pts',(5.70688856094828,1.57057920519222,8.51317949902182));
#15582=CARTESIAN_POINT('Ctrl Pts',(5.74630822459167,1.40991927091238,8.50539327044294));
#15583=CARTESIAN_POINT('Ctrl Pts',(5.7857382653199,1.24921704348203,8.49760499216736));
#15584=CARTESIAN_POINT('Ctrl Pts',(5.81842027071806,1.08686981835545,8.48981671389178));
#15585=CARTESIAN_POINT('Ctrl Pts',(5.84424113584269,0.92345877472909,8.4820284356162));
#15586=CARTESIAN_POINT('Ctrl Pts',(5.8687890573129,0.768103737361335,8.47462411192006));
#15587=CARTESIAN_POINT('Ctrl Pts',(5.88713599670188,0.611787505531511,8.46721978822393));
#15588=CARTESIAN_POINT('Ctrl Pts',(5.89922802781789,0.455015646223092,8.45981546452779));
#15589=CARTESIAN_POINT('Ctrl Pts',(5.91194660594708,0.290120673497471,8.45202748676627));
#15590=CARTESIAN_POINT('Ctrl Pts',(5.91774942167743,0.124662617031762,8.44423950900474));
#15591=CARTESIAN_POINT('Ctrl Pts',(5.91660955052299,-0.0407675012736267,
8.43645153124322));
#15592=CARTESIAN_POINT('Ctrl Pts',(5.915469903477,-0.206165094599524,8.4286650846649));
#15593=CARTESIAN_POINT('Ctrl Pts',(5.9073902953071,-0.371534441378662,8.42087863808657));
#15594=CARTESIAN_POINT('Ctrl Pts',(5.89239591395816,-0.536284398122123,
8.41309219150824));
#15595=CARTESIAN_POINT('Ctrl Pts',(5.87740096060738,-0.701040639705004,
8.40530544789454));
#15596=CARTESIAN_POINT('Ctrl Pts',(5.85549073126761,-0.865177125389408,
8.39751870428083));
#15597=CARTESIAN_POINT('Ctrl Pts',(5.82674236932942,-1.02810696134276,8.38973196066712));
#15598=CARTESIAN_POINT('Ctrl Pts',(5.79799590888029,-1.19102602070637,8.38194573208824));
#15599=CARTESIAN_POINT('Ctrl Pts',(5.76241227657733,-1.35273827535683,8.37415950350937));
#15600=CARTESIAN_POINT('Ctrl Pts',(5.72011993630161,-1.51266601628543,8.3663732749305));
#15601=CARTESIAN_POINT('Ctrl Pts',(5.67781646271926,-1.67263585761727,8.35858499665492));
#15602=CARTESIAN_POINT('Ctrl Pts',(5.62880083209673,-1.83081993689766,8.35079671837935));
#15603=CARTESIAN_POINT('Ctrl Pts',(5.57325193019818,-1.98665384127237,8.34300844010378));
#15604=CARTESIAN_POINT('Ctrl Pts',(5.52044153538815,-2.13480528501913,8.33560411640761));
#15605=CARTESIAN_POINT('Ctrl Pts',(5.46172660855925,-2.28083244648607,8.32819979271144));
#15606=CARTESIAN_POINT('Ctrl Pts',(5.39730180110787,-2.42426562700082,8.32079546901528));
#15607=CARTESIAN_POINT('Ctrl Pts',(5.3295388306719,-2.57513077903245,8.31300749125375));
#15608=CARTESIAN_POINT('Ctrl Pts',(5.25543431630152,-2.72317996704022,8.30521951349223));
#15609=CARTESIAN_POINT('Ctrl Pts',(5.17524752126884,-2.86788138808089,8.2974315357307));
#15610=CARTESIAN_POINT('Ctrl Pts',(5.09507649164752,-3.01255435958162,8.28964508915237));
#15611=CARTESIAN_POINT('Ctrl Pts',(5.00882572218651,-3.15388059808576,8.28185864257405));
#15612=CARTESIAN_POINT('Ctrl Pts',(4.91680028888243,-3.29135313841368,8.27407219599572));
#15613=CARTESIAN_POINT('Ctrl Pts',(4.82477134501554,-3.42883092300911,8.26628545238201));
#15614=CARTESIAN_POINT('Ctrl Pts',(4.72696747096683,-3.56245444752342,8.25849870876829));
#15615=CARTESIAN_POINT('Ctrl Pts',(4.623737325253,-3.691745347334,8.25071196515458));
#15616=CARTESIAN_POINT('Ctrl Pts',(4.52051400744109,-3.82102769551873,8.24292573657571));
#15617=CARTESIAN_POINT('Ctrl Pts',(4.41186533567916,-3.94597774280306,8.23513950799683));
#15618=CARTESIAN_POINT('Ctrl Pts',(4.29818063121219,-4.06614975424816,8.22735327941796));
#15619=CARTESIAN_POINT('Ctrl Pts',(4.18446599965516,-4.18635340054358,8.21956500114239));
#15620=CARTESIAN_POINT('Ctrl Pts',(4.06571290465907,-4.30177626401508,8.21177672286681));
#15621=CARTESIAN_POINT('Ctrl Pts',(3.94234857326351,-4.41200841900684,8.20398844459124));
#15622=CARTESIAN_POINT('Ctrl Pts',(3.82506598398084,-4.51680623546958,8.19658412089507));
#15623=CARTESIAN_POINT('Ctrl Pts',(3.70361606165273,-4.61691263329247,8.18917979719891));
#15624=CARTESIAN_POINT('Ctrl Pts',(3.57839453890219,-4.71200839201873,8.18177547350275));
#15625=CARTESIAN_POINT('Ctrl Pts',(3.44668467930316,-4.81203152506474,8.17398749574121));
#15626=CARTESIAN_POINT('Ctrl Pts',(3.31075487724238,-4.90654676209905,8.16619951797967));
#15627=CARTESIAN_POINT('Ctrl Pts',(3.17108732161921,-4.99521128293548,8.15841154021814));
#15628=CARTESIAN_POINT('Ctrl Pts',(3.03144722583491,-5.08385837156695,8.1506250936398));
#15629=CARTESIAN_POINT('Ctrl Pts',(2.8880711123933,-5.16665686803163,8.14283864706146));
#15630=CARTESIAN_POINT('Ctrl Pts',(2.74146950457276,-5.24330768866348,8.13505220048312));
#15631=CARTESIAN_POINT('Ctrl Pts',(2.59486230423139,-5.31996143335133,8.12726545686939));
#15632=CARTESIAN_POINT('Ctrl Pts',(2.44502964463216,-5.39046688136825,8.11947871325567));
#15633=CARTESIAN_POINT('Ctrl Pts',(2.29250662419488,-5.45457092176118,8.11169196964195));
#15634=CARTESIAN_POINT('Ctrl Pts',(2.13999369201428,-5.51867072215144,8.10390574106306));
#15635=CARTESIAN_POINT('Ctrl Pts',(1.98479104975206,-5.57636983849608,8.09611951248417));
#15636=CARTESIAN_POINT('Ctrl Pts',(1.82745387879159,-5.62746327250472,8.08833328390528));
#15637=CARTESIAN_POINT('Ctrl Pts',(1.67007528938611,-5.67857015667632,8.08054500562969));
#15638=CARTESIAN_POINT('Ctrl Pts',(1.5105613519986,-5.72306778315643,8.0727567273541));
#15639=CARTESIAN_POINT('Ctrl Pts',(1.349483388428,-5.76080073833984,8.06496844907851));
#15640=CARTESIAN_POINT('Ctrl Pts',(1.19634641252904,-5.7966734953603,8.05756412538242));
#15641=CARTESIAN_POINT('Ctrl Pts',(1.04179616223938,-5.82643243777275,8.05015980168633));
#15642=CARTESIAN_POINT('Ctrl Pts',(0.886332889760116,-5.84998671545752,
8.04275547799024));
#15643=CARTESIAN_POINT('Ctrl Pts',(0.722814308118198,-5.87476145496474,
8.03496750022871));
#15644=CARTESIAN_POINT('Ctrl Pts',(0.558227082250128,-5.89268033330261,
8.02717952246719));
#15645=CARTESIAN_POINT('Ctrl Pts',(0.393158669071448,-5.90367316366971,
8.01939154470566));
#15646=CARTESIAN_POINT('Ctrl Pts',(0.228122709757993,-5.91466383275213,
8.01160509812734));
#15647=CARTESIAN_POINT('Ctrl Pts',(0.062606070547979,-5.91873114967639,
8.00381865154901));
#15648=CARTESIAN_POINT('Ctrl Pts',(-0.102799849404808,-5.9158568908876,
7.99603220497068));
#15649=CARTESIAN_POINT('Ctrl Pts',(-0.268212079220525,-5.91298252245233,
7.98824546135697));
#15650=CARTESIAN_POINT('Ctrl Pts',(-0.433513261767925,-5.90316605002174,
7.98045871774326));
#15651=CARTESIAN_POINT('Ctrl Pts',(-0.598112426644313,-5.8864413772324,
7.97267197412955));
#15652=CARTESIAN_POINT('Ctrl Pts',(-0.762700704517325,-5.86971781065504,
7.96488574555067));
#15653=CARTESIAN_POINT('Ctrl Pts',(-0.926586739710877,-5.84608699051395,
7.9570995169718));
#15654=CARTESIAN_POINT('Ctrl Pts',(-1.08918495901314,-5.8156346762464,7.94931328839293));
#15655=CARTESIAN_POINT('Ctrl Pts',(-1.25182598171256,-5.7851743455165,7.94152501011735));
#15656=CARTESIAN_POINT('Ctrl Pts',(-1.41317819644302,-5.74788898934669,
7.93373673184177));
#15657=CARTESIAN_POINT('Ctrl Pts',(-1.57266559333533,-5.70391562823638,
7.92594845356619));
#15658=CARTESIAN_POINT('Ctrl Pts',(-1.72429041595515,-5.6621101112597,7.91854412987003));
#15659=CARTESIAN_POINT('Ctrl Pts',(-1.87422960504385,-5.61426019909701,
7.91113980617387));
#15660=CARTESIAN_POINT('Ctrl Pts',(-2.02200045401077,-5.56052558005808,
7.90373548247772));
#15661=CARTESIAN_POINT('Ctrl Pts',(-2.17742803021923,-5.50400670875095,
7.89594750471619));
#15662=CARTESIAN_POINT('Ctrl Pts',(-2.33051219542683,-5.44095689128444,
7.88815952695465));
#15663=CARTESIAN_POINT('Ctrl Pts',(-2.48070356847719,-5.3715957003338,7.88037154919312));
#15664=CARTESIAN_POINT('Ctrl Pts',(-2.63086541261569,-5.30224814638808,
7.87258510261481));
#15665=CARTESIAN_POINT('Ctrl Pts',(-2.77813530948668,-5.2265918287544,7.86479865603649));
#15666=CARTESIAN_POINT('Ctrl Pts',(-2.92198528977122,-5.14489383066945,
7.85701220945817));
#15667=CARTESIAN_POINT('Ctrl Pts',(-3.06584075760832,-5.06319271598999,
7.84922546584446));
#15668=CARTESIAN_POINT('Ctrl Pts',(-3.20627576799496,-4.97544961403753,
7.84143872223075));
#15669=CARTESIAN_POINT('Ctrl Pts',(-3.34278767963744,-4.88197717030346,
7.83365197861705));
#15670=CARTESIAN_POINT('Ctrl Pts',(-3.47929056203824,-4.78851090907225,
7.82586575003817));
#15671=CARTESIAN_POINT('Ctrl Pts',(-3.61187060133811,-4.68931624504618,
7.8180795214593));
#15672=CARTESIAN_POINT('Ctrl Pts',(-3.74005471663466,-4.58474876946151,
7.81029329288043));
#15673=CARTESIAN_POINT('Ctrl Pts',(-3.86827257593912,-4.4801537668645,7.80250501460485));
#15674=CARTESIAN_POINT('Ctrl Pts',(-3.99209194987532,-4.37018332710374,
7.79471673632928));
#15675=CARTESIAN_POINT('Ctrl Pts',(-4.11107269111636,-4.25523347078128,
7.7869284580537));
#15676=CARTESIAN_POINT('Ctrl Pts',(-4.22418779699555,-4.14595053109636,
7.77952413435753));
#15677=CARTESIAN_POINT('Ctrl Pts',(-4.33292966830714,-4.03216749219219,
7.77211981066136));
#15678=CARTESIAN_POINT('Ctrl Pts',(-4.43695092800242,-3.91425561569482,
7.7647154869652));
#15679=CARTESIAN_POINT('Ctrl Pts',(-4.54636203568433,-3.79023415071524,
7.75692750920367));
#15680=CARTESIAN_POINT('Ctrl Pts',(-4.65058948652761,-3.66160025311989,
7.74913953144214));
#15681=CARTESIAN_POINT('Ctrl Pts',(-4.74925602814725,-3.5288096777252,7.74135155368061));
#15682=CARTESIAN_POINT('Ctrl Pts',(-4.84790317107891,-3.39604521009608,
7.73356510710228));
#15683=CARTESIAN_POINT('Ctrl Pts',(-4.94099139582116,-3.25912595163801,
7.72577866052395));
#15684=CARTESIAN_POINT('Ctrl Pts',(-5.02818499125749,-3.11853912211999,
7.71799221394562));
#15685=CARTESIAN_POINT('Ctrl Pts',(-5.11538191293291,-2.97794692953138,
7.7102054703319));
#15686=CARTESIAN_POINT('Ctrl Pts',(-5.19668358356026,-2.8336871553884,7.70241872671819));
#15687=CARTESIAN_POINT('Ctrl Pts',(-5.27179833909937,-2.68627489925532,
7.69463198310447));
#15688=CARTESIAN_POINT('Ctrl Pts',(-5.3469081263593,-2.53887239334023,7.6868457545256));
#15689=CARTESIAN_POINT('Ctrl Pts',(-5.41583167244711,-2.38831810749391,
7.67905952594672));
#15690=CARTESIAN_POINT('Ctrl Pts',(-5.47832382396314,-2.23515069789441,
7.67127329736785));
#15691=CARTESIAN_POINT('Ctrl Pts',(-5.54083242631362,-2.08194296752444,
7.66348501909227));
#15692=CARTESIAN_POINT('Ctrl Pts',(-5.59690612843184,-1.92612103417125,
7.65569674081668));
#15693=CARTESIAN_POINT('Ctrl Pts',(-5.64634804469368,-1.76824328662202,
7.6479084625411));
#15694=CARTESIAN_POINT('Ctrl Pts',(-5.69335252234669,-1.61814875919138,
7.64050413884496));
#15695=CARTESIAN_POINT('Ctrl Pts',(-5.73436326555133,-1.46619648556496,
7.63309981514882));
#15696=CARTESIAN_POINT('Ctrl Pts',(-5.76925298933626,-1.31287871013838,
7.62569549145268));
#15697=CARTESIAN_POINT('Ctrl Pts',(-5.80662370099699,-1.14865859726936,
7.61776465062411));
#15698=CARTESIAN_POINT('Ctrl Pts',(-5.83698281989535,-0.982822746918895,
7.60983380979554));
#15699=CARTESIAN_POINT('Ctrl Pts',(-5.86021483926551,-0.815973406522722,
7.60190296896697));
#15700=CARTESIAN_POINT('Ctrl Pts',(-5.88344102365571,-0.649165972193497,
7.59397412005725));
#15701=CARTESIAN_POINT('Ctrl Pts',(-5.89954364132265,-0.481345846958705,
7.58604527114753));
#15702=CARTESIAN_POINT('Ctrl Pts',(-5.90845873389386,-0.313122902984345,
7.57811642223781));
#15703=CARTESIAN_POINT('Ctrl Pts',(-5.91398368173311,-0.208870144709672,
7.57320267890856));
#15704=CARTESIAN_POINT('Ctrl Pts',(-5.9167491721295,-0.104462820545378,
7.56828893557931));
#15705=CARTESIAN_POINT('Ctrl Pts',(-5.91674999981411,-4.6900922432644E-5,
7.56337519225006));
#15706=CARTESIAN_POINT('Ctrl Pts',(-5.9163616306653,-0.000102807950176053,
7.3116248177821));
#15707=CARTESIAN_POINT('Ctrl Pts',(-5.91659180076628,-0.372163743325732,
7.32913601855862));
#15708=CARTESIAN_POINT('Ctrl Pts',(-5.79067067213347,-1.72813661589886,
7.39296268109683));
#15709=CARTESIAN_POINT('Ctrl Pts',(-4.76676170732884,-3.91409292922659,
7.50310480539682));
#15710=CARTESIAN_POINT('Ctrl Pts',(-2.31316218083295,-5.71764124077766,
7.64205119068191));
#15711=CARTESIAN_POINT('Ctrl Pts',(0.704280682558441,-6.12748964529958,
7.78099757596707));
#15712=CARTESIAN_POINT('Ctrl Pts',(3.55005206806716,-5.04373581257866,7.91994396125215));
#15713=CARTESIAN_POINT('Ctrl Pts',(5.53048282990672,-2.73054945041935,8.05889034653732));
#15714=CARTESIAN_POINT('Ctrl Pts',(6.16283436094425,0.24822020997984,8.19783673182242));
#15715=CARTESIAN_POINT('Ctrl Pts',(5.29296822665717,3.16648511518309,8.33678311710757));
#15716=CARTESIAN_POINT('Ctrl Pts',(3.13291807858667,5.31290550884743,8.47572950239266));
#15717=CARTESIAN_POINT('Ctrl Pts',(0.209205530063851,6.16428208952746,8.61467588767782));
#15718=CARTESIAN_POINT('Ctrl Pts',(-2.76550177582862,5.51308811474716,8.75362227296292));
#15719=CARTESIAN_POINT('Ctrl Pts',(-5.06610600222509,3.51805494660003,8.89256865824806));
#15720=CARTESIAN_POINT('Ctrl Pts',(-5.85356588340937,1.41028719109854,8.99523616985879));
#15721=CARTESIAN_POINT('Ctrl Pts',(-5.91701383422643,0.213355077629451,
9.05158821970782));
#15722=CARTESIAN_POINT('Ctrl Pts',(-5.91679358169284,0.000152125488236412,
9.06162480779513));
#15723=CARTESIAN_POINT('Origin',(0.,0.,0.));
#15724=CARTESIAN_POINT('',(-5.91662392833365,-0.000151321579282548,11.0633751922049));
#15725=CARTESIAN_POINT('',(-5.91674999820671,-0.000145674166851941,10.811624807754));
#15726=CARTESIAN_POINT('',(-5.91675,-7.2459289488551E-16,0.));
#15727=CARTESIAN_POINT('Ctrl Pts',(-5.91662392833365,-0.000151321579282548,
11.0633751922049));
#15728=CARTESIAN_POINT('Ctrl Pts',(-5.91592640289124,0.716489165398392,
11.029641922721));
#15729=CARTESIAN_POINT('Ctrl Pts',(-5.60646173926398,2.4181775648746,10.9495686547327));
#15730=CARTESIAN_POINT('Ctrl Pts',(-4.01268187007679,4.6844298163471,10.8231553882407));
#15731=CARTESIAN_POINT('Ctrl Pts',(-1.28083654461856,6.03365198206632,10.6841353927279));
#15732=CARTESIAN_POINT('Ctrl Pts',(1.76354224681853,5.91061902328436,10.5451153972156));
#15733=CARTESIAN_POINT('Ctrl Pts',(4.37760385757118,4.34535187998648,10.406095401703));
#15734=CARTESIAN_POINT('Ctrl Pts',(5.92349817403787,1.71978716034709,10.2670754061905));
#15735=CARTESIAN_POINT('Ctrl Pts',(6.02401569919722,-1.32541817949976,10.128055410678));
#15736=CARTESIAN_POINT('Ctrl Pts',(4.65462942321255,-4.04721180904692,9.98903541516539));
#15737=CARTESIAN_POINT('Ctrl Pts',(2.14947959285796,-5.78145621574806,9.85001541965299));
#15738=CARTESIAN_POINT('Ctrl Pts',(-0.880158947650844,-6.10498310575821,
9.71099542414042));
#15739=CARTESIAN_POINT('Ctrl Pts',(-3.69503228047053,-4.9388495564256,9.57197542862794));
#15740=CARTESIAN_POINT('Ctrl Pts',(-5.51911104469368,-2.67812797647235,
9.43943535444122));
#15741=CARTESIAN_POINT('Ctrl Pts',(-5.9162401127627,-0.846510755967147,
9.35323527875873));
#15742=CARTESIAN_POINT('Ctrl Pts',(-5.91702658122213,0.000123612389871874,
9.31337520158039));
#15743=CARTESIAN_POINT('Ctrl Pts',(-5.91674999804438,0.000152124367665733,
9.06162480779513));
#15744=CARTESIAN_POINT('Ctrl Pts',(-5.9167542351693,-0.164647303984843,
9.06938284393673));
#15745=CARTESIAN_POINT('Ctrl Pts',(-5.90986888391126,-0.329469705868361,
9.07714088007834));
#15746=CARTESIAN_POINT('Ctrl Pts',(-5.89611425490407,-0.493727916586623,
9.08489891621994));
#15747=CARTESIAN_POINT('Ctrl Pts',(-5.88235943528536,-0.657988403593735,
9.09265705987234));
#15748=CARTESIAN_POINT('Ctrl Pts',(-5.86173517019319,-0.821684360345096,
9.10041520352474));
#15749=CARTESIAN_POINT('Ctrl Pts',(-5.83431375174233,-0.984232497294403,
9.10817334717714));
#15750=CARTESIAN_POINT('Ctrl Pts',(-5.80689385051353,-1.146771640485,9.11593106157288));
#15751=CARTESIAN_POINT('Ctrl Pts',(-5.77267760299697,-1.30816277131651,
9.12368877596861));
#15752=CARTESIAN_POINT('Ctrl Pts',(-5.73178868066648,-1.4678314217524,9.13144649036434));
#15753=CARTESIAN_POINT('Ctrl Pts',(-5.69088963594573,-1.62753959948071,
9.13920612524631));
#15754=CARTESIAN_POINT('Ctrl Pts',(-5.64331469579614,-1.78552413041893,
9.14696576012827));
#15755=CARTESIAN_POINT('Ctrl Pts',(-5.5892380063774,-1.941223601383,9.15472539501024));
#15756=CARTESIAN_POINT('Ctrl Pts',(-5.55268333914261,-2.04647306119465,
9.15997073961293));
#15757=CARTESIAN_POINT('Ctrl Pts',(-5.51315876414372,-2.1506786540877,9.16521608421562));
#15758=CARTESIAN_POINT('Ctrl Pts',(-5.47073076945238,-2.25367154010229,
9.17046142881831));
#15759=CARTESIAN_POINT('Ctrl Pts',(-5.40773510875417,-2.40659191611593,
9.17824954021127));
#15760=CARTESIAN_POINT('Ctrl Pts',(-5.33831243462539,-2.55689661293207,
9.18603765160423));
#15761=CARTESIAN_POINT('Ctrl Pts',(-5.26270520986413,-2.70404593832444,
9.1938257629972));
#15762=CARTESIAN_POINT('Ctrl Pts',(-5.18711282926339,-2.85116637351204,
9.20161234533026));
#15763=CARTESIAN_POINT('Ctrl Pts',(-5.1053384667167,-2.99513238933499,9.20939892766332));
#15764=CARTESIAN_POINT('Ctrl Pts',(-5.01767115424125,-3.13542768221423,
9.21718550999638));
#15765=CARTESIAN_POINT('Ctrl Pts',(-4.93000049903071,-3.27572832452172,
9.22497238923009));
#15766=CARTESIAN_POINT('Ctrl Pts',(-4.83643661024355,-3.4123576907616,9.2327592684638));
#15767=CARTESIAN_POINT('Ctrl Pts',(-4.73731297790831,-3.54482669701094,
9.24054614769751));
#15768=CARTESIAN_POINT('Ctrl Pts',(-4.6381958876755,-3.67728696038244,9.2483325130017));
#15769=CARTESIAN_POINT('Ctrl Pts',(-4.53351997974197,-3.8055871574595,9.25611887830588));
#15770=CARTESIAN_POINT('Ctrl Pts',(-4.42366041050591,-3.92926954216973,
9.26390524361006));
#15771=CARTESIAN_POINT('Ctrl Pts',(-4.313771994378,-4.05298440336243,9.27169365345564));
#15772=CARTESIAN_POINT('Ctrl Pts',(-4.19869740802239,-4.17207878893119,
9.27948206330123));
#15773=CARTESIAN_POINT('Ctrl Pts',(-4.07885081761466,-4.28612955592155,
9.28727047314682));
#15774=CARTESIAN_POINT('Ctrl Pts',(-3.96530240028921,-4.3941867317031,9.29464958679902));
#15775=CARTESIAN_POINT('Ctrl Pts',(-3.84747082336385,-4.49771657914358,
9.30202870045123));
#15776=CARTESIAN_POINT('Ctrl Pts',(-3.7257376286415,-4.5963909412739,9.30940781410344));
#15777=CARTESIAN_POINT('Ctrl Pts',(-3.59725720058452,-4.7005344685482,9.31719592549638));
#15778=CARTESIAN_POINT('Ctrl Pts',(-3.46438449849465,-4.79930619834674,
9.32498403688933));
#15779=CARTESIAN_POINT('Ctrl Pts',(-3.32759064228207,-4.89234821735911,
9.33277214828227));
#15780=CARTESIAN_POINT('Ctrl Pts',(-3.19082364315839,-4.98537196919307,
9.34055873061532));
#15781=CARTESIAN_POINT('Ctrl Pts',(-3.05013729003561,-5.07266807521593,
9.34834531294836));
#15782=CARTESIAN_POINT('Ctrl Pts',(-2.90603240636465,-5.15392144057886,
9.3561318952814));
#15783=CARTESIAN_POINT('Ctrl Pts',(-2.76192202800644,-5.2351779041146,9.36391877451511));
#15784=CARTESIAN_POINT('Ctrl Pts',(-2.61439313465634,-5.31039100557254,
9.37170565374881));
#15785=CARTESIAN_POINT('Ctrl Pts',(-2.46397256651647,-5.37929082258565,
9.37949253298251));
#15786=CARTESIAN_POINT('Ctrl Pts',(-2.31356192604721,-5.44818609225064,
9.38727889828668));
#15787=CARTESIAN_POINT('Ctrl Pts',(-2.1602602832813,-5.51076877833009,9.39506526359085));
#15788=CARTESIAN_POINT('Ctrl Pts',(-2.00461607347838,-5.56681641159937,
9.40285162889502));
#15789=CARTESIAN_POINT('Ctrl Pts',(-1.84893099466638,-5.62287876183909,
9.41064003874062));
#15790=CARTESIAN_POINT('Ctrl Pts',(-1.69090241986903,-5.67240252024348,
9.41842844858621));
#15791=CARTESIAN_POINT('Ctrl Pts',(-1.53109648437006,-5.71521426702881,
9.4262168584318));
#15792=CARTESIAN_POINT('Ctrl Pts',(-1.37968866380985,-5.75577617266081,
9.43359597208405));
#15793=CARTESIAN_POINT('Ctrl Pts',(-1.22668573656425,-5.79031331334059,
9.44097508573631));
#15794=CARTESIAN_POINT('Ctrl Pts',(-1.07257974506573,-5.81872006999604,
9.44835419938856));
#15795=CARTESIAN_POINT('Ctrl Pts',(-0.90993221249251,-5.84870131104637,
9.45614231078154));
#15796=CARTESIAN_POINT('Ctrl Pts',(-0.745997781172773,-5.87186403532856,
9.46393042217451));
#15797=CARTESIAN_POINT('Ctrl Pts',(-0.581361390602742,-5.88811935137328,
9.47171853356749));
#15798=CARTESIAN_POINT('Ctrl Pts',(-0.416757323518033,-5.90437147597006,
9.47950511590056));
#15799=CARTESIAN_POINT('Ctrl Pts',(-0.251451889955782,-5.91371886687374,
9.48729169823363));
#15800=CARTESIAN_POINT('Ctrl Pts',(-0.0860356269073524,-5.9161244437049,
9.4950782805667));
#15801=CARTESIAN_POINT('Ctrl Pts',(0.0793869434263262,-5.91853011226017,
9.50286515980042));
#15802=CARTESIAN_POINT('Ctrl Pts',(0.24492003227762,-5.9139934285044,9.51065203903415));
#15803=CARTESIAN_POINT('Ctrl Pts',(0.40997186886024,-5.90252942637673,9.51843891826787));
#15804=CARTESIAN_POINT('Ctrl Pts',(0.575012812117128,-5.89106618086658,
9.52622528357206));
#15805=CARTESIAN_POINT('Ctrl Pts',(0.739572247889583,-5.87267655416949,
9.53401164887625));
#15806=CARTESIAN_POINT('Ctrl Pts',(0.903062145535117,-5.84742758174922,
9.54179801418045));
#15807=CARTESIAN_POINT('Ctrl Pts',(1.0665949723077,-5.82217197946154,9.54958642402605));
#15808=CARTESIAN_POINT('Ctrl Pts',(1.22905738348968,-5.79005347931028,9.55737483387165));
#15809=CARTESIAN_POINT('Ctrl Pts',(1.38986927262554,-5.75119065650856,9.56516324371726));
#15810=CARTESIAN_POINT('Ctrl Pts',(1.54223018198633,-5.71437015117021,9.57254235736941));
#15811=CARTESIAN_POINT('Ctrl Pts',(1.69310933092947,-5.67149600691549,9.57992147102155));
#15812=CARTESIAN_POINT('Ctrl Pts',(1.84202411387482,-5.6227108876772,9.5873005846737));
#15813=CARTESIAN_POINT('Ctrl Pts',(1.99919270786961,-5.57122178466877,9.59508869606666));
#15814=CARTESIAN_POINT('Ctrl Pts',(2.15422913816093,-5.51312948870221,9.60287680745961));
#15815=CARTESIAN_POINT('Ctrl Pts',(2.30657722721143,-5.44863579783138,9.61066491885257));
#15816=CARTESIAN_POINT('Ctrl Pts',(2.45889540537103,-5.38415476917223,9.61845150118565));
#15817=CARTESIAN_POINT('Ctrl Pts',(2.60852600135886,-5.31327497779059,9.62623808351872));
#15818=CARTESIAN_POINT('Ctrl Pts',(2.75493271060179,-5.23624639628009,9.6340246658518));
#15819=CARTESIAN_POINT('Ctrl Pts',(2.90134500229945,-5.15921487768719,9.6418115450855));
#15820=CARTESIAN_POINT('Ctrl Pts',(3.04453287667135,-5.07603424510427,9.6495984243192));
#15821=CARTESIAN_POINT('Ctrl Pts',(3.18398387904865,-4.98700082418865,9.65738530355291));
#15822=CARTESIAN_POINT('Ctrl Pts',(3.32342567774074,-4.89797327942714,9.6651716688571));
#15823=CARTESIAN_POINT('Ctrl Pts',(3.45913082870976,-4.80309389140064,9.67295803416129));
#15824=CARTESIAN_POINT('Ctrl Pts',(3.59061504095564,-4.70270286007559,9.68074439946549));
#15825=CARTESIAN_POINT('Ctrl Pts',(3.72213377828536,-4.60228546810454,9.68853280931108));
#15826=CARTESIAN_POINT('Ctrl Pts',(3.84942910690183,-4.49635373342895,9.69632121915667));
#15827=CARTESIAN_POINT('Ctrl Pts',(3.97204835264803,-4.38528932303515,9.70410962900226));
#15828=CARTESIAN_POINT('Ctrl Pts',(4.08822371684238,-4.2800615649617,9.71148874265444));
#15829=CARTESIAN_POINT('Ctrl Pts',(4.20020163905907,-4.17022689480854,9.71886785630663));
#15830=CARTESIAN_POINT('Ctrl Pts',(4.30762658777829,-4.05614148455963,9.72624696995881));
#15831=CARTESIAN_POINT('Ctrl Pts',(4.42100571519722,-3.9357327301737,9.73403508135178));
#15832=CARTESIAN_POINT('Ctrl Pts',(4.52935334063389,-3.81054566362723,9.74182319274476));
#15833=CARTESIAN_POINT('Ctrl Pts',(4.63227761920229,-3.68102358334439,9.74961130413774));
#15834=CARTESIAN_POINT('Ctrl Pts',(4.73518169038258,-3.55152693246442,9.75739788647079));
#15835=CARTESIAN_POINT('Ctrl Pts',(4.83266434057913,-3.41769721606165,9.76518446880384));
#15836=CARTESIAN_POINT('Ctrl Pts',(4.92437422420804,-3.28001052779644,9.77297105113689));
#15837=CARTESIAN_POINT('Ctrl Pts',(5.01608760471454,-3.14231858956823,9.78075793037061));
#15838=CARTESIAN_POINT('Ctrl Pts',(5.1020275977916,-3.00076964893625,9.78854480960432));
#15839=CARTESIAN_POINT('Ctrl Pts',(5.18188597794096,-2.8558690926089,9.79633168883804));
#15840=CARTESIAN_POINT('Ctrl Pts',(5.26173908748337,-2.71097809963459,9.80411805414223));
#15841=CARTESIAN_POINT('Ctrl Pts',(5.33551123318978,-2.56273621355105,9.81190441944641));
#15842=CARTESIAN_POINT('Ctrl Pts',(5.40293991173904,-2.41167387360674,9.81969078475059));
#15843=CARTESIAN_POINT('Ctrl Pts',(5.47038629568999,-2.26057186775961,9.82747919459619));
#15844=CARTESIAN_POINT('Ctrl Pts',(5.53148575203806,-2.10664821937205,9.83526760444178));
#15845=CARTESIAN_POINT('Ctrl Pts',(5.58602338021825,-1.95045465421657,9.84305601428737));
#15846=CARTESIAN_POINT('Ctrl Pts',(5.63769494920871,-1.80246936686354,9.85043512793956));
#15847=CARTESIAN_POINT('Ctrl Pts',(5.68347653938985,-1.65244684911322,9.85781424159176));
#15848=CARTESIAN_POINT('Ctrl Pts',(5.72322635565564,-1.5008699625313,9.86519335524395));
#15849=CARTESIAN_POINT('Ctrl Pts',(5.76517936133073,-1.34089171406683,9.87298146663691));
#15850=CARTESIAN_POINT('Ctrl Pts',(5.80042797722494,-1.17912476859988,9.88076957802986));
#15851=CARTESIAN_POINT('Ctrl Pts',(5.82884020499789,-1.01614586900707,9.88855768942282));
#15852=CARTESIAN_POINT('Ctrl Pts',(5.85724685452527,-0.853198967479796,
9.89634427175589));
#15853=CARTESIAN_POINT('Ctrl Pts',(5.87881973918856,-0.689040901186373,
9.90413085408895));
#15854=CARTESIAN_POINT('Ctrl Pts',(5.89347811440653,-0.524257834954607,
9.91191743642202));
#15855=CARTESIAN_POINT('Ctrl Pts',(5.90813704854507,-0.359468485581343,
9.91970431565573));
#15856=CARTESIAN_POINT('Ctrl Pts',(5.91588091343333,-0.194054406492899,
9.92749119488943));
#15857=CARTESIAN_POINT('Ctrl Pts',(5.91668084404873,-0.0286068552416584,
9.93527807412314));
#15858=CARTESIAN_POINT('Ctrl Pts',(5.91748072186918,0.136829776566631,9.94306443942731));
#15859=CARTESIAN_POINT('Ctrl Pts',(5.9113375811097,0.302299556566704,9.95085080473149));
#15860=CARTESIAN_POINT('Ctrl Pts',(5.89827469245367,0.467211103100703,9.95863717003566));
#15861=CARTESIAN_POINT('Ctrl Pts',(5.88520837374833,0.632165952058229,9.96642557988126));
#15862=CARTESIAN_POINT('Ctrl Pts',(5.86521869974376,0.796561955757151,9.97421398972685));
#15863=CARTESIAN_POINT('Ctrl Pts',(5.8383809264139,0.959811815194203,9.98200239957245));
#15864=CARTESIAN_POINT('Ctrl Pts',(5.81295353064259,1.11448257474256,9.98938151322465));
#15865=CARTESIAN_POINT('Ctrl Pts',(5.78137932716879,1.26812429924061,9.99676062687685));
#15866=CARTESIAN_POINT('Ctrl Pts',(5.74376482047373,1.42024513714652,10.0041397405291));
#15867=CARTESIAN_POINT('Ctrl Pts',(5.70406547690208,1.58079748620148,10.011927851922));
#15868=CARTESIAN_POINT('Ctrl Pts',(5.65762307990393,1.73971291443102,10.019715963315));
#15869=CARTESIAN_POINT('Ctrl Pts',(5.60459765285382,1.89642181808939,10.027504074708));
#15870=CARTESIAN_POINT('Ctrl Pts',(5.55158263642175,2.05309995468695,10.0352906570411));
#15871=CARTESIAN_POINT('Ctrl Pts',(5.49198727113722,2.20757212861727,10.0430772393742));
#15872=CARTESIAN_POINT('Ctrl Pts',(5.42602109526431,2.35928498410995,10.0508638217073));
#15873=CARTESIAN_POINT('Ctrl Pts',(5.36005240411601,2.51100362437956,10.058650700941));
#15874=CARTESIAN_POINT('Ctrl Pts',(5.28771254008613,2.659962441092,10.0664375801748));
#15875=CARTESIAN_POINT('Ctrl Pts',(5.20925903460248,2.80562842744945,10.0742244594085));
#15876=CARTESIAN_POINT('Ctrl Pts',(5.13081070700497,2.95128479993576,10.0820108247127));
#15877=CARTESIAN_POINT('Ctrl Pts',(5.04624969704373,3.09364849568054,10.0897971900169));
#15878=CARTESIAN_POINT('Ctrl Pts',(4.95587937707644,3.2322113424664,10.0975835553211));
#15879=CARTESIAN_POINT('Ctrl Pts',(4.86548532769812,3.37081057304227,10.1053719651667));
#15880=CARTESIAN_POINT('Ctrl Pts',(4.76927909327423,3.5056066915216,10.1131603750123));
#15881=CARTESIAN_POINT('Ctrl Pts',(4.66760774234685,3.63611998235533,10.1209487848579));
#15882=CARTESIAN_POINT('Ctrl Pts',(4.57127942006711,3.75977454410303,10.12832789851));
#15883=CARTESIAN_POINT('Ctrl Pts',(4.47004577228953,3.87958463711967,10.1357070121621));
#15884=CARTESIAN_POINT('Ctrl Pts',(4.36423564215233,3.99516931083869,10.1430861258142));
#15885=CARTESIAN_POINT('Ctrl Pts',(4.25256083690262,4.11716042748022,10.1508742372072));
#15886=CARTESIAN_POINT('Ctrl Pts',(4.13574796316561,4.23448801203535,10.1586623486001));
#15887=CARTESIAN_POINT('Ctrl Pts',(4.0142100596376,4.34672844327826,10.1664504599931));
#15888=CARTESIAN_POINT('Ctrl Pts',(3.89269601795853,4.45894683806887,10.1742370423262));
#15889=CARTESIAN_POINT('Ctrl Pts',(3.76645903207633,4.56607985574839,10.1820236246592));
#15890=CARTESIAN_POINT('Ctrl Pts',(3.63594784723766,4.66774183247829,10.1898102069922));
#15891=CARTESIAN_POINT('Ctrl Pts',(3.50543168603635,4.76940768555691,10.197597086226));
#15892=CARTESIAN_POINT('Ctrl Pts',(3.3706412494076,4.86560188079502,10.2053839654597));
#15893=CARTESIAN_POINT('Ctrl Pts',(3.23205769082457,4.95597958487338,10.2131708446934));
#15894=CARTESIAN_POINT('Ctrl Pts',(3.09348327867668,5.04635132407528,10.2209572099975));
#15895=CARTESIAN_POINT('Ctrl Pts',(2.95111651327928,5.13090716587141,10.2287435753017));
#15896=CARTESIAN_POINT('Ctrl Pts',(2.80546692033342,5.20934601667185,10.2365299406058));
#15897=CARTESIAN_POINT('Ctrl Pts',(2.65977908276168,5.28780546392192,10.2443183504514));
#15898=CARTESIAN_POINT('Ctrl Pts',(2.51080697576852,5.36014455734318,10.252106760297));
#15899=CARTESIAN_POINT('Ctrl Pts',(2.35908488099827,5.42610809759125,10.2598951701426));
#15900=CARTESIAN_POINT('Ctrl Pts',(2.21533607950236,5.48860512458951,10.2672742837948));
#15901=CARTESIAN_POINT('Ctrl Pts',(2.06911912912654,5.54537935514081,10.2746533974471));
#15902=CARTESIAN_POINT('Ctrl Pts',(1.92090505472162,5.59625359801045,10.2820325110993));
#15903=CARTESIAN_POINT('Ctrl Pts',(1.76447600702374,5.64994761726201,10.2898206224923));
#15904=CARTESIAN_POINT('Ctrl Pts',(1.60576630230671,5.69708824938458,10.2976087338852));
#15905=CARTESIAN_POINT('Ctrl Pts',(1.44534131461086,5.7375011151876,10.3053968452782));
#15906=CARTESIAN_POINT('Ctrl Pts',(1.28494782356525,5.77790604662879,10.3131834276113));
#15907=CARTESIAN_POINT('Ctrl Pts',(1.1228400311459,5.81158576929197,10.3209700099443));
#15908=CARTESIAN_POINT('Ctrl Pts',(0.959596505977468,5.8384163185076,10.3287565922774));
#15909=CARTESIAN_POINT('Ctrl Pts',(0.796346756369521,5.86524789076614,10.3365434715111));
#15910=CARTESIAN_POINT('Ctrl Pts',(0.631961502003953,5.88522971128476,10.3443303507448));
#15911=CARTESIAN_POINT('Ctrl Pts',(0.467028235148636,5.89828917484332,10.3521172299785));
#15912=CARTESIAN_POINT('Ctrl Pts',(0.302105853793364,5.91134777648486,10.3599035952827));
#15913=CARTESIAN_POINT('Ctrl Pts',(0.136635850892719,5.91748491033067,10.3676899605869));
#15914=CARTESIAN_POINT('Ctrl Pts',(-0.0287902936134475,5.91667995428971,
10.375476325891));
#15915=CARTESIAN_POINT('Ctrl Pts',(-0.194259875665475,5.91587478688363,
10.3832647357366));
#15916=CARTESIAN_POINT('Ctrl Pts',(-0.359685256566639,5.90812388676744,
10.3910531455822));
#15917=CARTESIAN_POINT('Ctrl Pts',(-0.524475175043601,5.89345877675097,
10.3988415554278));
#15918=CARTESIAN_POINT('Ctrl Pts',(-0.680605060512899,5.87956434699198,
10.40622066908));
#15919=CARTESIAN_POINT('Ctrl Pts',(-0.836164296225479,5.85946374958126,
10.4135997827322));
#15920=CARTESIAN_POINT('Ctrl Pts',(-0.990654489972888,5.83322674374969,
10.4209788963844));
#15921=CARTESIAN_POINT('Ctrl Pts',(-1.15370751974506,5.80553551501071,10.4287670077774));
#15922=CARTESIAN_POINT('Ctrl Pts',(-1.31562787500577,5.77099846070048,10.4365551191703));
#15923=CARTESIAN_POINT('Ctrl Pts',(-1.4758356587507,5.72973294934938,10.4443432305633));
#15924=CARTESIAN_POINT('Ctrl Pts',(-1.63601198849001,5.68847553976209,10.4521298128963));
#15925=CARTESIAN_POINT('Ctrl Pts',(-1.79447610836175,5.64049238860399,10.4599163952294));
#15926=CARTESIAN_POINT('Ctrl Pts',(-1.95066065498055,5.5859514473016,10.4677029775624));
#15927=CARTESIAN_POINT('Ctrl Pts',(-2.10685115688151,5.5314084263652,10.4754898567961));
#15928=CARTESIAN_POINT('Ctrl Pts',(-2.26076160864956,5.47030721655194,10.4832767360299));
#15929=CARTESIAN_POINT('Ctrl Pts',(-2.41184138301624,5.40286513857882,10.4910636152636));
#15930=CARTESIAN_POINT('Ctrl Pts',(-2.56291118620474,5.33542751174403,10.4988499805677));
#15931=CARTESIAN_POINT('Ctrl Pts',(-2.71115039410231,5.2616499845865,10.5066363458719));
#15932=CARTESIAN_POINT('Ctrl Pts',(-2.85602974833675,5.18179743323835,10.514422711176));
#15933=CARTESIAN_POINT('Ctrl Pts',(-3.00094714494784,5.10192391423162,10.5222111210216));
#15934=CARTESIAN_POINT('Ctrl Pts',(-3.14250264405843,5.01597233617464,10.5299995308672));
#15935=CARTESIAN_POINT('Ctrl Pts',(-3.28019212727181,4.92425326020951,10.5377879407128));
#15936=CARTESIAN_POINT('Ctrl Pts',(-3.41064575843563,4.83735420134605,10.545167054365));
#15937=CARTESIAN_POINT('Ctrl Pts',(-3.5376290395649,4.74527838396932,10.5525461680173));
#15938=CARTESIAN_POINT('Ctrl Pts',(-3.66073769636084,4.64832551366002,10.5599252816695));
#15939=CARTESIAN_POINT('Ctrl Pts',(-3.79066982340934,4.54599889430925,10.5677133930625));
#15940=CARTESIAN_POINT('Ctrl Pts',(-3.91633203875168,4.4382027106867,10.5755015044555));
#15941=CARTESIAN_POINT('Ctrl Pts',(-4.03727127483512,4.32531746995422,10.5832896158485));
#15942=CARTESIAN_POINT('Ctrl Pts',(-4.15818676660779,4.21245439227093,10.5910761981816));
#15943=CARTESIAN_POINT('Ctrl Pts',(-4.27438089586976,4.09450446896867,10.5988627805146));
#15944=CARTESIAN_POINT('Ctrl Pts',(-4.38543580176644,3.97188662867977,10.6066493628477));
#15945=CARTESIAN_POINT('Ctrl Pts',(-4.49649494216205,3.84926411299981,10.6144362420815));
#15946=CARTESIAN_POINT('Ctrl Pts',(-4.60241424966546,3.72197355835321,10.6222231213152));
#15947=CARTESIAN_POINT('Ctrl Pts',(-4.70281417979792,3.59046923852463,10.6300100005489));
#15948=CARTESIAN_POINT('Ctrl Pts',(-4.80320748359333,3.45897359790473,10.6377963658532));
#15949=CARTESIAN_POINT('Ctrl Pts',(-4.89808194516815,3.32326500269818,10.6455827311574));
#15950=CARTESIAN_POINT('Ctrl Pts',(-4.98709953674678,3.18382926255163,10.6533690964616));
#15951=CARTESIAN_POINT('Ctrl Pts',(-5.07614050253693,3.04435690941179,10.6611575063072));
#15952=CARTESIAN_POINT('Ctrl Pts',(-5.15932135160683,2.90115572419639,10.6689459161529));
#15953=CARTESIAN_POINT('Ctrl Pts',(-5.23634798948701,2.75473960575139,10.6767343259985));
#15954=CARTESIAN_POINT('Ctrl Pts',(-5.3093267266648,2.6160179411344,10.6841134396506));
#15955=CARTESIAN_POINT('Ctrl Pts',(-5.37678132643697,2.47441078453376,10.6914925533026));
#15956=CARTESIAN_POINT('Ctrl Pts',(-5.43850017603216,2.33037473334186,10.6988716669547));
#15957=CARTESIAN_POINT('Ctrl Pts',(-5.50338173111395,2.17895773431376,10.7066289140845));
#15958=CARTESIAN_POINT('Ctrl Pts',(-5.56194908421775,2.02479825938375,10.7143861612142));
#15959=CARTESIAN_POINT('Ctrl Pts',(-5.6139872295826,1.86844265327665,10.7221434083439));
#15960=CARTESIAN_POINT('Ctrl Pts',(-5.66601947511043,1.71210477402332,10.7298997759939));
#15961=CARTESIAN_POINT('Ctrl Pts',(-5.71152388362962,1.55357156700543,10.7376561436439));
#15962=CARTESIAN_POINT('Ctrl Pts',(-5.75033467496015,1.39340650509854,10.7454125112939));
#15963=CARTESIAN_POINT('Ctrl Pts',(-5.78914022576506,1.23326306988571,10.7531678316207));
#15964=CARTESIAN_POINT('Ctrl Pts',(-5.82125388798296,1.07148853527656,10.7609231519475));
#15965=CARTESIAN_POINT('Ctrl Pts',(-5.84656050553762,0.908658801524338,
10.7686784722742));
#15966=CARTESIAN_POINT('Ctrl Pts',(-5.8718711620906,0.745803079746681,10.7764350303692));
#15967=CARTESIAN_POINT('Ctrl Pts',(-5.89037255084516,0.581892142820665,
10.7841915884641));
#15968=CARTESIAN_POINT('Ctrl Pts',(-5.90200100937398,0.417510057182556,
10.791948146559));
#15969=CARTESIAN_POINT('Ctrl Pts',(-5.91183394626391,0.278509804491384,
10.798507033624));
#15970=CARTESIAN_POINT('Ctrl Pts',(-5.91675342831919,0.139172905666653,
10.805065920689));
#15971=CARTESIAN_POINT('Ctrl Pts',(-5.91674999820671,-0.000145674166803196,
10.811624807754));
#15972=CARTESIAN_POINT('Origin',(0.,0.,0.));
#15973=CARTESIAN_POINT('',(-5.91650109564654,0.000137871390016447,12.8133751922049));
#15974=CARTESIAN_POINT('',(-5.91674999943461,8.17956336808546E-5,12.5616248077579));
#15975=CARTESIAN_POINT('',(-5.91675,-7.2459289488551E-16,0.));
#15976=CARTESIAN_POINT('Ctrl Pts',(-5.91650109564654,0.000137871390016447,
12.8133751922049));
#15977=CARTESIAN_POINT('Ctrl Pts',(-5.91676819625198,0.31131399389983,12.7987285699419));
#15978=CARTESIAN_POINT('Ctrl Pts',(-5.81632669523957,1.60683994088276,12.7377419491744));
#15979=CARTESIAN_POINT('Ctrl Pts',(-4.8844629651232,3.76663245314218,12.6304153299036));
#15980=CARTESIAN_POINT('Ctrl Pts',(-2.48557677379138,5.64512237212916,12.4913953343907));
#15981=CARTESIAN_POINT('Ctrl Pts',(0.519808293086261,6.14616122739744,12.3523753388782));
#15982=CARTESIAN_POINT('Ctrl Pts',(3.39835634226172,5.14749188107496,12.2133553433657));
#15983=CARTESIAN_POINT('Ctrl Pts',(5.44768063861793,2.89279694315932,12.0743353478532));
#15984=CARTESIAN_POINT('Ctrl Pts',(6.16773109540022,-0.0677615640123341,
11.9353153523407));
#15985=CARTESIAN_POINT('Ctrl Pts',(5.38281014535615,-3.01178575495921,11.7962953568282));
#15986=CARTESIAN_POINT('Ctrl Pts',(3.28444422959756,-5.22091223804679,11.6572753613157));
#15987=CARTESIAN_POINT('Ctrl Pts',(0.384649947977164,-6.15609802652996,
11.5182553658031));
#15988=CARTESIAN_POINT('Ctrl Pts',(-2.60900172858952,-5.58915096190302,
11.3792353702907));
#15989=CARTESIAN_POINT('Ctrl Pts',(-4.96603793973493,-3.65841026619979,
11.2402153747781));
#15990=CARTESIAN_POINT('Ctrl Pts',(-5.83342026961988,-1.52009487709728,
11.1349286487496));
#15991=CARTESIAN_POINT('Ctrl Pts',(-5.91688460612658,-0.267972750171078,
11.0759819212251));
#15992=CARTESIAN_POINT('Ctrl Pts',(-5.91662392833365,-0.000151321579282548,
11.0633751922049));
#15993=CARTESIAN_POINT('Ctrl Pts',(-5.91674999820668,-0.000145675039010474,
10.8116248077951));
#15994=CARTESIAN_POINT('Ctrl Pts',(-5.9167454320706,-0.185604253661456,
10.8203558892767));
#15995=CARTESIAN_POINT('Ctrl Pts',(-5.90801584367932,-0.371021786546643,
10.8290869707582));
#15996=CARTESIAN_POINT('Ctrl Pts',(-5.89060459663212,-0.555615018368427,
10.8378180522397));
#15997=CARTESIAN_POINT('Ctrl Pts',(-5.87507379076582,-0.720271900203724,
10.8456061636326));
#15998=CARTESIAN_POINT('Ctrl Pts',(-5.85263204077725,-0.88430658380832,
10.8533942750255));
#15999=CARTESIAN_POINT('Ctrl Pts',(-5.82335341479904,-1.04713206848436,
10.8611823864184));
#16000=CARTESIAN_POINT('Ctrl Pts',(-5.79408053716864,-1.20992558521501,
10.8689689687514));
#16001=CARTESIAN_POINT('Ctrl Pts',(-5.75797351835347,-1.37151006242046,
10.8767555510844));
#16002=CARTESIAN_POINT('Ctrl Pts',(-5.71515779917155,-1.53130724972769,
10.8845421334174));
#16003=CARTESIAN_POINT('Ctrl Pts',(-5.67234044743583,-1.69111053006599,
10.892329012651));
#16004=CARTESIAN_POINT('Ctrl Pts',(-5.6228139623546,-1.84912607448866,10.9001158918847));
#16005=CARTESIAN_POINT('Ctrl Pts',(-5.5667542586208,-2.00478866383146,10.9079027711184));
#16006=CARTESIAN_POINT('Ctrl Pts',(-5.51069825479507,-2.1604409795333,10.9156891364225));
#16007=CARTESIAN_POINT('Ctrl Pts',(-5.44811000357761,-2.31374035031104,
10.9234755017267));
#16008=CARTESIAN_POINT('Ctrl Pts',(-5.3792144279962,-2.4641393426788,10.9312618670308));
#16009=CARTESIAN_POINT('Ctrl Pts',(-5.31030076183565,-2.61457782676791,
10.9390502768764));
#16010=CARTESIAN_POINT('Ctrl Pts',(-5.23507659332383,-2.76211411915151,
10.946838686722));
#16011=CARTESIAN_POINT('Ctrl Pts',(-5.15381426804612,-2.90622247135079,
10.9546270965675));
#16012=CARTESIAN_POINT('Ctrl Pts',(-5.07682243713573,-3.04275764736727,
10.96200621022));
#16013=CARTESIAN_POINT('Ctrl Pts',(-4.9944108880427,-3.17621567975814,10.9693853238725));
#16014=CARTESIAN_POINT('Ctrl Pts',(-4.90684854034149,-3.30617119409273,
10.976764437525));
#16015=CARTESIAN_POINT('Ctrl Pts',(-4.81443292650969,-3.44332967537331,
10.984552548918));
#16016=CARTESIAN_POINT('Ctrl Pts',(-4.71624633646594,-3.57663535081104,
10.992340660311));
#16017=CARTESIAN_POINT('Ctrl Pts',(-4.61263465296196,-3.70560819850055,
11.000128771704));
#16018=CARTESIAN_POINT('Ctrl Pts',(-4.50904331180559,-3.83455572462002,
11.0079153540371));
#16019=CARTESIAN_POINT('Ctrl Pts',(-4.40002920241936,-3.95917187139405,
11.0157019363702));
#16020=CARTESIAN_POINT('Ctrl Pts',(-4.28597913261866,-4.07900887928151,
11.0234885187033));
#16021=CARTESIAN_POINT('Ctrl Pts',(-4.17192471411444,-4.19885045652714,
11.031275397937));
#16022=CARTESIAN_POINT('Ctrl Pts',(-4.05283416837771,-4.31391229607584,
11.0390622771707));
#16023=CARTESIAN_POINT('Ctrl Pts',(-3.92913239089576,-4.42378222987002,
11.0468491564044));
#16024=CARTESIAN_POINT('Ctrl Pts',(-3.80543877765967,-4.53364491231204,
11.0546355217086));
#16025=CARTESIAN_POINT('Ctrl Pts',(-3.67713478070579,-4.638316162603,11.0624218870128));
#16026=CARTESIAN_POINT('Ctrl Pts',(-3.54467982156324,-4.73742287801104,
11.070208252317));
#16027=CARTESIAN_POINT('Ctrl Pts',(-3.41219008243807,-4.83655561683007,
11.0779966621626));
#16028=CARTESIAN_POINT('Ctrl Pts',(-3.27554745800553,-4.9301207080088,11.0857850720082));
#16029=CARTESIAN_POINT('Ctrl Pts',(-3.13524263775297,-5.01778677953894,
11.0935734818538));
#16030=CARTESIAN_POINT('Ctrl Pts',(-3.00231111063719,-5.10084582728774,
11.1009525955059));
#16031=CARTESIAN_POINT('Ctrl Pts',(-2.86609261929444,-5.17860978068094,
11.108331709158));
#16032=CARTESIAN_POINT('Ctrl Pts',(-2.72702682226942,-5.25083376932875,
11.1157108228101));
#16033=CARTESIAN_POINT('Ctrl Pts',(-2.5802531080747,-5.32706087401279,11.123498934203));
#16034=CARTESIAN_POINT('Ctrl Pts',(-2.43025508611663,-5.39714370341423,
11.131287045596));
#16035=CARTESIAN_POINT('Ctrl Pts',(-2.27756614334164,-5.46082622184628,
11.139075156989));
#16036=CARTESIAN_POINT('Ctrl Pts',(-2.12490717837867,-5.52449623732604,
11.146861739322));
#16037=CARTESIAN_POINT('Ctrl Pts',(-1.96955864146968,-5.58176832618418,
11.1546483216551));
#16038=CARTESIAN_POINT('Ctrl Pts',(-1.81207442134101,-5.63243436304602,
11.1624349039882));
#16039=CARTESIAN_POINT('Ctrl Pts',(-1.65458419637423,-5.68310233179252,
11.1702217832219));
#16040=CARTESIAN_POINT('Ctrl Pts',(-1.494958428193,-5.72716364290202,11.1780086624556));
#16041=CARTESIAN_POINT('Ctrl Pts',(-1.33376742295693,-5.76445964717933,
11.1857955416893));
#16042=CARTESIAN_POINT('Ctrl Pts',(-1.17258705623392,-5.80175318994194,
11.1935819069935));
#16043=CARTESIAN_POINT('Ctrl Pts',(-1.00984197053972,-5.83228224748056,
11.2013682722977));
#16044=CARTESIAN_POINT('Ctrl Pts',(-0.846114099909923,-5.85593899323017,
11.2091546376019));
#16045=CARTESIAN_POINT('Ctrl Pts',(-0.68234323766618,-5.87960195076082,
11.2169430474475));
#16046=CARTESIAN_POINT('Ctrl Pts',(-0.517589391005335,-5.89638894303135,
11.2247314572931));
#16047=CARTESIAN_POINT('Ctrl Pts',(-0.352441985621134,-5.90624374787152,
11.2325198671388));
#16048=CARTESIAN_POINT('Ctrl Pts',(-0.195973399883253,-5.9155806634136,
11.2398989807909));
#16049=CARTESIAN_POINT('Ctrl Pts',(-0.0391518156922628,-5.91869523613666,
11.2472780944431));
#16050=CARTESIAN_POINT('Ctrl Pts',(0.11751953811834,-5.91558278791367,11.2546572080952));
#16051=CARTESIAN_POINT('Ctrl Pts',(0.282874621815559,-5.91229782787536,
11.2624453194882));
#16052=CARTESIAN_POINT('Ctrl Pts',(0.448121405794196,-5.90207481692401,
11.2702334308812));
#16053=CARTESIAN_POINT('Ctrl Pts',(0.612669014299875,-5.88494411540304,
11.2780215422741));
#16054=CARTESIAN_POINT('Ctrl Pts',(0.777184316751264,-5.86781677719666,
11.2858081246072));
#16055=CARTESIAN_POINT('Ctrl Pts',(0.941000400011421,-5.84378448751827,
11.2935947069402));
#16056=CARTESIAN_POINT('Ctrl Pts',(1.1035313072279,-5.81292948662444,11.3013812892733));
#16057=CARTESIAN_POINT('Ctrl Pts',(1.26606841171148,-5.78207330923634,11.309168168507));
#16058=CARTESIAN_POINT('Ctrl Pts',(1.42731992744971,-5.74439395578933,11.3169550477407));
#16059=CARTESIAN_POINT('Ctrl Pts',(1.58670915221621,-5.70002496738157,11.3247419269744));
#16060=CARTESIAN_POINT('Ctrl Pts',(1.7460878573861,-5.65565890730139,11.3325282922786));
#16061=CARTESIAN_POINT('Ctrl Pts',(1.90360420972952,-5.60460418160287,11.3403146575828));
#16062=CARTESIAN_POINT('Ctrl Pts',(2.05869561165523,-5.54704452308177,11.3481010228869));
#16063=CARTESIAN_POINT('Ctrl Pts',(2.21382773743365,-5.48946975056321,11.3558894327325));
#16064=CARTESIAN_POINT('Ctrl Pts',(2.36653334001421,-5.42538674158669,11.3636778425781));
#16065=CARTESIAN_POINT('Ctrl Pts',(2.51626793257187,-5.35502812821842,11.3714662524237));
#16066=CARTESIAN_POINT('Ctrl Pts',(2.65813367898902,-5.2883669978018,11.3788453660759));
#16067=CARTESIAN_POINT('Ctrl Pts',(2.7973324131779,-5.21607299921343,11.3862244797281));
#16068=CARTESIAN_POINT('Ctrl Pts',(2.93342000023192,-5.13838278690284,11.3936035933803));
#16069=CARTESIAN_POINT('Ctrl Pts',(3.07705043298201,-5.05638648543129,11.4013917047733));
#16070=CARTESIAN_POINT('Ctrl Pts',(3.21726635705876,-4.96834953748601,11.4091798161662));
#16071=CARTESIAN_POINT('Ctrl Pts',(3.35356343643352,-4.87458129897494,11.4169679275592));
#16072=CARTESIAN_POINT('Ctrl Pts',(3.48983375625269,-4.78083147022292,11.4247545098922));
#16073=CARTESIAN_POINT('Ctrl Pts',(3.62218650346077,-4.68135277708563,11.4325410922253));
#16074=CARTESIAN_POINT('Ctrl Pts',(3.75014648260913,-4.57649777903086,11.4403276745584));
#16075=CARTESIAN_POINT('Ctrl Pts',(3.87811134084303,-4.47163878287834,11.4481145537921));
#16076=CARTESIAN_POINT('Ctrl Pts',(4.00168284621691,-4.36140327106968,11.4559014330258));
#16077=CARTESIAN_POINT('Ctrl Pts',(4.12041847411225,-4.24618442377324,11.4636883122595));
#16078=CARTESIAN_POINT('Ctrl Pts',(4.23914626552484,-4.13097318085406,11.4714746775637));
#16079=CARTESIAN_POINT('Ctrl Pts',(4.35303858891042,-4.01077948324227,11.4792610428679));
#16080=CARTESIAN_POINT('Ctrl Pts',(4.46168931873055,-3.88603383742676,11.487047408172));
#16081=CARTESIAN_POINT('Ctrl Pts',(4.57036857802595,-3.76125543593788,11.4948358180176));
#16082=CARTESIAN_POINT('Ctrl Pts',(4.67380328208609,-3.63192293772112,11.5026242278632));
#16083=CARTESIAN_POINT('Ctrl Pts',(4.77162660398512,-3.49850112400174,11.5104126377088));
#16084=CARTESIAN_POINT('Ctrl Pts',(4.864309118701,-3.37209088794138,11.517791751361));
#16085=CARTESIAN_POINT('Ctrl Pts',(4.95195470633137,-3.24201029445954,11.5251708650132));
#16086=CARTESIAN_POINT('Ctrl Pts',(5.0342865857107,-3.10867964503152,11.5325499786654));
#16087=CARTESIAN_POINT('Ctrl Pts',(5.12118182516919,-2.96795895704839,11.5403380900584));
#16088=CARTESIAN_POINT('Ctrl Pts',(5.20218864833156,-2.82356746086751,11.5481262014514));
#16089=CARTESIAN_POINT('Ctrl Pts',(5.27701219299427,-2.676018101114,11.5559143128443));
#16090=CARTESIAN_POINT('Ctrl Pts',(5.35182104735834,-2.52849771010514,11.5637008951774));
#16091=CARTESIAN_POINT('Ctrl Pts',(5.4204489010451,-2.377820977395,11.5714874775105));
#16092=CARTESIAN_POINT('Ctrl Pts',(5.482647150966,-2.22452484375976,11.5792740598435));
#16093=CARTESIAN_POINT('Ctrl Pts',(5.54484777249233,-2.07122286497706,11.5870609390773));
#16094=CARTESIAN_POINT('Ctrl Pts',(5.60061817590153,-1.9153015800039,11.594847818311));
#16095=CARTESIAN_POINT('Ctrl Pts',(5.6497578814823,-1.75731796870364,11.6026346975447));
#16096=CARTESIAN_POINT('Ctrl Pts',(5.69889434387092,-1.59934478423033,11.6104210628489));
#16097=CARTESIAN_POINT('Ctrl Pts',(5.74140088938333,-1.43930985098022,11.6182074281531));
#16098=CARTESIAN_POINT('Ctrl Pts',(5.77712685939935,-1.27778551130722,11.6259937934573));
#16099=CARTESIAN_POINT('Ctrl Pts',(5.8128622103296,-1.11621875862271,11.6337822033029));
#16100=CARTESIAN_POINT('Ctrl Pts',(5.84181335712389,-0.953162129814492,
11.6415706131485));
#16101=CARTESIAN_POINT('Ctrl Pts',(5.86388054841331,-0.789199262822796,
11.6493590229941));
#16102=CARTESIAN_POINT('Ctrl Pts',(5.88478806557499,-0.633852965663927,
11.6567381366462));
#16103=CARTESIAN_POINT('Ctrl Pts',(5.89951651366658,-0.477693487410386,
11.6641172502984));
#16104=CARTESIAN_POINT('Ctrl Pts',(5.90802393187583,-0.321222326251578,
11.6714963639506));
#16105=CARTESIAN_POINT('Ctrl Pts',(5.91700288569104,-0.156078531165855,
11.6792844753436));
#16106=CARTESIAN_POINT('Ctrl Pts',(5.91905484265651,0.00947145838644853,
11.6870725867365));
#16107=CARTESIAN_POINT('Ctrl Pts',(5.91416628833766,0.174836141545134,11.6948606981295));
#16108=CARTESIAN_POINT('Ctrl Pts',(5.90927869380122,0.340168358230971,11.7026472804625));
#16109=CARTESIAN_POINT('Ctrl Pts',(5.89745331630517,0.505315021923757,11.7104338627956));
#16110=CARTESIAN_POINT('Ctrl Pts',(5.87872874320458,0.669685692187242,11.7182204451286));
#16111=CARTESIAN_POINT('Ctrl Pts',(5.86000345614018,0.834062629867812,11.7260073243623));
#16112=CARTESIAN_POINT('Ctrl Pts',(5.83437847931976,0.997663197003097,11.733794203596));
#16113=CARTESIAN_POINT('Ctrl Pts',(5.80194424574037,1.15990238029765,11.7415810828297));
#16114=CARTESIAN_POINT('Ctrl Pts',(5.76951215280164,1.32213085589998,11.7493674481339));
#16115=CARTESIAN_POINT('Ctrl Pts',(5.73027176519635,1.48299781413655,11.7571538134381));
#16116=CARTESIAN_POINT('Ctrl Pts',(5.68436461491616,1.64192858772515,11.7649401787423));
#16117=CARTESIAN_POINT('Ctrl Pts',(5.63844541035054,1.80090109330747,11.7727285885878));
#16118=CARTESIAN_POINT('Ctrl Pts',(5.58585603199734,1.95793609062769,11.7805169984334));
#16119=CARTESIAN_POINT('Ctrl Pts',(5.52678811887441,2.1124733493156,11.788305408279));
#16120=CARTESIAN_POINT('Ctrl Pts',(5.47082434028861,2.25888937235113,11.7956845219312));
#16121=CARTESIAN_POINT('Ctrl Pts',(5.40904552559427,2.40306318372778,11.8030636355835));
#16122=CARTESIAN_POINT('Ctrl Pts',(5.34165476246286,2.54453433090572,11.8104427492357));
#16123=CARTESIAN_POINT('Ctrl Pts',(5.27052877161072,2.6938467151623,11.8182308606287));
#16124=CARTESIAN_POINT('Ctrl Pts',(5.19312568894896,2.8402016684873,11.8260189720216));
#16125=CARTESIAN_POINT('Ctrl Pts',(5.10971664201412,2.98307331469141,11.8338070834146));
#16126=CARTESIAN_POINT('Ctrl Pts',(5.02632397099162,3.12591691053838,11.8415936657477));
#16127=CARTESIAN_POINT('Ctrl Pts',(4.93692784948212,3.26527828804663,11.8493802480808));
#16128=CARTESIAN_POINT('Ctrl Pts',(4.84184464944875,3.40065742954278,11.8571668304138));
#16129=CARTESIAN_POINT('Ctrl Pts',(4.74675782391412,3.53604173301549,11.8649537096476));
#16130=CARTESIAN_POINT('Ctrl Pts',(4.6459836663555,3.66744323290245,11.8727405888813));
#16131=CARTESIAN_POINT('Ctrl Pts',(4.5398814790422,3.79439148200995,11.880527468115));
#16132=CARTESIAN_POINT('Ctrl Pts',(4.43378629441189,3.92133135260641,11.8883138334192));
#16133=CARTESIAN_POINT('Ctrl Pts',(4.32236398874528,4.04381831547097,11.8961001987234));
#16134=CARTESIAN_POINT('Ctrl Pts',(4.20601378560764,4.16141545604119,11.9038865640276));
#16135=CARTESIAN_POINT('Ctrl Pts',(4.08963303126935,4.2790434752325,11.9116749738732));
#16136=CARTESIAN_POINT('Ctrl Pts',(3.9683220173478,4.39177887783712,11.9194633837188));
#16137=CARTESIAN_POINT('Ctrl Pts',(3.84251706040394,4.49922139964291,11.9272517935644));
#16138=CARTESIAN_POINT('Ctrl Pts',(3.72332340037689,4.60101760646711,11.9346309072166));
#16139=CARTESIAN_POINT('Ctrl Pts',(3.60009617753248,4.69806275771776,11.9420100208687));
#16140=CARTESIAN_POINT('Ctrl Pts',(3.47323402452313,4.79004968381277,11.9493891345208));
#16141=CARTESIAN_POINT('Ctrl Pts',(3.33934035845881,4.88713511451598,11.9571772459138));
#16142=CARTESIAN_POINT('Ctrl Pts',(3.20134957404015,4.97862037553502,11.9649653573067));
#16143=CARTESIAN_POINT('Ctrl Pts',(3.05975135225921,5.06417339995857,11.9727534686997));
#16144=CARTESIAN_POINT('Ctrl Pts',(2.91818093082082,5.1497096275371,11.9805400510327));
#16145=CARTESIAN_POINT('Ctrl Pts',(2.7730047585213,5.22931577728854,11.9883266333658));
#16146=CARTESIAN_POINT('Ctrl Pts',(2.62473987489058,5.30270413578387,11.9961132156988));
#16147=CARTESIAN_POINT('Ctrl Pts',(2.47646933795271,5.37609529256104,12.0039000949326));
#16148=CARTESIAN_POINT('Ctrl Pts',(2.32511013862664,5.44326803839932,12.0116869741663));
#16149=CARTESIAN_POINT('Ctrl Pts',(2.17120286696385,5.5039811657552,12.0194738534));
#16150=CARTESIAN_POINT('Ctrl Pts',(2.01730575309196,5.56469028607979,12.0272602187042));
#16151=CARTESIAN_POINT('Ctrl Pts',(1.86086120072366,5.61894052392279,12.0350465840083));
#16152=CARTESIAN_POINT('Ctrl Pts',(1.70242881251837,5.66653921726545,12.0428329493125));
#16153=CARTESIAN_POINT('Ctrl Pts',(1.54395482318527,5.71415040905838,12.0506213591581));
#16154=CARTESIAN_POINT('Ctrl Pts',(1.38349226067852,5.75510647250128,12.0584097690037));
#16155=CARTESIAN_POINT('Ctrl Pts',(1.22161576504376,5.78926467568175,12.0661981788493));
#16156=CARTESIAN_POINT('Ctrl Pts',(1.06824619633969,5.82162779837571,12.0735772925015));
#16157=CARTESIAN_POINT('Ctrl Pts',(0.913607736579875,5.84788911203013,12.0809564061537));
#16158=CARTESIAN_POINT('Ctrl Pts',(0.758197394955816,5.86796960394157,12.0883355198059));
#16159=CARTESIAN_POINT('Ctrl Pts',(0.594173216818297,5.88916308532738,12.0961236311989));
#16160=CARTESIAN_POINT('Ctrl Pts',(0.429230584190746,5.90347872398087,12.1039117425918));
#16161=CARTESIAN_POINT('Ctrl Pts',(0.263958369650268,5.91085920502185,12.1116998539848));
#16162=CARTESIAN_POINT('Ctrl Pts',(0.0987186034279958,5.91823823703405,
12.1194864363179));
#16163=CARTESIAN_POINT('Ctrl Pts',(-0.0668502965829588,5.91868481397916,
12.1272730186509));
#16164=CARTESIAN_POINT('Ctrl Pts',(-0.232156653918887,5.91219365807153,
12.135059600984));
#16165=CARTESIAN_POINT('Ctrl Pts',(-0.397469314349455,5.90570225465757,
12.1428464802177));
#16166=CARTESIAN_POINT('Ctrl Pts',(-0.562519092648928,5.89227259764935,
12.1506333594514));
#16167=CARTESIAN_POINT('Ctrl Pts',(-0.726715882158628,5.87195151454084,
12.1584202386851));
#16168=CARTESIAN_POINT('Ctrl Pts',(-0.890901834775293,5.85163177261204,
12.1662066039893));
#16169=CARTESIAN_POINT('Ctrl Pts',(-1.05423459414129,5.82442155413361,12.1739929692935));
#16170=CARTESIAN_POINT('Ctrl Pts',(-1.21613058408384,5.79041941183503,12.1817793345977));
#16171=CARTESIAN_POINT('Ctrl Pts',(-1.3780690846256,5.75640834126439,12.1895677444433));
#16172=CARTESIAN_POINT('Ctrl Pts',(-1.53856974857601,5.71560184704553,12.1973561542889));
#16173=CARTESIAN_POINT('Ctrl Pts',(-1.69705968341381,5.66814952108988,12.2051445641345));
#16174=CARTESIAN_POINT('Ctrl Pts',(-1.84722066172463,5.62319090781317,12.2125236777867));
#16175=CARTESIAN_POINT('Ctrl Pts',(-1.99557656161878,5.57226707450899,12.2199027914389));
#16176=CARTESIAN_POINT('Ctrl Pts',(-2.1416531455166,5.51554642504248,12.2272819050911));
#16177=CARTESIAN_POINT('Ctrl Pts',(-2.2958262292934,5.45568195389499,12.2350700164841));
#16178=CARTESIAN_POINT('Ctrl Pts',(-2.44751522642145,5.389338471031,12.2428581278771));
#16179=CARTESIAN_POINT('Ctrl Pts',(-2.59617561298909,5.31674738435265,12.25064623927));
#16180=CARTESIAN_POINT('Ctrl Pts',(-2.74480681268132,5.24417054966874,12.2584328216031));
#16181=CARTESIAN_POINT('Ctrl Pts',(-2.89041030129804,5.16534869873573,12.2662194039361));
#16182=CARTESIAN_POINT('Ctrl Pts',(-3.0324639891518,5.08056027589454,12.2740059862692));
#16183=CARTESIAN_POINT('Ctrl Pts',(-3.17452309348098,4.9957686200897,12.2817928655029));
#16184=CARTESIAN_POINT('Ctrl Pts',(-3.31303184982197,4.90501009750941,12.2895797447366));
#16185=CARTESIAN_POINT('Ctrl Pts',(-3.44749447597213,4.80860815627991,12.2973666239703));
#16186=CARTESIAN_POINT('Ctrl Pts',(-3.58194822766667,4.71221257752282,12.3051529892745));
#16187=CARTESIAN_POINT('Ctrl Pts',(-3.71235612392713,4.61017451175995,12.3129393545787));
#16188=CARTESIAN_POINT('Ctrl Pts',(-3.83825286429633,4.50285970381279,12.3207257198829));
#16189=CARTESIAN_POINT('Ctrl Pts',(-3.96418266259308,4.39551671717622,12.3285141297285));
#16190=CARTESIAN_POINT('Ctrl Pts',(-4.08559869345287,4.28289442564719,12.336302539574));
#16191=CARTESIAN_POINT('Ctrl Pts',(-4.20206945692127,4.16539828128228,12.3440909494196));
#16192=CARTESIAN_POINT('Ctrl Pts',(-4.31241945362519,4.0540767894565,12.3514700630718));
#16193=CARTESIAN_POINT('Ctrl Pts',(-4.41833039815079,3.93838071492787,12.358849176724));
#16194=CARTESIAN_POINT('Ctrl Pts',(-4.51946642200182,3.81868482895592,12.3662282903762));
#16195=CARTESIAN_POINT('Ctrl Pts',(-4.62620805205678,3.69235463034798,12.3740164017692));
#16196=CARTESIAN_POINT('Ctrl Pts',(-4.72766856124315,3.56152353830952,12.3818045131622));
#16197=CARTESIAN_POINT('Ctrl Pts',(-4.82348050438523,3.42665527684294,12.3895926245551));
#16198=CARTESIAN_POINT('Ctrl Pts',(-4.91927363652244,3.29181349440852,12.3973792068882));
#16199=CARTESIAN_POINT('Ctrl Pts',(-5.00942023045605,3.15293638440082,12.4051657892213));
#16200=CARTESIAN_POINT('Ctrl Pts',(-5.0935950449057,3.01051824126879,12.4129523715543));
#16201=CARTESIAN_POINT('Ctrl Pts',(-5.17777306892231,2.86809466776462,12.4207392507881));
#16202=CARTESIAN_POINT('Ctrl Pts',(-5.2559786918491,2.72213006401831,12.4285261300218));
#16203=CARTESIAN_POINT('Ctrl Pts',(-5.32793130500654,2.57314565690154,12.4363130092555));
#16204=CARTESIAN_POINT('Ctrl Pts',(-5.39987916933312,2.42417108266951,12.4440993745597));
#16205=CARTESIAN_POINT('Ctrl Pts',(-5.46557471089158,2.27217739171107,12.4518857398639));
#16206=CARTESIAN_POINT('Ctrl Pts',(-5.52478432394942,2.1177083690496,12.4596721051681));
#16207=CARTESIAN_POINT('Ctrl Pts',(-5.58400948424929,1.96319878595958,12.4674605150137));
#16208=CARTESIAN_POINT('Ctrl Pts',(-5.63674519670071,1.80621287024954,12.4752489248593));
#16209=CARTESIAN_POINT('Ctrl Pts',(-5.68280653390567,1.64731310341993,12.4830373347049));
#16210=CARTESIAN_POINT('Ctrl Pts',(-5.72644725761465,1.49676383059325,12.4904164483571));
#16211=CARTESIAN_POINT('Ctrl Pts',(-5.76409699364876,1.34449693593846,12.4977955620092));
#16212=CARTESIAN_POINT('Ctrl Pts',(-5.79564011200116,1.19100220598584,12.5051746756613));
#16213=CARTESIAN_POINT('Ctrl Pts',(-5.82972444891384,1.02514142990224,12.51314827526));
#16214=CARTESIAN_POINT('Ctrl Pts',(-5.85668801831256,0.857799885178385,
12.5211218748587));
#16215=CARTESIAN_POINT('Ctrl Pts',(-5.87642730860905,0.689588753630612,
12.5290954744574));
#16216=CARTESIAN_POINT('Ctrl Pts',(-5.89616094744817,0.521425781769642,
12.5370667911747));
#16217=CARTESIAN_POINT('Ctrl Pts',(-5.90867440354806,0.352394003831148,
12.5450381078921));
#16218=CARTESIAN_POINT('Ctrl Pts',(-5.91391586784887,0.18311108788216,12.5530094246094));
#16219=CARTESIAN_POINT('Ctrl Pts',(-5.91580418922297,0.122124209004174,
12.5558812189922));
#16220=CARTESIAN_POINT('Ctrl Pts',(-5.91674915582728,0.0611047797757011,
12.5587530133751));
#16221=CARTESIAN_POINT('Ctrl Pts',(-5.91674999943461,8.1795633684796E-5,
12.5616248077579));
#16222=CARTESIAN_POINT('Origin',(0.,0.,0.));
#16223=CARTESIAN_POINT('',(-5.91713904777553,-9.26149740448912E-5,14.5633751922049));
#16224=CARTESIAN_POINT('',(-5.9167499999999,1.1077521759692E-6,14.3116248077956));
#16225=CARTESIAN_POINT('',(-5.91675,-7.2459289488551E-16,0.));
#16226=CARTESIAN_POINT('Ctrl Pts',(-5.91713904777553,-9.26149740448912E-5,
14.5633751922049));
#16227=CARTESIAN_POINT('Ctrl Pts',(-5.9164724942665,0.8898205116778,14.5214752186586));
#16228=CARTESIAN_POINT('Ctrl Pts',(-5.48777132288459,2.76456885274308,14.4332352466081));
#16229=CARTESIAN_POINT('Ctrl Pts',(-3.58563248749387,5.01883832767618,14.2986552760536));
#16230=CARTESIAN_POINT('Ctrl Pts',(-0.74581831746291,6.12284684865313,14.159635280541));
#16231=CARTESIAN_POINT('Ctrl Pts',(2.27598096591196,5.73283604662921,14.0206152850285));
#16232=CARTESIAN_POINT('Ctrl Pts',(4.74242428074643,3.94397140406846,13.8815952895159));
#16233=CARTESIAN_POINT('Ctrl Pts',(6.05168145514075,1.19274895104965,13.7425752940035));
#16234=CARTESIAN_POINT('Ctrl Pts',(5.88428418200233,-1.8495129521476,13.6035552984909));
#16235=CARTESIAN_POINT('Ctrl Pts',(4.28107861784435,-4.44048019504202,13.4645353029784));
#16236=CARTESIAN_POINT('Ctrl Pts',(1.63325862245189,-5.94793785835978,13.3255153074659));
#16237=CARTESIAN_POINT('Ctrl Pts',(-1.41308839831272,-6.00405526900601,
13.1864953119534));
#16238=CARTESIAN_POINT('Ctrl Pts',(-4.11463153546355,-4.59513936916963,
13.0474753164408));
#16239=CARTESIAN_POINT('Ctrl Pts',(-5.63332781710766,-2.33154439788799,
12.9231019431914));
#16240=CARTESIAN_POINT('Ctrl Pts',(-5.91592312484681,-0.67320658652368,
12.845068568446));
#16241=CARTESIAN_POINT('Ctrl Pts',(-5.91650109564654,0.000137871390016447,
12.8133751922049));
#16242=CARTESIAN_POINT('Ctrl Pts',(-5.91674999943462,8.17948436890362E-5,
12.5616248077951));
#16243=CARTESIAN_POINT('Ctrl Pts',(-5.91675229657022,-0.166084878407706,
12.5694447550752));
#16244=CARTESIAN_POINT('Ctrl Pts',(-5.90975028468448,-0.332249809338274,
12.5772647023552));
#16245=CARTESIAN_POINT('Ctrl Pts',(-5.89577044899758,-0.497816608026388,
12.5850846496353));
#16246=CARTESIAN_POINT('Ctrl Pts',(-5.88179051581164,-0.663384561420722,
12.5929046514537));
#16247=CARTESIAN_POINT('Ctrl Pts',(-5.86083269146452,-0.828354061912414,
12.6007246532721));
#16248=CARTESIAN_POINT('Ctrl Pts',(-5.83297537516117,-0.992133476536006,
12.6085446550905));
#16249=CARTESIAN_POINT('Ctrl Pts',(-5.80511105887375,-1.15595404563694,
12.6163666219184));
#16250=CARTESIAN_POINT('Ctrl Pts',(-5.77034383978369,-1.31858362209411,
12.6241885887462));
#16251=CARTESIAN_POINT('Ctrl Pts',(-5.72880346599528,-1.47943955959696,
12.632010555574));
#16252=CARTESIAN_POINT('Ctrl Pts',(-5.70736491432772,-1.56245562355329,
12.6360473906981));
#16253=CARTESIAN_POINT('Ctrl Pts',(-5.68412317400547,-1.64499946397032,
12.6400842258223));
#16254=CARTESIAN_POINT('Ctrl Pts',(-5.65910133104918,-1.72699238198012,
12.6441210609464));
#16255=CARTESIAN_POINT('Ctrl Pts',(-5.61082764777827,-1.88517817834122,
12.6519091723394));
#16256=CARTESIAN_POINT('Ctrl Pts',(-5.5559086689182,-2.0413668953765,12.6596972837324));
#16257=CARTESIAN_POINT('Ctrl Pts',(-5.49453480994079,-2.19499835645699,
12.6674853951253));
#16258=CARTESIAN_POINT('Ctrl Pts',(-5.43317300065069,-2.34859965467829,
12.6752719774584));
#16259=CARTESIAN_POINT('Ctrl Pts',(-5.36535895835549,-2.49964440218507,
12.6830585597914));
#16260=CARTESIAN_POINT('Ctrl Pts',(-5.29133166826683,-2.64759130888749,
12.6908451421245));
#16261=CARTESIAN_POINT('Ctrl Pts',(-5.21730155553412,-2.79554385677244,
12.6986320213582));
#16262=CARTESIAN_POINT('Ctrl Pts',(-5.13705786039537,-2.94039803998609,
12.7064189005919));
#16263=CARTESIAN_POINT('Ctrl Pts',(-5.0508863977957,-3.08163546823151,12.7142057798256));
#16264=CARTESIAN_POINT('Ctrl Pts',(-4.96472062246255,-3.22286357488861,
12.7219921451298));
#16265=CARTESIAN_POINT('Ctrl Pts',(-4.87262802911266,-3.36047513153216,
12.729778510434));
#16266=CARTESIAN_POINT('Ctrl Pts',(-4.77493887214427,-3.49397901106827,
12.7375648757382));
#16267=CARTESIAN_POINT('Ctrl Pts',(-4.67722406398722,-3.62751794601184,
12.7453532855838));
#16268=CARTESIAN_POINT('Ctrl Pts',(-4.57390994300305,-3.75694678941308,
12.7531416954294));
#16269=CARTESIAN_POINT('Ctrl Pts',(-4.46536886666572,-3.88180517892288,
12.7609301052749));
#16270=CARTESIAN_POINT('Ctrl Pts',(-4.36253183650075,-4.00010201549067,
12.7683092189272));
#16271=CARTESIAN_POINT('Ctrl Pts',(-4.25500326494473,-4.11429621906942,
12.7756883325794));
#16272=CARTESIAN_POINT('Ctrl Pts',(-4.14313200053735,-4.22402506960167,
12.7830674462316));
#16273=CARTESIAN_POINT('Ctrl Pts',(-4.02506011413759,-4.3398357958275,12.7908555576246));
#16274=CARTESIAN_POINT('Ctrl Pts',(-3.90210831516608,-4.45071349736323,
12.7986436690175));
#16275=CARTESIAN_POINT('Ctrl Pts',(-3.77471182004837,-4.55625737180058,
12.8064317804105));
#16276=CARTESIAN_POINT('Ctrl Pts',(-3.64734033701145,-4.66178052453823,
12.8142183627436));
#16277=CARTESIAN_POINT('Ctrl Pts',(-3.51552614490619,-4.76197173593689,
12.8220049450766));
#16278=CARTESIAN_POINT('Ctrl Pts',(-3.379738074369,-4.85647002576568,12.8297915274097));
#16279=CARTESIAN_POINT('Ctrl Pts',(-3.24394482626307,-4.95097191879312,
12.8375784066434));
#16280=CARTESIAN_POINT('Ctrl Pts',(-3.10417765653071,-5.03978027014071,
12.8453652858771));
#16281=CARTESIAN_POINT('Ctrl Pts',(-2.96093556199778,-5.12257661340432,
12.8531521651108));
#16282=CARTESIAN_POINT('Ctrl Pts',(-2.81770292136031,-5.20536749215713,
12.860938530415));
#16283=CARTESIAN_POINT('Ctrl Pts',(-2.67099609159335,-5.28214699704896,
12.8687248957192));
#16284=CARTESIAN_POINT('Ctrl Pts',(-2.52134004914326,-5.35264186351808,
12.8765112610233));
#16285=CARTESIAN_POINT('Ctrl Pts',(-2.37164471005547,-5.42315524050759,
12.8842996708689));
#16286=CARTESIAN_POINT('Ctrl Pts',(-2.2189988992925,-5.48738054358563,12.8920880807145));
#16287=CARTESIAN_POINT('Ctrl Pts',(-2.06394984603373,-5.54509166701123,
12.8998764905601));
#16288=CARTESIAN_POINT('Ctrl Pts',(-1.91704892423512,-5.59976995785576,
12.9072556042123));
#16289=CARTESIAN_POINT('Ctrl Pts',(-1.76799109714567,-5.64860103418118,
12.9146347178645));
#16290=CARTESIAN_POINT('Ctrl Pts',(-1.61725623469744,-5.69143328466848,
12.9220138315167));
#16291=CARTESIAN_POINT('Ctrl Pts',(-1.45816668073688,-5.73663957281228,
12.9298019429097));
#16292=CARTESIAN_POINT('Ctrl Pts',(-1.29715209712433,-5.77517933711375,
12.9375900543026));
#16293=CARTESIAN_POINT('Ctrl Pts',(-1.13478641534345,-5.80690884671457,
12.9453781656956));
#16294=CARTESIAN_POINT('Ctrl Pts',(-0.972452611234238,-5.83863212677921,
12.9531647480287));
#16295=CARTESIAN_POINT('Ctrl Pts',(-0.808768551641325,-5.86354775875977,
12.9609513303617));
#16296=CARTESIAN_POINT('Ctrl Pts',(-0.644318633120283,-5.88156306278476,
12.9687379126948));
#16297=CARTESIAN_POINT('Ctrl Pts',(-0.479862444159993,-5.89957905372933,
12.9765247919285));
#16298=CARTESIAN_POINT('Ctrl Pts',(-0.31464065502396,-5.91069415151979,
12.9843116711622));
#16299=CARTESIAN_POINT('Ctrl Pts',(-0.149243811773383,-5.91486744121518,
12.992098550396));
#16300=CARTESIAN_POINT('Ctrl Pts',(0.0161421153806483,-5.91904045547584,
12.9998849157002));
#16301=CARTESIAN_POINT('Ctrl Pts',(0.181702754074313,-5.91627257053815,
13.0076712810043));
#16302=CARTESIAN_POINT('Ctrl Pts',(0.346846371104012,-5.90657499379733,
13.0154576463085));
#16303=CARTESIAN_POINT('Ctrl Pts',(0.512033351494504,-5.89687487066976,
13.0232460561541));
#16304=CARTESIAN_POINT('Ctrl Pts',(0.676802772111731,-5.88024143661172,
13.0310344659997));
#16305=CARTESIAN_POINT('Ctrl Pts',(0.840565921562127,-5.85673795674763,
13.0388228758453));
#16306=CARTESIAN_POINT('Ctrl Pts',(0.99572299672694,-5.8344696307894,13.0462019894975));
#16307=CARTESIAN_POINT('Ctrl Pts',(1.14997658604171,-5.8060347927389,13.0535811031497));
#16308=CARTESIAN_POINT('Ctrl Pts',(1.30283276856397,-5.77152989593366,13.0609602168018));
#16309=CARTESIAN_POINT('Ctrl Pts',(1.46416121974405,-5.73511251674843,13.0687483281948));
#16310=CARTESIAN_POINT('Ctrl Pts',(1.62399058331058,-5.69192010873466,13.0765364395878));
#16311=CARTESIAN_POINT('Ctrl Pts',(1.78174811101581,-5.64210104760554,13.0843245509807));
#16312=CARTESIAN_POINT('Ctrl Pts',(1.93947466578125,-5.5922917675804,13.0921111333138));
#16313=CARTESIAN_POINT('Ctrl Pts',(2.09512989180203,-5.53585852653935,13.0998977156469));
#16314=CARTESIAN_POINT('Ctrl Pts',(2.24815627580423,-5.47299953609189,13.10768429798));
#16315=CARTESIAN_POINT('Ctrl Pts',(2.40118849466776,-5.41013814884538,13.1154711772137));
#16316=CARTESIAN_POINT('Ctrl Pts',(2.55159137388544,-5.34085063967505,13.1232580564474));
#16317=CARTESIAN_POINT('Ctrl Pts',(2.69882676633028,-5.26538361829784,13.1310449356811));
#16318=CARTESIAN_POINT('Ctrl Pts',(2.84605244132441,-5.18992157770038,13.1388313009852));
#16319=CARTESIAN_POINT('Ctrl Pts',(2.99011076357107,-5.10828098691886,13.1466176662894));
#16320=CARTESIAN_POINT('Ctrl Pts',(3.13048748065006,-5.02075479345419,13.1544040315936));
#16321=CARTESIAN_POINT('Ctrl Pts',(3.27090105780461,-4.93320561738834,13.1621924414392));
#16322=CARTESIAN_POINT('Ctrl Pts',(3.40763082574729,-4.83976791805148,13.1699808512848));
#16323=CARTESIAN_POINT('Ctrl Pts',(3.5401900918317,-4.74077891028433,13.1777692611304));
#16324=CARTESIAN_POINT('Ctrl Pts',(3.66578310882499,-4.64699196877597,13.1851483747826));
#16325=CARTESIAN_POINT('Ctrl Pts',(3.78763247743074,-4.54822233173038,13.1925274884348));
#16326=CARTESIAN_POINT('Ctrl Pts',(3.90535062107284,-4.44479100622132,13.199906602087));
#16327=CARTESIAN_POINT('Ctrl Pts',(4.0295934582035,-4.33562685418967,13.20769471348));
#16328=CARTESIAN_POINT('Ctrl Pts',(4.14927849957738,-4.2212306110712,13.215482824873));
#16329=CARTESIAN_POINT('Ctrl Pts',(4.26397379005778,-4.10200659192551,13.2232709362659));
#16330=CARTESIAN_POINT('Ctrl Pts',(4.37864656211684,-3.9828059803381,13.231057518599));
#16331=CARTESIAN_POINT('Ctrl Pts',(4.4883313165885,-3.85877971409506,13.238844100932));
#16332=CARTESIAN_POINT('Ctrl Pts',(4.59263331976451,-3.73036858134539,13.246630683265));
#16333=CARTESIAN_POINT('Ctrl Pts',(4.69693929995296,-3.60195255230748,13.2544175624988));
#16334=CARTESIAN_POINT('Ctrl Pts',(4.79586191364239,-3.46915156772926,13.2622044417325));
#16335=CARTESIAN_POINT('Ctrl Pts',(4.8890465883415,-3.33243964979509,13.2699913209662));
#16336=CARTESIAN_POINT('Ctrl Pts',(4.98222511290619,-3.1957367547681,13.2777776862704));
#16337=CARTESIAN_POINT('Ctrl Pts',(5.06966627643691,-3.05512370703689,13.2855640515746));
#16338=CARTESIAN_POINT('Ctrl Pts',(5.15105865855979,-2.91110378698119,13.2933504168788));
#16339=CARTESIAN_POINT('Ctrl Pts',(5.23247241266918,-2.76704605021946,13.3011388267244));
#16340=CARTESIAN_POINT('Ctrl Pts',(5.30783405263702,-2.61957993099091,13.30892723657));
#16341=CARTESIAN_POINT('Ctrl Pts',(5.37687753801227,-2.46923439626924,13.3167156464155));
#16342=CARTESIAN_POINT('Ctrl Pts',(5.44229265298793,-2.32678981389564,13.3240947600677));
#16343=CARTESIAN_POINT('Ctrl Pts',(5.50203648760668,-2.18176090623693,13.3314738737199));
#16344=CARTESIAN_POINT('Ctrl Pts',(5.55592228313402,-2.03461498723343,13.3388529873721));
#16345=CARTESIAN_POINT('Ctrl Pts',(5.61279477458043,-1.87931329894982,13.3466410987651));
#16346=CARTESIAN_POINT('Ctrl Pts',(5.66316174465532,-1.72159780226747,13.354429210158));
#16347=CARTESIAN_POINT('Ctrl Pts',(5.70683732227528,-1.56203019803906,13.362217321551));
#16348=CARTESIAN_POINT('Ctrl Pts',(5.75050432495694,-1.4024939221281,13.3700039038841));
#16349=CARTESIAN_POINT('Ctrl Pts',(5.78748247217824,-1.24110657222112,13.3777904862172));
#16350=CARTESIAN_POINT('Ctrl Pts',(5.81763602785388,-1.07844406897924,13.3855770685502));
#16351=CARTESIAN_POINT('Ctrl Pts',(5.84779073327786,-0.915775363452519,
13.3933639477839));
#16352=CARTESIAN_POINT('Ctrl Pts',(5.87112026433525,-0.751831720743396,
13.4011508270176));
#16353=CARTESIAN_POINT('Ctrl Pts',(5.8875400517566,-0.587199030535578,13.4089377062514));
#16354=CARTESIAN_POINT('Ctrl Pts',(5.90395875548152,-0.422577205989584,
13.4167240715556));
#16355=CARTESIAN_POINT('Ctrl Pts',(5.91346859657836,-0.257266742938307,
13.4245104368598));
#16356=CARTESIAN_POINT('Ctrl Pts',(5.9160368967894,-0.0918585778600394,
13.432296802164));
#16357=CARTESIAN_POINT('Ctrl Pts',(5.91860587138391,0.0735930200429167,
13.4400852120096));
#16358=CARTESIAN_POINT('Ctrl Pts',(5.91422965603774,0.239142051566006,13.4478736218552));
#16359=CARTESIAN_POINT('Ctrl Pts',(5.90292771101162,0.404196735601776,13.4556620317008));
#16360=CARTESIAN_POINT('Ctrl Pts',(5.89221970533505,0.560577472679632,13.4630411453529));
#16361=CARTESIAN_POINT('Ctrl Pts',(5.87529518657233,0.716514224268211,13.470420259005));
#16362=CARTESIAN_POINT('Ctrl Pts',(5.85221373708393,0.871507279364983,13.4777993726572));
#16363=CARTESIAN_POINT('Ctrl Pts',(5.82785296583125,1.03509104228522,13.4855874840502));
#16364=CARTESIAN_POINT('Ctrl Pts',(5.79662469670607,1.1976819546261,13.4933755954432));
#16365=CARTESIAN_POINT('Ctrl Pts',(5.75863444956288,1.35869784676641,13.5011637068362));
#16366=CARTESIAN_POINT('Ctrl Pts',(5.72065166114231,1.51968212624377,13.5089502891693));
#16367=CARTESIAN_POINT('Ctrl Pts',(5.67590961698329,1.67909169172433,13.5167368715024));
#16368=CARTESIAN_POINT('Ctrl Pts',(5.62456466488435,1.83635587319953,13.5245234538355));
#16369=CARTESIAN_POINT('Ctrl Pts',(5.57321775501406,1.9936260511222,13.5323103330692));
#16370=CARTESIAN_POINT('Ctrl Pts',(5.51526752883052,2.14875037638898,13.540097212303));
#16371=CARTESIAN_POINT('Ctrl Pts',(5.45092003441312,2.30117390497409,13.5478840915367));
#16372=CARTESIAN_POINT('Ctrl Pts',(5.38657678689338,2.45358737369387,13.5556704568408));
#16373=CARTESIAN_POINT('Ctrl Pts',(5.31583724044993,2.60330010809086,13.563456822145));
#16374=CARTESIAN_POINT('Ctrl Pts',(5.2389554244086,2.74977755892357,13.5712431874492));
#16375=CARTESIAN_POINT('Ctrl Pts',(5.16205342076334,2.89629347176089,13.5790315972948));
#16376=CARTESIAN_POINT('Ctrl Pts',(5.07900607161702,3.03957211950319,13.5868200071404));
#16377=CARTESIAN_POINT('Ctrl Pts',(4.990113594419,3.17910315612669,13.594608416986));
#16378=CARTESIAN_POINT('Ctrl Pts',(4.90589259102248,3.31130156345884,13.6019875306381));
#16379=CARTESIAN_POINT('Ctrl Pts',(4.81642514389851,3.44013589792041,13.6093666442902));
#16380=CARTESIAN_POINT('Ctrl Pts',(4.72200265304312,3.56519585817578,13.6167457579423));
#16381=CARTESIAN_POINT('Ctrl Pts',(4.62234666298081,3.69718744242121,13.6245338693353));
#16382=CARTESIAN_POINT('Ctrl Pts',(4.51713518100456,3.82502152875385,13.6323219807282));
#16383=CARTESIAN_POINT('Ctrl Pts',(4.40673939698348,3.94823738515983,13.6401100921212));
#16384=CARTESIAN_POINT('Ctrl Pts',(4.29636528725013,4.07142905028035,13.6478966744543));
#16385=CARTESIAN_POINT('Ctrl Pts',(4.18080911946914,4.1900040567933,13.6556832567873));
#16386=CARTESIAN_POINT('Ctrl Pts',(4.0604812148673,4.30353608863801,13.6634698391204));
#16387=CARTESIAN_POINT('Ctrl Pts',(3.94014872218915,4.41707244943392,13.6712567183541));
#16388=CARTESIAN_POINT('Ctrl Pts',(3.81504435830708,4.52556522864861,13.6790435975878));
#16389=CARTESIAN_POINT('Ctrl Pts',(3.68561456353431,4.62862569793279,13.6868304768215));
#16390=CARTESIAN_POINT('Ctrl Pts',(3.55619331105306,4.73167936528567,13.6946168421257));
#16391=CARTESIAN_POINT('Ctrl Pts',(3.42244744901976,4.82930124121891,13.7024032074299));
#16392=CARTESIAN_POINT('Ctrl Pts',(3.28485579359134,4.92114346242918,13.7101895727341));
#16393=CARTESIAN_POINT('Ctrl Pts',(3.14722800938819,5.01300979954175,13.7179779825797));
#16394=CARTESIAN_POINT('Ctrl Pts',(3.00575267880336,5.09909327028345,13.7257663924253));
#16395=CARTESIAN_POINT('Ctrl Pts',(2.86093759716649,5.17908936277597,13.7335548022709));
#16396=CARTESIAN_POINT('Ctrl Pts',(2.72373283173475,5.25488150391093,13.7409339159231));
#16397=CARTESIAN_POINT('Ctrl Pts',(2.58353053539893,5.32520949217967,13.7483130295753));
#16398=CARTESIAN_POINT('Ctrl Pts',(2.44078289577494,5.3898524486476,13.7556921432275));
#16399=CARTESIAN_POINT('Ctrl Pts',(2.2901232676854,5.45807833179158,13.7634802546205));
#16400=CARTESIAN_POINT('Ctrl Pts',(2.13657432894415,5.51999547787825,13.7712683660134));
#16401=CARTESIAN_POINT('Ctrl Pts',(1.9806824602908,5.57537689793223,13.7790564774064));
#16402=CARTESIAN_POINT('Ctrl Pts',(1.82482119828813,5.63074744480987,13.7868430597394));
#16403=CARTESIAN_POINT('Ctrl Pts',(1.66661822510406,5.67958471907336,13.7946296420725));
#16404=CARTESIAN_POINT('Ctrl Pts',(1.50663781781091,5.72171067500289,13.8024162244055));
#16405=CARTESIAN_POINT('Ctrl Pts',(1.3466513105004,5.76383823718574,13.8102031036392));
#16406=CARTESIAN_POINT('Ctrl Pts',(1.18488754144456,5.7992538837969,13.8179899828729));
#16407=CARTESIAN_POINT('Ctrl Pts',(1.02192452142343,5.82782985638853,13.8257768621066));
#16408=CARTESIAN_POINT('Ctrl Pts',(0.85897225686742,5.85640394298248,13.8335632274108));
#16409=CARTESIAN_POINT('Ctrl Pts',(0.694821214508458,5.87813920383052,13.8413495927149));
#16410=CARTESIAN_POINT('Ctrl Pts',(0.530058283814878,5.8929592547598,13.8491359580191));
#16411=CARTESIAN_POINT('Ctrl Pts',(0.365252089721593,5.90778319713351,13.8569243678647));
#16412=CARTESIAN_POINT('Ctrl Pts',(0.199834004521786,5.91568827067656,13.8647127777103));
#16413=CARTESIAN_POINT('Ctrl Pts',(0.0343956241064442,5.91665002375012,
13.8725011875558));
#16414=CARTESIAN_POINT('Ctrl Pts',(-0.12234864535721,5.91756123481579,13.8798803012081));
#16415=CARTESIAN_POINT('Ctrl Pts',(-0.279110871713278,5.91224012403344,
13.8872594148603));
#16416=CARTESIAN_POINT('Ctrl Pts',(-0.435388302423011,5.90070907506998,
13.8946385285126));
#16417=CARTESIAN_POINT('Ctrl Pts',(-0.600327629276045,5.88853890151834,
13.9024266399056));
#16418=CARTESIAN_POINT('Ctrl Pts',(-0.764785803487357,5.86944653384659,
13.9102147512985));
#16419=CARTESIAN_POINT('Ctrl Pts',(-0.928174436127251,5.84349405566737,
13.9180028626915));
#16420=CARTESIAN_POINT('Ctrl Pts',(-1.09153099025755,5.81754667280479,13.9257894450246));
#16421=CARTESIAN_POINT('Ctrl Pts',(-1.25381810642313,5.7847419169213,13.9335760273576));
#16422=CARTESIAN_POINT('Ctrl Pts',(-1.41445509669538,5.74519341205607,13.9413626096907));
#16423=CARTESIAN_POINT('Ctrl Pts',(-1.57509821202015,5.70564339921519,13.9491494889244));
#16424=CARTESIAN_POINT('Ctrl Pts',(-1.73409076435548,5.6593491954094,13.9569363681581));
#16425=CARTESIAN_POINT('Ctrl Pts',(-1.89086406509477,5.60647515376937,13.9647232473918));
#16426=CARTESIAN_POINT('Ctrl Pts',(-2.04762701888733,5.55360460178535,13.972509612696));
#16427=CARTESIAN_POINT('Ctrl Pts',(-2.20217071143322,5.49415518323302,13.9802959780003));
#16428=CARTESIAN_POINT('Ctrl Pts',(-2.35394323681174,5.42834061204419,13.9880823433045));
#16429=CARTESIAN_POINT('Ctrl Pts',(-2.50575561457341,5.36250875928545,13.9958707531501));
#16430=CARTESIAN_POINT('Ctrl Pts',(-2.6547950770493,5.29030853958997,14.0036591629957));
#16431=CARTESIAN_POINT('Ctrl Pts',(-2.8005304318572,5.21200152175167,14.0114475728413));
#16432=CARTESIAN_POINT('Ctrl Pts',(-2.93860710830029,5.1378096910903,14.0188266864935));
#16433=CARTESIAN_POINT('Ctrl Pts',(-3.07371779055359,5.05813652514174,14.0262058001456));
#16434=CARTESIAN_POINT('Ctrl Pts',(-3.20543170927236,4.97324221405828,14.0335849137977));
#16435=CARTESIAN_POINT('Ctrl Pts',(-3.3444460569765,4.8836425165179,14.0413730251907));
#16436=CARTESIAN_POINT('Ctrl Pts',(-3.47972607179349,4.78819448270224,14.0491611365836));
#16437=CARTESIAN_POINT('Ctrl Pts',(-3.61078477896287,4.68723413566146,14.0569492479766));
#16438=CARTESIAN_POINT('Ctrl Pts',(-3.74181775503953,4.58629361042503,14.0647358303096));
#16439=CARTESIAN_POINT('Ctrl Pts',(-3.86863082415813,4.47984312624384,14.0725224126427));
#16440=CARTESIAN_POINT('Ctrl Pts',(-3.99076843274064,4.3682602805626,14.0803089949757));
#16441=CARTESIAN_POINT('Ctrl Pts',(-4.11291069840339,4.25667318025191,14.0880958742094));
#16442=CARTESIAN_POINT('Ctrl Pts',(-4.23037690824559,4.13995353944782,14.0958827534431));
#16443=CARTESIAN_POINT('Ctrl Pts',(-4.34274631615404,4.01851776106944,14.1036696326768));
#16444=CARTESIAN_POINT('Ctrl Pts',(-4.45510830774686,3.89708999738186,14.111455997981));
#16445=CARTESIAN_POINT('Ctrl Pts',(-4.56237395361935,3.770946953628,14.1192423632853));
#16446=CARTESIAN_POINT('Ctrl Pts',(-4.66416086086581,3.64054034814443,14.1270287285895));
#16447=CARTESIAN_POINT('Ctrl Pts',(-4.76597449528655,3.51009950053516,14.134817138435));
#16448=CARTESIAN_POINT('Ctrl Pts',(-4.86230631818407,3.37539310500728,14.1426055482806));
#16449=CARTESIAN_POINT('Ctrl Pts',(-4.95281502113717,3.23690499225695,14.1503939581262));
#16450=CARTESIAN_POINT('Ctrl Pts',(-5.03856731446105,3.10569470110308,14.1577730717784));
#16451=CARTESIAN_POINT('Ctrl Pts',(-5.11909263648977,2.97109016052616,14.1651521854306));
#16452=CARTESIAN_POINT('Ctrl Pts',(-5.19413720297289,2.83352594468323,14.1725312990828));
#16453=CARTESIAN_POINT('Ctrl Pts',(-5.27334530227268,2.68832955566769,14.1803198118866));
#16454=CARTESIAN_POINT('Ctrl Pts',(-5.34647549203921,2.53978395594202,14.1881083246904));
#16455=CARTESIAN_POINT('Ctrl Pts',(-5.41326089867347,2.38841725948228,14.1958968374942));
#16456=CARTESIAN_POINT('Ctrl Pts',(-5.48003320542014,2.2370802534416,14.2036838225893));
#16457=CARTESIAN_POINT('Ctrl Pts',(-5.54046308335368,2.0829235468732,14.2114708076845));
#16458=CARTESIAN_POINT('Ctrl Pts',(-5.59433114166826,1.9264967271866,14.2192577927796));
#16459=CARTESIAN_POINT('Ctrl Pts',(-5.64820127053387,1.77006389485125,14.2270450771867));
#16460=CARTESIAN_POINT('Ctrl Pts',(-5.69550896734166,1.61136107555123,14.2348323615937));
#16461=CARTESIAN_POINT('Ctrl Pts',(-5.73608397242631,1.4509552797292,14.2426196460007));
#16462=CARTESIAN_POINT('Ctrl Pts',(-5.77665628716277,1.29056011970228,14.2504064140676));
#16463=CARTESIAN_POINT('Ctrl Pts',(-5.81049672527585,1.12846251887456,14.2581931821344));
#16464=CARTESIAN_POINT('Ctrl Pts',(-5.83748560214795,0.965242149522809,
14.2659799502012));
#16465=CARTESIAN_POINT('Ctrl Pts',(-5.86448157733698,0.801978851748411,
14.273768766258));
#16466=CARTESIAN_POINT('Ctrl Pts',(-5.88462233636885,0.637592510450985,
14.2815575823147));
#16467=CARTESIAN_POINT('Ctrl Pts',(-5.89783963535104,0.472671342670865,
14.2893463983715));
#16468=CARTESIAN_POINT('Ctrl Pts',(-5.91044148206916,0.315429588531977,
14.2967725348457));
#16469=CARTESIAN_POINT('Ctrl Pts',(-5.91674997047388,0.157701949386365,
14.30419867132));
#16470=CARTESIAN_POINT('Ctrl Pts',(-5.9167499999999,1.10778128295403E-6,
14.3116248077942));
#16471=CARTESIAN_POINT('Origin',(0.,0.,0.));
#16472=CARTESIAN_POINT('',(-5.91670008156886,7.08465806803855E-6,16.3133751922624));
#16473=CARTESIAN_POINT('',(-5.91674999941157,-8.34454905785101E-5,16.0616248078328));
#16474=CARTESIAN_POINT('',(-5.91675,-7.2459289488551E-16,0.));
#16475=CARTESIAN_POINT('Ctrl Pts',(-5.91624282479069,7.08533173049419E-6,
16.3133751922049));
#16476=CARTESIAN_POINT('Ctrl Pts',(-5.9162630038869,0.48475024959515,16.2905618658795));
#16477=CARTESIAN_POINT('Ctrl Pts',(-5.7377459192182,1.95412248637943,16.2214085410499));
#16478=CARTESIAN_POINT('Ctrl Pts',(-4.53467287003993,4.18117692240458,16.1059152177163));
#16479=CARTESIAN_POINT('Ctrl Pts',(-1.98003345441907,5.84165781384912,15.9668952222037));
#16480=CARTESIAN_POINT('Ctrl Pts',(1.05774857675516,6.07673155924276,15.8278752266912));
#16481=CARTESIAN_POINT('Ctrl Pts',(3.83743223447477,4.82903844885686,15.6888552311787));
#16482=CARTESIAN_POINT('Ctrl Pts',(5.68075441676886,2.40302470879641,15.5498352356661));
#16483=CARTESIAN_POINT('Ctrl Pts',(6.13793105636612,-0.609344600385745,
15.4108152401537));
#16484=CARTESIAN_POINT('Ctrl Pts',(5.0974077161784,-3.47302937934159,15.2717952446411));
#16485=CARTESIAN_POINT('Ctrl Pts',(2.81307968620657,-5.48926963937609,15.1327752491286));
#16486=CARTESIAN_POINT('Ctrl Pts',(-0.157660320451772,-6.16608804008501,
14.9937552536161));
#16487=CARTESIAN_POINT('Ctrl Pts',(-3.08993005812401,-5.33833595145761,
14.8547352581036));
#16488=CARTESIAN_POINT('Ctrl Pts',(-5.2682343075742,-3.20799092505311,14.715715262591));
#16489=CARTESIAN_POINT('Ctrl Pts',(-5.89196019578445,-1.17287284551572,
14.6185952406248));
#16490=CARTESIAN_POINT('Ctrl Pts',(-5.91720968061764,-0.0943942614492433,
14.5678152171628));
#16491=CARTESIAN_POINT('Ctrl Pts',(-5.91713904777553,-9.26149740448912E-5,
14.5633751922049));
#16492=CARTESIAN_POINT('Ctrl Pts',(-5.9167499999999,1.10775218765784E-6,
14.3116248077956));
#16493=CARTESIAN_POINT('Ctrl Pts',(-5.91675003096271,-0.165378134030277,
14.3194125203214));
#16494=CARTESIAN_POINT('Ctrl Pts',(-5.90981193875335,-0.330786962771931,
14.3272002328471));
#16495=CARTESIAN_POINT('Ctrl Pts',(-5.8959543270468,-0.495634074573328,
14.3349879453728));
#16496=CARTESIAN_POINT('Ctrl Pts',(-5.88209943852473,-0.660448791968869,
14.342774127521));
#16497=CARTESIAN_POINT('Ctrl Pts',(-5.8613277703964,-0.824701694397815,
14.3505603096692));
#16498=CARTESIAN_POINT('Ctrl Pts',(-5.83370989376855,-0.987805364354207,
14.3583464918173));
#16499=CARTESIAN_POINT('Ctrl Pts',(-5.80609097249611,-1.15091520369749,
14.3661329684774));
#16500=CARTESIAN_POINT('Ctrl Pts',(-5.77162537401302,-1.31287540782977,
14.3739194451375));
#16501=CARTESIAN_POINT('Ctrl Pts',(-5.7304351438749,-1.47310679325821,14.3817059217975));
#16502=CARTESIAN_POINT('Ctrl Pts',(-5.68924761963206,-1.63332765266267,
14.3894918869433));
#16503=CARTESIAN_POINT('Ctrl Pts',(-5.64133642746416,-1.79181961111337,
14.3972778520891));
#16504=CARTESIAN_POINT('Ctrl Pts',(-5.5868740747597,-1.94801659009309,14.4050638172349));
#16505=CARTESIAN_POINT('Ctrl Pts',(-5.53239744487556,-2.10425451574928,
14.4128518234534));
#16506=CARTESIAN_POINT('Ctrl Pts',(-5.47136632627987,-2.25819595716394,
14.4206398296719));
#16507=CARTESIAN_POINT('Ctrl Pts',(-5.40400247469969,-2.40929197399145,
14.4284278358904));
#16508=CARTESIAN_POINT('Ctrl Pts',(-5.340582262263,-2.55154247274941,14.4357599138113));
#16509=CARTESIAN_POINT('Ctrl Pts',(-5.27154958777164,-2.69127090072943,
14.4430919917322));
#16510=CARTESIAN_POINT('Ctrl Pts',(-5.19712781468605,-2.82803695879609,
14.4504240696531));
#16511=CARTESIAN_POINT('Ctrl Pts',(-5.11807722833013,-2.97330945951067,
14.4582121810461));
#16512=CARTESIAN_POINT('Ctrl Pts',(-5.03291762851382,-3.11529133204175,
14.4660002924391));
#16513=CARTESIAN_POINT('Ctrl Pts',(-4.94194802326531,-3.25347203735396,
14.473788403832));
#16514=CARTESIAN_POINT('Ctrl Pts',(-4.85099627831309,-3.39162561329332,
14.4815749861651));
#16515=CARTESIAN_POINT('Ctrl Pts',(-4.75423697954309,-3.52597924436967,
14.4893615684982));
#16516=CARTESIAN_POINT('Ctrl Pts',(-4.65201292374638,-3.65605064513563,
14.4971481508312));
#16517=CARTESIAN_POINT('Ctrl Pts',(-4.54978497016906,-3.78612700549529,
14.5049350300649));
#16518=CARTESIAN_POINT('Ctrl Pts',(-4.44209203694593,-3.91192055516285,
14.5127219092987));
#16519=CARTESIAN_POINT('Ctrl Pts',(-4.32931819929146,-4.03298084446031,
14.5205087885324));
#16520=CARTESIAN_POINT('Ctrl Pts',(-4.21655180464509,-4.15403314384864,
14.5282951538366));
#16521=CARTESIAN_POINT('Ctrl Pts',(-4.09870539452829,-4.27035257427359,
14.5360815191408));
#16522=CARTESIAN_POINT('Ctrl Pts',(-3.97620110490398,-4.38152431647484,
14.5438678844449));
#16523=CARTESIAN_POINT('Ctrl Pts',(-3.85366464814084,-4.4927252501181,14.5516562942906));
#16524=CARTESIAN_POINT('Ctrl Pts',(-3.72646810340338,-4.59877557829264,
14.5594447041362));
#16525=CARTESIAN_POINT('Ctrl Pts',(-3.59506867557559,-4.69929907330819,
14.5672331139818));
#16526=CARTESIAN_POINT('Ctrl Pts',(-3.47057454506767,-4.79453986175346,
14.5746122276339));
#16527=CARTESIAN_POINT('Ctrl Pts',(-3.34230811575963,-4.88481961000261,
14.5819913412861));
#16528=CARTESIAN_POINT('Ctrl Pts',(-3.21068395809315,-4.96985302436031,
14.5893704549382));
#16529=CARTESIAN_POINT('Ctrl Pts',(-3.07176434657417,-5.05959953516903,
14.5971585663312));
#16530=CARTESIAN_POINT('Ctrl Pts',(-2.92905462345105,-5.14353370279028,
14.6049466777241));
#16531=CARTESIAN_POINT('Ctrl Pts',(-2.78306161437668,-5.22135026722811,
14.6127347891171));
#16532=CARTESIAN_POINT('Ctrl Pts',(-2.63709726848453,-5.2991515537401,14.6205213714501));
#16533=CARTESIAN_POINT('Ctrl Pts',(-2.48785120464156,-5.37083748338602,
14.6283079537832));
#16534=CARTESIAN_POINT('Ctrl Pts',(-2.33585518290006,-5.43614855637877,
14.6360945361162));
#16535=CARTESIAN_POINT('Ctrl Pts',(-2.1838533655841,-5.50146211966818,14.6438814153499));
#16536=CARTESIAN_POINT('Ctrl Pts',(-2.02910167255777,-5.5604002101492,14.6516682945836));
#16537=CARTESIAN_POINT('Ctrl Pts',(-1.87215288004449,-5.61275103280389,
14.6594551738174));
#16538=CARTESIAN_POINT('Ctrl Pts',(-1.71521444606072,-5.66509840033457,
14.6672415391215));
#16539=CARTESIAN_POINT('Ctrl Pts',(-1.55607950594408,-5.71085926905235,
14.6750279044257));
#16540=CARTESIAN_POINT('Ctrl Pts',(-1.39531721108171,-5.74987134142662,
14.6828142697299));
#16541=CARTESIAN_POINT('Ctrl Pts',(-1.23451270330536,-5.78889365757886,
14.6906026795755));
#16542=CARTESIAN_POINT('Ctrl Pts',(-1.07208029719107,-5.82116355907977,
14.6983910894211));
#16543=CARTESIAN_POINT('Ctrl Pts',(-0.908601475378053,-5.84656941474578,
14.7061794992667));
#16544=CARTESIAN_POINT('Ctrl Pts',(-0.753713785874834,-5.87064014293137,
14.7135586129189));
#16545=CARTESIAN_POINT('Ctrl Pts',(-0.59788709126143,-5.88854966770614,
14.7209377265711));
#16546=CARTESIAN_POINT('Ctrl Pts',(-0.441621929870274,-5.90024581128258,
14.7283168402233));
#16547=CARTESIAN_POINT('Ctrl Pts',(-0.276695552379318,-5.91259023004812,
14.7361049516163));
#16548=CARTESIAN_POINT('Ctrl Pts',(-0.111221821319569,-5.91801737454039,
14.7438930630093));
#16549=CARTESIAN_POINT('Ctrl Pts',(0.0542081609874399,-5.91650167225383,
14.7516811744022));
#16550=CARTESIAN_POINT('Ctrl Pts',(0.21960566400132,-5.914986267549,14.7594677567353));
#16551=CARTESIAN_POINT('Ctrl Pts',(0.384959116082934,-5.90653073879459,
14.7672543390683));
#16552=CARTESIAN_POINT('Ctrl Pts',(0.549677412743056,-5.89116162606494,
14.7750409214014));
#16553=CARTESIAN_POINT('Ctrl Pts',(0.71440199007518,-5.87579192731444,14.7828278006351));
#16554=CARTESIAN_POINT('Ctrl Pts',(0.878491045024127,-5.85350814285044,
14.7906146798688));
#16555=CARTESIAN_POINT('Ctrl Pts',(1.0413578419649,-5.8243887582714,14.7984015591025));
#16556=CARTESIAN_POINT('Ctrl Pts',(1.20421388979135,-5.79527129555488,14.8061879244067));
#16557=CARTESIAN_POINT('Ctrl Pts',(1.365847526495,-5.75931919189307,14.8139742897109));
#16558=CARTESIAN_POINT('Ctrl Pts',(1.52568131838922,-5.71666223221367,14.8217606550151));
#16559=CARTESIAN_POINT('Ctrl Pts',(1.68555707939135,-5.67399407168291,14.8295490648607));
#16560=CARTESIAN_POINT('Ctrl Pts',(1.84363174179873,-5.62461761774218,14.8373374747063));
#16561=CARTESIAN_POINT('Ctrl Pts',(1.99934128413789,-5.5687130463009,14.8451258845519));
#16562=CARTESIAN_POINT('Ctrl Pts',(2.14686798502193,-5.51574636959522,14.8525049982041));
#16563=CARTESIAN_POINT('Ctrl Pts',(2.29227151074867,-5.45692014637828,14.8598841118563));
#16564=CARTESIAN_POINT('Ctrl Pts',(2.43508736348934,-5.3924280333329,14.8672632255085));
#16565=CARTESIAN_POINT('Ctrl Pts',(2.58581898550395,-5.32436135431982,14.8750513369015));
#16566=CARTESIAN_POINT('Ctrl Pts',(2.73372178324025,-5.24995858562116,14.8828394482945));
#16567=CARTESIAN_POINT('Ctrl Pts',(2.87826446146846,-5.16948007563117,14.8906275596874));
#16568=CARTESIAN_POINT('Ctrl Pts',(3.02277876126157,-5.08901736619366,14.8984141420205));
#16569=CARTESIAN_POINT('Ctrl Pts',(3.16393397884555,-5.00248145092886,14.9062007243536));
#16570=CARTESIAN_POINT('Ctrl Pts',(3.30122374958302,-4.91017844051405,14.9139873066866));
#16571=CARTESIAN_POINT('Ctrl Pts',(3.4385187551488,-4.81787191060606,14.9217741859203));
#16572=CARTESIAN_POINT('Ctrl Pts',(3.57194775158137,-4.71979802052766,14.929561065154));
#16573=CARTESIAN_POINT('Ctrl Pts',(3.70103306321329,-4.61630640528789,14.9373479443878));
#16574=CARTESIAN_POINT('Ctrl Pts',(3.83010985528933,-4.51282162043485,14.9451343096919));
#16575=CARTESIAN_POINT('Ctrl Pts',(3.95484328701192,-4.40392002594475,14.9529206749961));
#16576=CARTESIAN_POINT('Ctrl Pts',(4.07478839436612,-4.28999185356326,14.9607070403003));
#16577=CARTESIAN_POINT('Ctrl Pts',(4.19476499686976,-4.17603376595728,14.9684954501459));
#16578=CARTESIAN_POINT('Ctrl Pts',(4.30995052945779,-4.05704668186232,14.9762838599915));
#16579=CARTESIAN_POINT('Ctrl Pts',(4.41993591450846,-3.93345866561964,14.9840722698371));
#16580=CARTESIAN_POINT('Ctrl Pts',(4.52414135213382,-3.81636544171644,14.9914513834893));
#16581=CARTESIAN_POINT('Ctrl Pts',(4.62367896750848,-3.69514261813513,14.9988304971414));
#16582=CARTESIAN_POINT('Ctrl Pts',(4.71823352667229,-3.5701824813706,15.0062096107936));
#16583=CARTESIAN_POINT('Ctrl Pts',(4.81802890511365,-3.43829625347443,15.0139977221866));
#16584=CARTESIAN_POINT('Ctrl Pts',(4.91230881964435,-3.30219956988426,15.0217858335795));
#16585=CARTESIAN_POINT('Ctrl Pts',(5.00073128764819,-3.16237523884129,15.0295739449725));
#16586=CARTESIAN_POINT('Ctrl Pts',(5.08913639544186,-3.02257835986821,15.0373605273055));
#16587=CARTESIAN_POINT('Ctrl Pts',(5.17168618063996,-2.8790555636108,15.0451471096386));
#16588=CARTESIAN_POINT('Ctrl Pts',(5.24808244703849,-2.73231791554102,15.0529336919716));
#16589=CARTESIAN_POINT('Ctrl Pts',(5.32448162640965,-2.5855746723974,15.0607205712053));
#16590=CARTESIAN_POINT('Ctrl Pts',(5.39472666642934,-2.43561661373874,15.068507450439));
#16591=CARTESIAN_POINT('Ctrl Pts',(5.45856538690808,-2.28297929893134,15.0762943296727));
#16592=CARTESIAN_POINT('Ctrl Pts',(5.5223998940682,-2.13035205809842,15.0840806949769));
#16593=CARTESIAN_POINT('Ctrl Pts',(5.57982880461097,-1.97504620983258,15.0918670602811));
#16594=CARTESIAN_POINT('Ctrl Pts',(5.63064808610609,-1.81761731201314,15.0996534255853));
#16595=CARTESIAN_POINT('Ctrl Pts',(5.68148071171253,-1.66014707656208,15.1074418354309));
#16596=CARTESIAN_POINT('Ctrl Pts',(5.72570014020122,-1.50055298129828,15.1152302452764));
#16597=CARTESIAN_POINT('Ctrl Pts',(5.76315195225073,-1.33940663645087,15.123018655122));
#16598=CARTESIAN_POINT('Ctrl Pts',(5.79863559821622,-1.18672884767953,15.1303977687743));
#16599=CARTESIAN_POINT('Ctrl Pts',(5.82804457680214,-1.03265801393605,15.1377768824265));
#16600=CARTESIAN_POINT('Ctrl Pts',(5.85128975756504,-0.877689429989035,
15.1451559960787));
#16601=CARTESIAN_POINT('Ctrl Pts',(5.87582333512782,-0.714131494568395,
15.1529441074717));
#16602=CARTESIAN_POINT('Ctrl Pts',(5.8934992274515,-0.549515054323571,15.1607322188647));
#16603=CARTESIAN_POINT('Ctrl Pts',(5.90424812428272,-0.384427690735162,
15.1685203302576));
#16604=CARTESIAN_POINT('Ctrl Pts',(5.91499491075543,-0.219372739172725,
15.1763069125907));
#16605=CARTESIAN_POINT('Ctrl Pts',(5.91881739458184,-0.0538473674034925,
15.1840934949238));
#16606=CARTESIAN_POINT('Ctrl Pts',(5.91569823461231,0.111556978736245,15.1918800772569));
#16607=CARTESIAN_POINT('Ctrl Pts',(5.91257895570991,0.276967631706899,15.1996669564906));
#16608=CARTESIAN_POINT('Ctrl Pts',(5.90251750545671,0.442256930280642,15.2074538357243));
#16609=CARTESIAN_POINT('Ctrl Pts',(5.88554866915859,0.60683393565751,15.215240714958));
#16610=CARTESIAN_POINT('Ctrl Pts',(5.86858095279385,0.771400079047217,15.2230270802622));
#16611=CARTESIAN_POINT('Ctrl Pts',(5.84470679556843,0.935253705460038,15.2308134455664));
#16612=CARTESIAN_POINT('Ctrl Pts',(5.81401283042844,1.09780935053107,15.2385998108706));
#16613=CARTESIAN_POINT('Ctrl Pts',(5.78331080567652,1.26040767941348,15.2463882207162));
#16614=CARTESIAN_POINT('Ctrl Pts',(5.74578545214969,1.4217070313706,15.2541766305619));
#16615=CARTESIAN_POINT('Ctrl Pts',(5.70157464920767,1.58113158276359,15.2619650404075));
#16616=CARTESIAN_POINT('Ctrl Pts',(5.65968721056133,1.7321780616966,15.2693441540596));
#16617=CARTESIAN_POINT('Ctrl Pts',(5.61179898598714,1.88154147012821,15.2767232677117));
#16618=CARTESIAN_POINT('Ctrl Pts',(5.55806867449139,2.02874423526907,15.2841023813638));
#16619=CARTESIAN_POINT('Ctrl Pts',(5.50136028499707,2.18410592046812,15.2918904927568));
#16620=CARTESIAN_POINT('Ctrl Pts',(5.43812357952267,2.33711614446931,15.2996786041497));
#16621=CARTESIAN_POINT('Ctrl Pts',(5.36857881485322,2.48722577809277,15.3074667155427));
#16622=CARTESIAN_POINT('Ctrl Pts',(5.29904770408597,2.63730594030648,15.3152532978758));
#16623=CARTESIAN_POINT('Ctrl Pts',(5.22321113949174,2.78448635867911,15.3230398802088));
#16624=CARTESIAN_POINT('Ctrl Pts',(5.14133686195587,2.92823937450369,15.3308264625419));
#16625=CARTESIAN_POINT('Ctrl Pts',(5.05945946257203,3.07199787159876,15.3386133417756));
#16626=CARTESIAN_POINT('Ctrl Pts',(4.97154404428249,3.21232842504674,15.3464002210093));
#16627=CARTESIAN_POINT('Ctrl Pts',(4.877903878819,3.34872876051533,15.354187100243));
#16628=CARTESIAN_POINT('Ctrl Pts',(4.78426989355225,3.48512009364071,15.3619734655472));
#16629=CARTESIAN_POINT('Ctrl Pts',(4.68491209816364,3.61758146448982,15.3697598308514));
#16630=CARTESIAN_POINT('Ctrl Pts',(4.58018667381851,3.74564021169617,15.3775461961556));
#16631=CARTESIAN_POINT('Ctrl Pts',(4.47543375070362,3.87373258452904,15.3853346060012));
#16632=CARTESIAN_POINT('Ctrl Pts',(4.36531058320663,3.99741977497081,15.3931230158467));
#16633=CARTESIAN_POINT('Ctrl Pts',(4.25021374067511,4.116262105488,15.4009114256923));
#16634=CARTESIAN_POINT('Ctrl Pts',(4.14116546267098,4.22885903874746,15.4082905393446));
#16635=CARTESIAN_POINT('Ctrl Pts',(4.02765299784576,4.33710704178295,15.4156696529968));
#16636=CARTESIAN_POINT('Ctrl Pts',(3.91004419108284,4.44066267422772,15.423048766649));
#16637=CARTESIAN_POINT('Ctrl Pts',(3.78591675098202,4.54995802308117,15.430836878042));
#16638=CARTESIAN_POINT('Ctrl Pts',(3.65718166955882,4.65406512360351,15.4386249894349));
#16639=CARTESIAN_POINT('Ctrl Pts',(3.52429508208788,4.75260715154021,15.4464131008279));
#16640=CARTESIAN_POINT('Ctrl Pts',(3.39143458458177,4.85112983246763,15.454199683161));
#16641=CARTESIAN_POINT('Ctrl Pts',(3.25442446384809,4.94408943067253,15.461986265494));
#16642=CARTESIAN_POINT('Ctrl Pts',(3.11375227980248,5.03115069368081,15.4697728478271));
#16643=CARTESIAN_POINT('Ctrl Pts',(2.97307473195789,5.11821527631561,15.4775597270608));
#16644=CARTESIAN_POINT('Ctrl Pts',(2.82873511100821,5.1993809022184,15.4853466062945));
#16645=CARTESIAN_POINT('Ctrl Pts',(2.68124881376462,5.27435639307639,15.4931334855282));
#16646=CARTESIAN_POINT('Ctrl Pts',(2.53377225053131,5.34932693559537,15.5009198508324));
#16647=CARTESIAN_POINT('Ctrl Pts',(2.38314971151354,5.41810801592708,15.5087062161366));
#16648=CARTESIAN_POINT('Ctrl Pts',(2.22992010538849,5.48045498896617,15.5164925814408));
#16649=CARTESIAN_POINT('Ctrl Pts',(2.07665026428052,5.54281833305429,15.5242809912864));
#16650=CARTESIAN_POINT('Ctrl Pts',(1.92077228359581,5.59874407164264,15.532069401132));
#16651=CARTESIAN_POINT('Ctrl Pts',(1.76284475716744,5.64803584661316,15.5398578109775));
#16652=CARTESIAN_POINT('Ctrl Pts',(1.61321663160311,5.69473724225569,15.5472369246297));
#16653=CARTESIAN_POINT('Ctrl Pts',(1.46174908326808,5.73548391859867,15.5546160382819));
#16654=CARTESIAN_POINT('Ctrl Pts',(1.30892943913352,5.7701502827803,15.5619951519341));
#16655=CARTESIAN_POINT('Ctrl Pts',(1.14763955153279,5.80673807889805,15.5697832633271));
#16656=CARTESIAN_POINT('Ctrl Pts',(0.984785829869154,5.83656549763545,15.57757137472));
#16657=CARTESIAN_POINT('Ctrl Pts',(0.820949102950824,5.85951987221344,15.585359486113));
#16658=CARTESIAN_POINT('Ctrl Pts',(0.657144542517688,5.88246974010015,15.5931460684461));
#16659=CARTESIAN_POINT('Ctrl Pts',(0.49235767815655,5.89854921197925,15.6009326507791));
#16660=CARTESIAN_POINT('Ctrl Pts',(0.327177043964479,5.90769716085741,15.6087192331122));
#16661=CARTESIAN_POINT('Ctrl Pts',(0.161990111471635,5.91684545854481,15.6165061123459));
#16662=CARTESIAN_POINT('Ctrl Pts',(-0.00359030208728486,5.91906168276146,
15.6242929915796));
#16663=CARTESIAN_POINT('Ctrl Pts',(-0.168972305034811,5.91433672719361,
15.6320798708133));
#16664=CARTESIAN_POINT('Ctrl Pts',(-0.334343392865846,5.90961208347009,
15.6398662361175));
#16665=CARTESIAN_POINT('Ctrl Pts',(-0.499515776870923,5.89794718596203,
15.6476526014217));
#16666=CARTESIAN_POINT('Ctrl Pts',(-0.663899182193702,5.87938503913314,
15.6554389667259));
#16667=CARTESIAN_POINT('Ctrl Pts',(-0.828325751260559,5.86081801826143,
15.6632273765715));
#16668=CARTESIAN_POINT('Ctrl Pts',(-0.991962609739375,5.83535016310612,
15.6710157864171));
#16669=CARTESIAN_POINT('Ctrl Pts',(-1.15422529898659,5.80307629810942,15.6788041962627));
#16670=CARTESIAN_POINT('Ctrl Pts',(-1.30796076607134,5.77249848793681,15.6861833099149));
#16671=CARTESIAN_POINT('Ctrl Pts',(-1.4604625245801,5.7358116581035,15.693562423567));
#16672=CARTESIAN_POINT('Ctrl Pts',(-1.61124255352161,5.69313867705866,15.7009415372192));
#16673=CARTESIAN_POINT('Ctrl Pts',(-1.77037977739198,5.64810048608985,15.7087296486122));
#16674=CARTESIAN_POINT('Ctrl Pts',(-1.92765583671498,5.59637766006532,15.7165177600051));
#16675=CARTESIAN_POINT('Ctrl Pts',(-2.08250678869568,5.53814915269862,15.7243058713981));
#16676=CARTESIAN_POINT('Ctrl Pts',(-2.23732733839127,5.47993207748432,15.7320924537311));
#16677=CARTESIAN_POINT('Ctrl Pts',(-2.38972343186278,5.41521198186983,15.7398790360642));
#16678=CARTESIAN_POINT('Ctrl Pts',(-2.53914901857623,5.34421676431293,15.7476656183972));
#16679=CARTESIAN_POINT('Ctrl Pts',(-2.68858030285425,5.27321883972409,15.7554524976309));
#16680=CARTESIAN_POINT('Ctrl Pts',(-2.83504056343902,5.195945447968,15.7632393768646));
#16681=CARTESIAN_POINT('Ctrl Pts',(-2.97800568995612,5.1126717744335,15.7710262560983));
#16682=CARTESIAN_POINT('Ctrl Pts',(-3.1209613808575,5.02940359691332,15.7788126214025));
#16683=CARTESIAN_POINT('Ctrl Pts',(-3.26042212324386,4.94013609104064,15.7865989867066));
#16684=CARTESIAN_POINT('Ctrl Pts',(-3.39589015814186,4.84518942832324,15.7943853520108));
#16685=CARTESIAN_POINT('Ctrl Pts',(-3.53139376419482,4.75021783454032,15.8021737618564));
#16686=CARTESIAN_POINT('Ctrl Pts',(-3.66290230488369,4.64956428604458,15.809962171702));
#16687=CARTESIAN_POINT('Ctrl Pts',(-3.78994792108942,4.54359167596847,15.8177505815476));
#16688=CARTESIAN_POINT('Ctrl Pts',(-3.91031704130632,4.44318813413124,15.8251296951998));
#16689=CARTESIAN_POINT('Ctrl Pts',(-4.02668004342882,4.33801037237021,15.8325088088521));
#16690=CARTESIAN_POINT('Ctrl Pts',(-4.13866716968353,4.22839977072695,15.8398879225043));
#16691=CARTESIAN_POINT('Ctrl Pts',(-4.25686133973629,4.1127138475009,15.8476760338973));
#16692=CARTESIAN_POINT('Ctrl Pts',(-4.37022301358027,3.99204844039662,15.8554641452903));
#16693=CARTESIAN_POINT('Ctrl Pts',(-4.47834259794153,3.86683050287471,15.8632522566833));
#16694=CARTESIAN_POINT('Ctrl Pts',(-4.58644095490732,3.74163714971184,15.8710388390164));
#16695=CARTESIAN_POINT('Ctrl Pts',(-4.68929906724063,3.61189329124728,15.8788254213495));
#16696=CARTESIAN_POINT('Ctrl Pts',(-4.78654647016189,3.47806030015018,15.8866120036826));
#16697=CARTESIAN_POINT('Ctrl Pts',(-4.88379758110478,3.3442222060312,15.8943988829163));
#16698=CARTESIAN_POINT('Ctrl Pts',(-4.97543736353533,3.20629492344992,15.90218576215));
#16699=CARTESIAN_POINT('Ctrl Pts',(-5.06113724256425,3.06477085186301,15.9099726413837));
#16700=CARTESIAN_POINT('Ctrl Pts',(-5.14683146545077,2.92325612078289,15.9177590066879));
#16701=CARTESIAN_POINT('Ctrl Pts',(-5.22658640402623,2.77814534914727,15.9255453719922));
#16702=CARTESIAN_POINT('Ctrl Pts',(-5.30011814611382,2.62995783231119,15.9333317372964));
#16703=CARTESIAN_POINT('Ctrl Pts',(-5.37366919614364,2.4817314044425,15.941120147142));
#16704=CARTESIAN_POINT('Ctrl Pts',(-5.44099364058232,2.3304269025924,15.9489085569876));
#16705=CARTESIAN_POINT('Ctrl Pts',(-5.50185426252937,2.17658683180511,15.9566969668332));
#16706=CARTESIAN_POINT('Ctrl Pts',(-5.55951653957791,2.03083135808319,15.9640760804853));
#16707=CARTESIAN_POINT('Ctrl Pts',(-5.61137679771396,1.88280020103458,15.9714551941374));
#16708=CARTESIAN_POINT('Ctrl Pts',(-5.65727367244669,1.73297003942408,15.9788343077895));
#16709=CARTESIAN_POINT('Ctrl Pts',(-5.70591845315597,1.57416934988649,15.9866552186364));
#16710=CARTESIAN_POINT('Ctrl Pts',(-5.74788083090549,1.41329275660616,15.9944761294833));
#16711=CARTESIAN_POINT('Ctrl Pts',(-5.78300440114525,1.25091592796425,16.0022970403302));
#16712=CARTESIAN_POINT('Ctrl Pts',(-5.81812005154061,1.08857571289005,16.0101161876776));
#16713=CARTESIAN_POINT('Ctrl Pts',(-5.8463999057942,0.924736244257924,16.017935335025));
#16714=CARTESIAN_POINT('Ctrl Pts',(-5.86773839626611,0.759984654769045,
16.0257544823725));
#16715=CARTESIAN_POINT('Ctrl Pts',(-5.88907483684367,0.595248892236278,
16.033572878569));
#16716=CARTESIAN_POINT('Ctrl Pts',(-5.9034712026441,0.429601494728204,16.0413912747655));
#16717=CARTESIAN_POINT('Ctrl Pts',(-5.91087356280468,0.263636657232531,
16.0492096709621));
#16718=CARTESIAN_POINT('Ctrl Pts',(-5.91479172845615,0.175789306992596,
16.0533480499064));
#16719=CARTESIAN_POINT('Ctrl Pts',(-5.91675123959221,0.0878531121041889,
16.0574864288508));
#16720=CARTESIAN_POINT('Ctrl Pts',(-5.91674999941158,-8.34446900113325E-5,
16.0616248077951));
#16721=CARTESIAN_POINT('Origin',(0.,0.,0.));
#16722=CARTESIAN_POINT('',(-5.9167499994649,7.95746162001808E-5,18.0633751922476));
#16723=CARTESIAN_POINT('',(-5.91674999819064,0.000146325028563304,17.8116248078341));
#16724=CARTESIAN_POINT('',(-5.91675,-7.2459289488551E-16,0.));
#16725=CARTESIAN_POINT('Ctrl Pts',(-5.91674999946489,7.95755227456555E-5,
18.0633751922049));
#16726=CARTESIAN_POINT('Ctrl Pts',(-5.91674893504203,0.0792235603697716,
18.0596485131004));
#16727=CARTESIAN_POINT('Ctrl Pts',(-5.9151597379013,0.158363133491373,18.055921833996));
#16728=CARTESIAN_POINT('Ctrl Pts',(-5.91198387910413,0.23743878308492,18.0521951548916));
#16729=CARTESIAN_POINT('Ctrl Pts',(-5.90534700026585,0.402690306823815,
18.0444071771304));
#16730=CARTESIAN_POINT('Ctrl Pts',(-5.89177593913822,0.567692935344161,
18.0366191993691));
#16731=CARTESIAN_POINT('Ctrl Pts',(-5.87131301784458,0.731856549460908,
18.0288312216077));
#16732=CARTESIAN_POINT('Ctrl Pts',(-5.85085411973669,0.895987887603674,
18.0210447750296));
#16733=CARTESIAN_POINT('Ctrl Pts',(-5.82350610458599,1.05928022357998,18.0132583284514));
#16734=CARTESIAN_POINT('Ctrl Pts',(-5.78936306414922,1.22114940689694,18.0054718818733));
#16735=CARTESIAN_POINT('Ctrl Pts',(-5.75521872123245,1.38302476515821,17.9976851382597));
#16736=CARTESIAN_POINT('Ctrl Pts',(-5.7142788964161,1.54347654864934,17.9898983946461));
#16737=CARTESIAN_POINT('Ctrl Pts',(-5.66668878439145,1.70193089852442,17.9821116510325));
#16738=CARTESIAN_POINT('Ctrl Pts',(-5.61910182009667,1.86037476782972,17.9743254224537));
#16739=CARTESIAN_POINT('Ctrl Pts',(-5.56486554086642,2.01682116186363,17.9665391938749));
#16740=CARTESIAN_POINT('Ctrl Pts',(-5.50417503703645,2.1707113405897,17.9587529652961));
#16741=CARTESIAN_POINT('Ctrl Pts',(-5.44346855664941,2.32464203035241,17.9509646870206));
#16742=CARTESIAN_POINT('Ctrl Pts',(-5.37630457209364,2.47601486199876,17.9431764087451));
#16743=CARTESIAN_POINT('Ctrl Pts',(-5.30292669648032,2.62429019246278,17.9353881304696));
#16744=CARTESIAN_POINT('Ctrl Pts',(-5.23316627909153,2.76525569269255,17.9279838067726));
#16745=CARTESIAN_POINT('Ctrl Pts',(-5.15779000658236,2.90342150635967,17.9205794830756));
#16746=CARTESIAN_POINT('Ctrl Pts',(-5.07704608213876,3.03834389797131,17.9131751593787));
#16747=CARTESIAN_POINT('Ctrl Pts',(-4.9921184218028,3.18025727567085,17.9053871816171));
#16748=CARTESIAN_POINT('Ctrl Pts',(-4.90122171273217,3.31863295778427,17.8975992038555));
#16749=CARTESIAN_POINT('Ctrl Pts',(-4.80467558436886,3.45297308003838,17.8898112260939));
#16750=CARTESIAN_POINT('Ctrl Pts',(-4.70814843780226,3.58728678987252,17.8820247795155));
#16751=CARTESIAN_POINT('Ctrl Pts',(-4.60597427453763,3.71756626363497,17.8742383329372));
#16752=CARTESIAN_POINT('Ctrl Pts',(-4.49851532054828,3.84334365797444,17.8664518863588));
#16753=CARTESIAN_POINT('Ctrl Pts',(-4.39105226724193,3.96912585043815,17.8586651427451));
#16754=CARTESIAN_POINT('Ctrl Pts',(-4.27830422435648,4.09040537430116,17.8508783991313));
#16755=CARTESIAN_POINT('Ctrl Pts',(-4.1606733597801,4.2067478835457,17.8430916555176));
#16756=CARTESIAN_POINT('Ctrl Pts',(-4.04305027560537,4.32308269760365,17.8353054269387));
#16757=CARTESIAN_POINT('Ctrl Pts',(-3.92054524333074,4.43448092586513,17.8275191983598));
#16758=CARTESIAN_POINT('Ctrl Pts',(-3.79359700215806,4.54054537998657,17.8197329697809));
#16759=CARTESIAN_POINT('Ctrl Pts',(-3.66661534231701,4.64663775519448,17.8119446915053));
#16760=CARTESIAN_POINT('Ctrl Pts',(-3.53518838048702,4.74739334405995,17.8041564132298));
#16761=CARTESIAN_POINT('Ctrl Pts',(-3.3997883175939,4.84245495157694,17.7963681349542));
#16762=CARTESIAN_POINT('Ctrl Pts',(-3.27106334673067,4.93283011386543,17.7889638112583));
#16763=CARTESIAN_POINT('Ctrl Pts',(-3.13874779404817,5.01805903521906,17.7815594875624));
#16764=CARTESIAN_POINT('Ctrl Pts',(-3.0032719827193,5.09787092424997,17.7741551638666));
#16765=CARTESIAN_POINT('Ctrl Pts',(-2.86077650991355,5.18181825589113,17.7663671861051));
#16766=CARTESIAN_POINT('Ctrl Pts',(-2.7147336133888,5.25980231512419,17.7585792083436));
#16767=CARTESIAN_POINT('Ctrl Pts',(-2.5656622379888,5.3315389751045,17.750791230582));
#16768=CARTESIAN_POINT('Ctrl Pts',(-2.41662017129931,5.4032615310424,17.7430047840037));
#16769=CARTESIAN_POINT('Ctrl Pts',(-2.26455110155002,5.4687390000518,17.7352183374254));
#16770=CARTESIAN_POINT('Ctrl Pts',(-2.10999700314931,5.52773400311565,17.7274318908471));
#16771=CARTESIAN_POINT('Ctrl Pts',(-1.95543700885806,5.58673125670591,17.7196451472334));
#16772=CARTESIAN_POINT('Ctrl Pts',(-1.7983920933421,5.63924543186964,17.7118584036196));
#16773=CARTESIAN_POINT('Ctrl Pts',(-1.63942326578623,5.68508767901594,17.7040716600059));
#16774=CARTESIAN_POINT('Ctrl Pts',(-1.4804649528289,5.73092689404058,17.696285431427));
#16775=CARTESIAN_POINT('Ctrl Pts',(-1.31958328957831,5.77009497571143,17.6884992028481));
#16776=CARTESIAN_POINT('Ctrl Pts',(-1.15735360853468,5.80245320423282,17.6807129742692));
#16777=CARTESIAN_POINT('Ctrl Pts',(-0.995081221110475,5.8348199509416,17.6729246959936));
#16778=CARTESIAN_POINT('Ctrl Pts',(-0.831460420009935,5.86037319790401,
17.665136417718));
#16779=CARTESIAN_POINT('Ctrl Pts',(-0.667076773500843,5.87902535636271,
17.6573481394424));
#16780=CARTESIAN_POINT('Ctrl Pts',(-0.510797081630046,5.89675798146596,
17.6499438157462));
#16781=CARTESIAN_POINT('Ctrl Pts',(-0.353828209411745,5.90825353161256,
17.64253949205));
#16782=CARTESIAN_POINT('Ctrl Pts',(-0.196677598010754,5.91348023459458,
17.6351351683539));
#16783=CARTESIAN_POINT('Ctrl Pts',(-0.03138424820307,5.91897775850903,17.6273471905923));
#16784=CARTESIAN_POINT('Ctrl Pts',(0.13416930302721,5.91754151518804,17.6195592128308));
#16785=CARTESIAN_POINT('Ctrl Pts',(0.299391421764328,5.90917044423952,17.6117712350693));
#16786=CARTESIAN_POINT('Ctrl Pts',(0.46458105641641,5.90080101911532,17.603984788491));
#16787=CARTESIAN_POINT('Ctrl Pts',(0.629439069648811,5.88549950300046,17.5961983419126));
#16788=CARTESIAN_POINT('Ctrl Pts',(0.793375984329712,5.86331690342496,17.5884118953343));
#16789=CARTESIAN_POINT('Ctrl Pts',(0.957319152834323,5.8411334576333,17.5806251517206));
#16790=CARTESIAN_POINT('Ctrl Pts',(1.12034083529254,5.8120684420466,17.5728384081069));
#16791=CARTESIAN_POINT('Ctrl Pts',(1.28185807155892,5.77622458417947,17.5650516644932));
#16792=CARTESIAN_POINT('Ctrl Pts',(1.44336462466847,5.74038309711538,17.5572654359143));
#16793=CARTESIAN_POINT('Ctrl Pts',(1.60336661875418,5.6977637343724,17.5494792073355));
#16794=CARTESIAN_POINT('Ctrl Pts',(1.76129251334702,5.64852009334549,17.5416929787566));
#16795=CARTESIAN_POINT('Ctrl Pts',(1.91925998136431,5.59926348910697,17.533904700481));
#16796=CARTESIAN_POINT('Ctrl Pts',(2.075149951966,5.54337921538932,17.5261164222055));
#16797=CARTESIAN_POINT('Ctrl Pts',(2.22840637247383,5.48107066198001,17.5183281439299));
#16798=CARTESIAN_POINT('Ctrl Pts',(2.37410739981275,5.42183385993508,17.5109238202338));
#16799=CARTESIAN_POINT('Ctrl Pts',(2.51742804099188,5.35679104072722,17.5035194965376));
#16800=CARTESIAN_POINT('Ctrl Pts',(2.65790755620268,5.28615720397916,17.4961151728415));
#16801=CARTESIAN_POINT('Ctrl Pts',(2.80566599914875,5.21186348420414,17.4883271950799));
#16802=CARTESIAN_POINT('Ctrl Pts',(2.95033393017463,5.13135739218281,17.4805392173184));
#16803=CARTESIAN_POINT('Ctrl Pts',(3.09139138928646,5.04492119271902,17.4727512395569));
#16804=CARTESIAN_POINT('Ctrl Pts',(3.23242111529251,4.95850198735309,17.4649647929786));
#16805=CARTESIAN_POINT('Ctrl Pts',(3.36984151344637,4.86615516773485,17.4571783464002));
#16806=CARTESIAN_POINT('Ctrl Pts',(3.50315944061564,4.76820768173174,17.4493918998219));
#16807=CARTESIAN_POINT('Ctrl Pts',(3.63648245356332,4.67025645925282,17.4416051562082));
#16808=CARTESIAN_POINT('Ctrl Pts',(3.76570242251492,4.56670432887035,17.4338184125945));
#16809=CARTESIAN_POINT('Ctrl Pts',(3.89035668289502,4.45792052894105,17.4260316689807));
#16810=CARTESIAN_POINT('Ctrl Pts',(4.01500269832836,4.34914392424628,17.4182454404019));
#16811=CARTESIAN_POINT('Ctrl Pts',(4.13508336880468,4.23513655268629,17.410459211823));
#16812=CARTESIAN_POINT('Ctrl Pts',(4.25017040593234,4.11630684996113,17.4026729832441));
#16813=CARTESIAN_POINT('Ctrl Pts',(4.36528773930906,3.99744586574364,17.3948847049685));
#16814=CARTESIAN_POINT('Ctrl Pts',(4.47540858871175,3.8737602420439,17.3870964266929));
#16815=CARTESIAN_POINT('Ctrl Pts',(4.58014209796389,3.74569471860147,17.3793081484173));
#16816=CARTESIAN_POINT('Ctrl Pts',(4.67971234659843,3.62394270148939,17.3719038247212));
#16817=CARTESIAN_POINT('Ctrl Pts',(4.77441347416384,3.49823243557518,17.3644995010251));
#16818=CARTESIAN_POINT('Ctrl Pts',(4.86394386608415,3.36897323083493,17.3570951773289));
#16819=CARTESIAN_POINT('Ctrl Pts',(4.95811326357019,3.23301647728081,17.3493071995674));
#16820=CARTESIAN_POINT('Ctrl Pts',(5.04659554326005,3.09308461064301,17.3415192218059));
#16821=CARTESIAN_POINT('Ctrl Pts',(5.12906929311559,2.94967434624888,17.3337312440443));
#16822=CARTESIAN_POINT('Ctrl Pts',(5.21152682792484,2.80629227754222,17.325944797466));
#16823=CARTESIAN_POINT('Ctrl Pts',(5.28797803079056,2.65943345246605,17.3181583508877));
#16824=CARTESIAN_POINT('Ctrl Pts',(5.35814642310363,2.50962098155912,17.3103719043093));
#16825=CARTESIAN_POINT('Ctrl Pts',(5.4283174921827,2.35980279564414,17.3025851606956));
#16826=CARTESIAN_POINT('Ctrl Pts',(5.49220513200002,2.20703102612777,17.2947984170819));
#16827=CARTESIAN_POINT('Ctrl Pts',(5.54957986708367,2.05185132535463,17.2870116734682));
#16828=CARTESIAN_POINT('Ctrl Pts',(5.60695080725784,1.89668188855775,17.2792254448893));
#16829=CARTESIAN_POINT('Ctrl Pts',(5.65780959403473,1.73910513900488,17.2714392163104));
#16830=CARTESIAN_POINT('Ctrl Pts',(5.70197569659381,1.57968468940912,17.2636529877316));
#16831=CARTESIAN_POINT('Ctrl Pts',(5.74615342572071,1.42022227295274,17.255864709456));
#16832=CARTESIAN_POINT('Ctrl Pts',(5.78363486287517,1.25891549426072,17.2480764311804));
#16833=CARTESIAN_POINT('Ctrl Pts',(5.81428972014246,1.096341923282,17.2402881529048));
#16834=CARTESIAN_POINT('Ctrl Pts',(5.84343332262229,0.941783071971193,17.2328838292087));
#16835=CARTESIAN_POINT('Ctrl Pts',(5.86640717020521,0.786079581818818,17.2254795055126));
#16836=CARTESIAN_POINT('Ctrl Pts',(5.88314236970594,0.629735198532512,17.2180751818164));
#16837=CARTESIAN_POINT('Ctrl Pts',(5.90074470138335,0.465289851443275,17.2102872040549));
#16838=CARTESIAN_POINT('Ctrl Pts',(5.91145100764235,0.30007660704057,17.2024992262934));
#16839=CARTESIAN_POINT('Ctrl Pts',(5.91521685128385,0.134685429009756,17.1947112485319));
#16840=CARTESIAN_POINT('Ctrl Pts',(5.91898195452821,-0.0306732316975447,
17.1869248019535));
#16841=CARTESIAN_POINT('Ctrl Pts',(5.9158093105734,-0.196209436959831,17.1791383553752));
#16842=CARTESIAN_POINT('Ctrl Pts',(5.90570656813228,-0.361331556356784,
17.1713519087969));
#16843=CARTESIAN_POINT('Ctrl Pts',(5.89560344029432,-0.526459974790323,
17.1635651651832));
#16844=CARTESIAN_POINT('Ctrl Pts',(5.87856970053289,-0.691173956565553,
17.1557784215695));
#16845=CARTESIAN_POINT('Ctrl Pts',(5.85466505616971,-0.854884578504832,
17.1479916779557));
#16846=CARTESIAN_POINT('Ctrl Pts',(5.8307619929199,-1.01858437221124,17.1402054493769));
#16847=CARTESIAN_POINT('Ctrl Pts',(5.79998898079507,-1.18128062268044,17.132419220798));
#16848=CARTESIAN_POINT('Ctrl Pts',(5.76245729738374,-1.34239206580227,17.1246329922191));
#16849=CARTESIAN_POINT('Ctrl Pts',(5.72491573389159,-1.5035459209327,17.1168447139435));
#16850=CARTESIAN_POINT('Ctrl Pts',(5.68061201454751,-1.66311382320429,17.109056435668));
#16851=CARTESIAN_POINT('Ctrl Pts',(5.62970821090074,-1.82052630374207,17.1012681573924));
#16852=CARTESIAN_POINT('Ctrl Pts',(5.58131391549526,-1.97017850137579,17.0938638336962));
#16853=CARTESIAN_POINT('Ctrl Pts',(5.52695469659419,-2.11788242765818,17.08645951));
#16854=CARTESIAN_POINT('Ctrl Pts',(5.46681119284299,-2.26316281877965,17.0790551863038));
#16855=CARTESIAN_POINT('Ctrl Pts',(5.40355136129935,-2.4159708943942,17.0712672085423));
#16856=CARTESIAN_POINT('Ctrl Pts',(5.33386927725262,-2.56615227900246,17.0634792307807));
#16857=CARTESIAN_POINT('Ctrl Pts',(5.25800832134371,-2.71316771600656,17.0556912530192));
#16858=CARTESIAN_POINT('Ctrl Pts',(5.18216228034909,-2.86015424851539,17.0479048064409));
#16859=CARTESIAN_POINT('Ctrl Pts',(5.10013993785626,-3.00397579159731,17.0401183598625));
#16860=CARTESIAN_POINT('Ctrl Pts',(5.01223120355831,-3.14411655709142,17.0323319132842));
#16861=CARTESIAN_POINT('Ctrl Pts',(4.92431911574033,-3.28426266863981,17.0245451696704));
#16862=CARTESIAN_POINT('Ctrl Pts',(4.83052035323439,-3.42072744883984,17.0167584260567));
#16863=CARTESIAN_POINT('Ctrl Pts',(4.73116923713355,-3.55302240523489,17.008971682443));
#16864=CARTESIAN_POINT('Ctrl Pts',(4.63182469236578,-3.68530861130829,17.0011854538641));
#16865=CARTESIAN_POINT('Ctrl Pts',(4.52692872091587,-3.81342529002623,16.9933992252852));
#16866=CARTESIAN_POINT('Ctrl Pts',(4.41685725623758,-3.9369153585671,16.9856129967063));
#16867=CARTESIAN_POINT('Ctrl Pts',(4.30675681564162,-4.06043793542488,16.9778247184307));
#16868=CARTESIAN_POINT('Ctrl Pts',(4.19147837070045,-4.17933122840309,16.9700364401551));
#16869=CARTESIAN_POINT('Ctrl Pts',(4.07143680578625,-4.29317282426285,16.9622481618795));
#16870=CARTESIAN_POINT('Ctrl Pts',(3.95731317381578,-4.40140213965138,16.9548438381835));
#16871=CARTESIAN_POINT('Ctrl Pts',(3.83888493462339,-4.50506566592638,16.9474395144874));
#16872=CARTESIAN_POINT('Ctrl Pts',(3.71653818153727,-4.6038325890149,16.9400351907913));
#16873=CARTESIAN_POINT('Ctrl Pts',(3.58785204741612,-4.7077171073262,16.9322472130298));
#16874=CARTESIAN_POINT('Ctrl Pts',(3.45478451019537,-4.80622127808978,16.9244592352683));
#16875=CARTESIAN_POINT('Ctrl Pts',(3.31780738170305,-4.89898813434129,16.9166712575068));
#16876=CARTESIAN_POINT('Ctrl Pts',(3.18085718408845,-4.9917367518336,16.9088848109284));
#16877=CARTESIAN_POINT('Ctrl Pts',(3.03999919332433,-5.07875012643922,16.9010983643501));
#16878=CARTESIAN_POINT('Ctrl Pts',(2.89573484000276,-5.15971416833279,16.8933119177718));
#16879=CARTESIAN_POINT('Ctrl Pts',(2.75146498332143,-5.24068129882199,16.8855251741581));
#16880=CARTESIAN_POINT('Ctrl Pts',(2.60378878077965,-5.31559847499263,16.8777384305444));
#16881=CARTESIAN_POINT('Ctrl Pts',(2.45323359045479,-5.38419683083413,16.8699516869307));
#16882=CARTESIAN_POINT('Ctrl Pts',(2.30268835822943,-5.4527906494076,16.8621654583518));
#16883=CARTESIAN_POINT('Ctrl Pts',(2.14926481014631,-5.51506635161638,16.8543792297729));
#16884=CARTESIAN_POINT('Ctrl Pts',(1.99351180501769,-5.57080256747222,16.846593001194));
#16885=CARTESIAN_POINT('Ctrl Pts',(1.83771779847005,-5.62655345568664,16.8388047229185));
#16886=CARTESIAN_POINT('Ctrl Pts',(1.67959340993951,-5.6757613080575,16.8310164446429));
#16887=CARTESIAN_POINT('Ctrl Pts',(1.51970510180609,-5.71825383889563,16.8232281663673));
#16888=CARTESIAN_POINT('Ctrl Pts',(1.3676991324811,-5.75865152909903,16.8158238426712));
#16889=CARTESIAN_POINT('Ctrl Pts',(1.21409922779002,-5.79297999829685,16.808419518975));
#16890=CARTESIAN_POINT('Ctrl Pts',(1.05940272615352,-5.82113360320123,16.8010151952788));
#16891=CARTESIAN_POINT('Ctrl Pts',(0.896690645486941,-5.85074598346707,
16.7932272175173));
#16892=CARTESIAN_POINT('Ctrl Pts',(0.732707105461285,-5.87353720371765,
16.7854392397558));
#16893=CARTESIAN_POINT('Ctrl Pts',(0.568037223561832,-5.88941968916702,
16.7776512619942));
#16894=CARTESIAN_POINT('Ctrl Pts',(0.403399717172985,-5.90529905198358,
16.7698648154159));
#16895=CARTESIAN_POINT('Ctrl Pts',(0.238076456035561,-5.91427235958073,
16.7620783688376));
#16896=CARTESIAN_POINT('Ctrl Pts',(0.0726580389161019,-5.91630386067863,
16.7542919222593));
#16897=CARTESIAN_POINT('Ctrl Pts',(-0.0927666885429905,-5.91833543927372,
16.7465051786456));
#16898=CARTESIAN_POINT('Ctrl Pts',(-0.258286259781496,-5.91342467359364,
16.7387184350319));
#16899=CARTESIAN_POINT('Ctrl Pts',(-0.423308958957855,-5.90158792934292,
16.7309316914181));
#16900=CARTESIAN_POINT('Ctrl Pts',(-0.588320743117305,-5.88975196800427,
16.7231454628393));
#16901=CARTESIAN_POINT('Ctrl Pts',(-0.752835402231415,-5.87099096780191,
16.7153592342604));
#16902=CARTESIAN_POINT('Ctrl Pts',(-0.916265077685874,-5.84537328747389,
16.7075730056815));
#16903=CARTESIAN_POINT('Ctrl Pts',(-1.07973777541529,-5.81974886338355,
16.6997847274059));
#16904=CARTESIAN_POINT('Ctrl Pts',(-1.24212460255152,-5.78726419999045,
16.6919964491304));
#16905=CARTESIAN_POINT('Ctrl Pts',(-1.40284573966221,-5.7480391781208,16.6842081708548));
#16906=CARTESIAN_POINT('Ctrl Pts',(-1.55564348030185,-5.71074791185695,
16.6768038471586));
#16907=CARTESIAN_POINT('Ctrl Pts',(-1.70693555258789,-5.66736492692143,
16.6693995234625));
#16908=CARTESIAN_POINT('Ctrl Pts',(-1.85623472721197,-5.61803552854486,
16.6619951997663));
#16909=CARTESIAN_POINT('Ctrl Pts',(-2.01326981907195,-5.56615013383342,
16.6542072220048));
#16910=CARTESIAN_POINT('Ctrl Pts',(-2.16815618118622,-5.50766717947198,
16.6464192442433));
#16911=CARTESIAN_POINT('Ctrl Pts',(-2.32033816334955,-5.44278985173997,
16.6386312664818));
#16912=CARTESIAN_POINT('Ctrl Pts',(-2.47249022523054,-5.37792527944679,
16.6308448199034));
#16913=CARTESIAN_POINT('Ctrl Pts',(-2.62193867429505,-5.30666896748374,
16.6230583733251));
#16914=CARTESIAN_POINT('Ctrl Pts',(-2.768147854012,-5.22927222668975,16.6152719267468));
#16915=CARTESIAN_POINT('Ctrl Pts',(-2.91436261127951,-5.15187253338459,
16.6074851831331));
#16916=CARTESIAN_POINT('Ctrl Pts',(-3.05733756767092,-5.06833208852439,
16.5996984395194));
#16917=CARTESIAN_POINT('Ctrl Pts',(-3.19656103256491,-4.97894849617744,
16.5919116959056));
#16918=CARTESIAN_POINT('Ctrl Pts',(-3.3357752888681,-4.88957081588652,16.5841254673268));
#16919=CARTESIAN_POINT('Ctrl Pts',(-3.47123828136255,-4.79435093426291,
16.5763392387479));
#16920=CARTESIAN_POINT('Ctrl Pts',(-3.60246659342468,-4.69363025873994,
16.568553010169));
#16921=CARTESIAN_POINT('Ctrl Pts',(-3.73372945086859,-4.59288306886093,
16.5607647318935));
#16922=CARTESIAN_POINT('Ctrl Pts',(-3.86075514549399,-4.48663238468414,
16.5529764536179));
#16923=CARTESIAN_POINT('Ctrl Pts',(-3.98309198098985,-4.37526100175456,
16.5451881753423));
#16924=CARTESIAN_POINT('Ctrl Pts',(-4.09939772892601,-4.26938012018846,
16.5377838516462));
#16925=CARTESIAN_POINT('Ctrl Pts',(-4.21146559885731,-4.1588714461052,16.53037952795));
#16926=CARTESIAN_POINT('Ctrl Pts',(-4.31893735809536,-4.04409577771697,
16.5229752042538));
#16927=CARTESIAN_POINT('Ctrl Pts',(-4.43197775250338,-3.92337302306,16.5151872264923));
#16928=CARTESIAN_POINT('Ctrl Pts',(-4.53997353380287,-3.79788616182981,
16.5073992487308));
#16929=CARTESIAN_POINT('Ctrl Pts',(-4.64253410177453,-3.66807956243599,
16.4996112709692));
#16930=CARTESIAN_POINT('Ctrl Pts',(-4.74507450545943,-3.53829848413223,
16.4918248243909));
#16931=CARTESIAN_POINT('Ctrl Pts',(-4.84218163002422,-3.40419961284222,
16.4840383778125));
#16932=CARTESIAN_POINT('Ctrl Pts',(-4.93350546527673,-3.26625999984457,
16.4762519312342));
#16933=CARTESIAN_POINT('Ctrl Pts',(-5.0248327843276,-3.12831512476175,16.4684651876205));
#16934=CARTESIAN_POINT('Ctrl Pts',(-5.1103761929086,-2.98652947904605,16.4606784440067));
#16935=CARTESIAN_POINT('Ctrl Pts',(-5.18982888186515,-2.8414092875646,16.452891700393));
#16936=CARTESIAN_POINT('Ctrl Pts',(-5.26927631562065,-2.69629869469827,
16.4451054718141));
#16937=CARTESIAN_POINT('Ctrl Pts',(-5.34263368255457,-2.54785427779887,
16.4373192432352));
#16938=CARTESIAN_POINT('Ctrl Pts',(-5.40963996521877,-2.39660718708926,
16.4295330146564));
#16939=CARTESIAN_POINT('Ctrl Pts',(-5.47666388704616,-2.24532028112637,
16.4217447363808));
#16940=CARTESIAN_POINT('Ctrl Pts',(-5.53733325248533,-2.09122951865049,
16.4139564581052));
#16941=CARTESIAN_POINT('Ctrl Pts',(-5.59143470554352,-1.93488720501827,
16.4061681798296));
#16942=CARTESIAN_POINT('Ctrl Pts',(-5.64286900933923,-1.78625241609988,
16.3987638561335));
#16943=CARTESIAN_POINT('Ctrl Pts',(-5.68836729864528,-1.63558297597227,
16.3913595324374));
#16944=CARTESIAN_POINT('Ctrl Pts',(-5.72778774878402,-1.48336713843192,
16.3839552087413));
#16945=CARTESIAN_POINT('Ctrl Pts',(-5.76973707593995,-1.32138644199592,
16.376075887323));
#16946=CARTESIAN_POINT('Ctrl Pts',(-5.8048168140385,-1.15760282851791,16.3681965659048));
#16947=CARTESIAN_POINT('Ctrl Pts',(-5.83289481012724,-0.99260702016997,
16.3603172444865));
#16948=CARTESIAN_POINT('Ctrl Pts',(-5.86096757812148,-0.827641933874796,
16.3524393901899));
#16949=CARTESIAN_POINT('Ctrl Pts',(-5.8820411538682,-0.661465402049517,
16.3445615358933));
#16950=CARTESIAN_POINT('Ctrl Pts',(-5.89603466904057,-0.494677414050429,
16.3366836815967));
#16951=CARTESIAN_POINT('Ctrl Pts',(-5.90983570702114,-0.330183551806171,
16.328914185154));
#16952=CARTESIAN_POINT('Ctrl Pts',(-5.9167501976856,-0.165095237549104,
16.3211446887113));
#16953=CARTESIAN_POINT('Ctrl Pts',(-5.91674999999576,7.08458452474372E-6,
16.3133751922686));
#16954=CARTESIAN_POINT('Ctrl Pts',(-5.91674999941157,-8.34454905555866E-5,
16.0616248078328));
#16955=CARTESIAN_POINT('Ctrl Pts',(-5.91674760998257,-0.16950726878363,
16.0695980559169));
#16956=CARTESIAN_POINT('Ctrl Pts',(-5.90946380488815,-0.338903242213537,
16.0775713040011));
#16957=CARTESIAN_POINT('Ctrl Pts',(-5.89493172683878,-0.507651946130016,
16.0855445520852));
#16958=CARTESIAN_POINT('Ctrl Pts',(-5.88039486884334,-0.676456155508387,
16.0935204227603));
#16959=CARTESIAN_POINT('Ctrl Pts',(-5.85860500012414,-0.844612385715935,
16.1014962934354));
#16960=CARTESIAN_POINT('Ctrl Pts',(-5.82964715749152,-1.01150609570632,
16.1094721641104));
#16961=CARTESIAN_POINT('Ctrl Pts',(-5.81959195123027,-1.06945760469643,
16.1122416737652));
#16962=CARTESIAN_POINT('Ctrl Pts',(-5.80867293760191,-1.12725695627872,
16.1150111834199));
#16963=CARTESIAN_POINT('Ctrl Pts',(-5.79689512537895,-1.18487867220983,
16.1177806930746));
#16964=CARTESIAN_POINT('Ctrl Pts',(-5.76377485320318,-1.34691614391897,
16.1255688044675));
#16965=CARTESIAN_POINT('Ctrl Pts',(-5.72385039390528,-1.50759298455844,
16.1333569158605));
#16966=CARTESIAN_POINT('Ctrl Pts',(-5.67725841384133,-1.66633353953158,
16.1411450272535));
#16967=CARTESIAN_POINT('Ctrl Pts',(-5.63067558130054,-1.82504292856367,
16.1489316095865));
#16968=CARTESIAN_POINT('Ctrl Pts',(-5.57742792987381,-1.98181648404794,
16.1567181919195));
#16969=CARTESIAN_POINT('Ctrl Pts',(-5.51770226209812,-2.13609276702518,
16.1645047742525));
#16970=CARTESIAN_POINT('Ctrl Pts',(-5.45797431699597,-2.29037493252289,
16.1722916534862));
#16971=CARTESIAN_POINT('Ctrl Pts',(-5.39176797295808,-2.4421593355855,16.1800785327199));
#16972=CARTESIAN_POINT('Ctrl Pts',(-5.31931881544833,-2.59090291252245,
16.1878654119536));
#16973=CARTESIAN_POINT('Ctrl Pts',(-5.24687443954099,-2.73963667246955,
16.1956517772578));
#16974=CARTESIAN_POINT('Ctrl Pts',(-5.16818821471741,-2.88532972067255,
16.203438142562));
#16975=CARTESIAN_POINT('Ctrl Pts',(-5.0835425418119,-3.02746193833855,16.2112245078661));
#16976=CARTESIAN_POINT('Ctrl Pts',(-4.99887464267158,-3.16963147703863,
16.2190129177117));
#16977=CARTESIAN_POINT('Ctrl Pts',(-4.90824433052758,-3.30823804116743,
16.2268013275573));
#16978=CARTESIAN_POINT('Ctrl Pts',(-4.81197882630275,-3.44278816335163,
16.2345897374029));
#16979=CARTESIAN_POINT('Ctrl Pts',(-4.7207722628896,-3.57026741305853,16.2419688510552));
#16980=CARTESIAN_POINT('Ctrl Pts',(-4.62450770574258,-3.69410539135892,
16.2493479647074));
#16981=CARTESIAN_POINT('Ctrl Pts',(-4.52349819239377,-3.81390805682443,
16.2567270783597));
#16982=CARTESIAN_POINT('Ctrl Pts',(-4.41689008486494,-3.94035095332748,
16.2645151897527));
#16983=CARTESIAN_POINT('Ctrl Pts',(-4.30495803919303,-4.06234368556955,
16.2723033011456));
#16984=CARTESIAN_POINT('Ctrl Pts',(-4.18809747868372,-4.17944614411325,
16.2800914125386));
#16985=CARTESIAN_POINT('Ctrl Pts',(-4.07125986170831,-4.29652561163057,
16.2878779948716));
#16986=CARTESIAN_POINT('Ctrl Pts',(-3.94949588616863,-4.4087164951398,16.2956645772047));
#16987=CARTESIAN_POINT('Ctrl Pts',(-3.82323819983297,-4.51561515519624,
16.3034511595377));
#16988=CARTESIAN_POINT('Ctrl Pts',(-3.69697569931977,-4.62251789127485,
16.3112380387714));
#16989=CARTESIAN_POINT('Ctrl Pts',(-3.56621938645127,-4.72412779064063,
16.3190249180052));
#16990=CARTESIAN_POINT('Ctrl Pts',(-3.43143595502093,-4.8200806890642,16.3268117972389));
#16991=CARTESIAN_POINT('Ctrl Pts',(-3.29666141921912,-4.91602725465195,
16.3345981625431));
#16992=CARTESIAN_POINT('Ctrl Pts',(-3.15786055712963,-5.00631738121599,
16.3423845278472));
#16993=CARTESIAN_POINT('Ctrl Pts',(-3.0155301945431,-5.09062945108941,16.3501708931514));
#16994=CARTESIAN_POINT('Ctrl Pts',(-2.87316245889367,-5.17496365960025,
16.357959302997));
#16995=CARTESIAN_POINT('Ctrl Pts',(-2.72726364496336,-5.2533165101719,16.3657477128426));
#16996=CARTESIAN_POINT('Ctrl Pts',(-2.57835718510673,-5.32541123186825,
16.3735361226882));
#16997=CARTESIAN_POINT('Ctrl Pts',(-2.43727605139484,-5.39371723471968,
16.3809152363404));
#16998=CARTESIAN_POINT('Ctrl Pts',(-2.2934954905747,-5.45640583146567,16.3882943499926));
#16999=CARTESIAN_POINT('Ctrl Pts',(-2.14747891136345,-5.51328077352761,
16.3956734636448));
#17000=CARTESIAN_POINT('Ctrl Pts',(-1.99336915811693,-5.57330808915453,
16.4034615750378));
#17001=CARTESIAN_POINT('Ctrl Pts',(-1.83671344877192,-5.62688045421262,
16.4112496864308));
#17002=CARTESIAN_POINT('Ctrl Pts',(-1.67806957743404,-5.67380058301227,
16.4190377978238));
#17003=CARTESIAN_POINT('Ctrl Pts',(-1.51945685305472,-5.72071149986257,
16.4268243801568));
#17004=CARTESIAN_POINT('Ctrl Pts',(-1.35885705174777,-5.76097269584713,
16.4346109624899));
#17005=CARTESIAN_POINT('Ctrl Pts',(-1.19684320673853,-5.79443671990504,
16.442397544823));
#17006=CARTESIAN_POINT('Ctrl Pts',(-1.03482318417745,-5.82790201993873,
16.4501844240567));
#17007=CARTESIAN_POINT('Ctrl Pts',(-0.871389322137765,-5.85456956093857,
16.4579713032905));
#17008=CARTESIAN_POINT('Ctrl Pts',(-0.707125664101611,-5.87434284475028,
16.4657581825242));
#17009=CARTESIAN_POINT('Ctrl Pts',(-0.542872847371819,-5.89411482353671,
16.4735445478284));
#17010=CARTESIAN_POINT('Ctrl Pts',(-0.377790661517953,-5.90699341762036,
16.4813309131326));
#17011=CARTESIAN_POINT('Ctrl Pts',(-0.212469253840867,-5.91293390616471,
16.4891172784368));
#17012=CARTESIAN_POINT('Ctrl Pts',(-0.0471044361194315,-5.91887595456072,
16.4969056882824));
#17013=CARTESIAN_POINT('Ctrl Pts',(0.118499409479502,-5.91787624364827,
16.504694098128));
#17014=CARTESIAN_POINT('Ctrl Pts',(0.283750228081456,-5.90994216304726,
16.5124825079736));
#17015=CARTESIAN_POINT('Ctrl Pts',(0.440316792469277,-5.90242503392326,
16.5198616216258));
#17016=CARTESIAN_POINT('Ctrl Pts',(0.596566220247805,-5.88868363115203,
16.5272407352779));
#17017=CARTESIAN_POINT('Ctrl Pts',(0.751997689404057,-5.86876733544881,
16.53461984893));
#17018=CARTESIAN_POINT('Ctrl Pts',(0.916044166098635,-5.84774715107652,
16.542407960323));
#17019=CARTESIAN_POINT('Ctrl Pts',(1.0792380289808,-5.81984065208844,16.5501960717159));
#17020=CARTESIAN_POINT('Ctrl Pts',(1.24099507788301,-5.78514146578717,16.5579841831089));
#17021=CARTESIAN_POINT('Ctrl Pts',(1.40272036860826,-5.7504490920663,16.5657707654419));
#17022=CARTESIAN_POINT('Ctrl Pts',(1.56300909598557,-5.70896675898949,16.573557347775));
#17023=CARTESIAN_POINT('Ctrl Pts',(1.72128752067219,-5.66083914571666,16.581343930108));
#17024=CARTESIAN_POINT('Ctrl Pts',(1.87957198048011,-5.6127096973486,16.5891308093417));
#17025=CARTESIAN_POINT('Ctrl Pts',(2.03584567737109,-5.55793455094008,16.5969176885754));
#17026=CARTESIAN_POINT('Ctrl Pts',(2.18954958131189,-5.49670839625652,16.6047045678091));
#17027=CARTESIAN_POINT('Ctrl Pts',(2.343243340884,-5.43548628246374,16.6124909331133));
#17028=CARTESIAN_POINT('Ctrl Pts',(2.49436735008731,-5.36781413077603,16.6202772984175));
#17029=CARTESIAN_POINT('Ctrl Pts',(2.64238199108072,-5.29393501808554,16.6280636637217));
#17030=CARTESIAN_POINT('Ctrl Pts',(2.79043549771314,-5.22003650624031,16.6358520735673));
#17031=CARTESIAN_POINT('Ctrl Pts',(2.9353777177355,-5.13992791772467,16.6436404834128));
#17032=CARTESIAN_POINT('Ctrl Pts',(3.0766922897027,-5.05389900146253,16.6514288932584));
#17033=CARTESIAN_POINT('Ctrl Pts',(3.21058050410514,-4.97239107326396,16.6588080069107));
#17034=CARTESIAN_POINT('Ctrl Pts',(3.34121232160782,-4.88556919763453,16.6661871205629));
#17035=CARTESIAN_POINT('Ctrl Pts',(3.46817158444463,-4.79371634781938,16.6735662342151));
#17036=CARTESIAN_POINT('Ctrl Pts',(3.60216774278325,-4.6967724247635,16.6813543456081));
#17037=CARTESIAN_POINT('Ctrl Pts',(3.73212054572166,-4.59418939216722,16.689142457001));
#17038=CARTESIAN_POINT('Ctrl Pts',(3.85756178836071,-4.4863289682634,16.696930568394));
#17039=CARTESIAN_POINT('Ctrl Pts',(3.98297840279855,-4.37848972087351,16.704717150727));
#17040=CARTESIAN_POINT('Ctrl Pts',(4.10388498217366,-4.2653753577464,16.7125037330601));
#17041=CARTESIAN_POINT('Ctrl Pts',(4.21984693248474,-4.14738742208865,16.7202903153932));
#17042=CARTESIAN_POINT('Ctrl Pts',(4.33581330439915,-4.0293949875772,16.7280771946269));
#17043=CARTESIAN_POINT('Ctrl Pts',(4.44683444320285,-3.90652883380487,16.7358640738606));
#17044=CARTESIAN_POINT('Ctrl Pts',(4.55251259831223,-3.77922738198013,16.7436509530943));
#17045=CARTESIAN_POINT('Ctrl Pts',(4.6581837787245,-3.65193433197759,16.7514373183985));
#17046=CARTESIAN_POINT('Ctrl Pts',(4.75851247709818,-3.52020681566315,16.7592236837026));
#17047=CARTESIAN_POINT('Ctrl Pts',(4.85314113924644,-3.3845164566085,16.7670100490068));
#17048=CARTESIAN_POINT('Ctrl Pts',(4.94779464895975,-3.24879046802104,16.7747984588524));
#17049=CARTESIAN_POINT('Ctrl Pts',(5.03674494721138,-3.10909981858482,16.782586868698));
#17050=CARTESIAN_POINT('Ctrl Pts',(5.11967723133251,-2.96594598896802,16.7903752785436));
#17051=CARTESIAN_POINT('Ctrl Pts',(5.19825126147458,-2.83031517350858,16.7977543921958));
#17052=CARTESIAN_POINT('Ctrl Pts',(5.27142339532634,-2.69157603462084,16.805133505848));
#17053=CARTESIAN_POINT('Ctrl Pts',(5.33896357963309,-2.55017616212124,16.8125126195002));
#17054=CARTESIAN_POINT('Ctrl Pts',(5.41024727353926,-2.40093900304194,16.8203007308932));
#17055=CARTESIAN_POINT('Ctrl Pts',(5.47528245591269,-2.24868449696134,16.8280888422862));
#17056=CARTESIAN_POINT('Ctrl Pts',(5.5338310441021,-2.09395428265087,16.8358769536791));
#17057=CARTESIAN_POINT('Ctrl Pts',(5.59236813729686,-1.93925444692065,16.8436635360122));
#17058=CARTESIAN_POINT('Ctrl Pts',(5.64442106436579,-1.7820801714638,16.8514501183452));
#17059=CARTESIAN_POINT('Ctrl Pts',(5.68980031082602,-1.6229919856315,16.8592367006783));
#17060=CARTESIAN_POINT('Ctrl Pts',(5.73518128758682,-1.4638977338021,16.867023579912));
#17061=CARTESIAN_POINT('Ctrl Pts',(5.77388798311082,-1.30288973174729,16.8748104591457));
#17062=CARTESIAN_POINT('Ctrl Pts',(5.8057808796978,-1.14054326504322,16.8825973383794));
#17063=CARTESIAN_POINT('Ctrl Pts',(5.83767167137206,-0.978207513112043,
16.8903837036836));
#17064=CARTESIAN_POINT('Ctrl Pts',(5.86274950255863,-0.814533786892136,
16.8981700689878));
#17065=CARTESIAN_POINT('Ctrl Pts',(5.88092603811226,-0.650107296339016,
16.905956434292));
#17066=CARTESIAN_POINT('Ctrl Pts',(5.89910734645501,-0.485637630728497,
16.9137448441376));
#17067=CARTESIAN_POINT('Ctrl Pts',(5.91038370107013,-0.320415123407121,
16.9215332539832));
#17068=CARTESIAN_POINT('Ctrl Pts',(5.91471859258403,-0.155030748694557,
16.9293216638288));
#17069=CARTESIAN_POINT('Ctrl Pts',(5.91882567705765,0.00166235317050914,
16.936700777481));
#17070=CARTESIAN_POINT('Ctrl Pts',(5.91670210155318,0.158500487113797,16.9440798911332));
#17071=CARTESIAN_POINT('Ctrl Pts',(5.90835999380824,0.314980548711032,16.9514590047854));
#17072=CARTESIAN_POINT('Ctrl Pts',(5.89955551302207,0.48013373755449,16.9592471161784));
#17073=CARTESIAN_POINT('Ctrl Pts',(5.88382046641899,0.644947019412175,16.9670352275714));
#17074=CARTESIAN_POINT('Ctrl Pts',(5.86120492727678,0.808830861779118,16.9748233389643));
#17075=CARTESIAN_POINT('Ctrl Pts',(5.83859382830144,0.9726825284105,16.9826099212974));
#17076=CARTESIAN_POINT('Ctrl Pts',(5.80910497581698,1.13560480331814,16.9903965036305));
#17077=CARTESIAN_POINT('Ctrl Pts',(5.77284012983798,1.29701480247227,16.9981830859636));
#17078=CARTESIAN_POINT('Ctrl Pts',(5.73657390108848,1.45843095615374,17.0059699651973));
#17079=CARTESIAN_POINT('Ctrl Pts',(5.69353122804064,1.61833440608861,17.013756844431));
#17080=CARTESIAN_POINT('Ctrl Pts',(5.64386483392354,1.77615323069302,17.0215437236647));
#17081=CARTESIAN_POINT('Ctrl Pts',(5.5942017177597,1.93396163934636,17.0293300889689));
#17082=CARTESIAN_POINT('Ctrl Pts',(5.53791585139387,2.08968539321618,17.0371164542731));
#17083=CARTESIAN_POINT('Ctrl Pts',(5.475209650798,2.24276834343373,17.0449028195773));
#17084=CARTESIAN_POINT('Ctrl Pts',(5.41248698482726,2.39589149012528,17.0526912294229));
#17085=CARTESIAN_POINT('Ctrl Pts',(5.34334073534985,2.54637215095016,17.0604796392685));
#17086=CARTESIAN_POINT('Ctrl Pts',(5.26802158560594,2.69367391049657,17.0682680491141));
#17087=CARTESIAN_POINT('Ctrl Pts',(5.19666060471776,2.83323467404113,17.0756471627663));
#17088=CARTESIAN_POINT('Ctrl Pts',(5.11975895061818,2.96994182611438,17.0830262764184));
#17089=CARTESIAN_POINT('Ctrl Pts',(5.03756797584835,3.10335938157461,17.0904053900705));
#17090=CARTESIAN_POINT('Ctrl Pts',(4.9508214508346,3.24417179248001,17.0981935014635));
#17091=CARTESIAN_POINT('Ctrl Pts',(4.85815166126487,3.38136989621794,17.1059816128564));
#17092=CARTESIAN_POINT('Ctrl Pts',(4.75988463076687,3.51445996766066,17.1137697242494));
#17093=CARTESIAN_POINT('Ctrl Pts',(4.66163689328724,3.64752390918798,17.1215563065824));
#17094=CARTESIAN_POINT('Ctrl Pts',(4.55779429723068,3.77648117081394,17.1293428889155));
#17095=CARTESIAN_POINT('Ctrl Pts',(4.44872507266335,3.9008685943462,17.1371294712485));
#17096=CARTESIAN_POINT('Ctrl Pts',(4.3396516893108,4.02526076074319,17.1449163504822));
#17097=CARTESIAN_POINT('Ctrl Pts',(4.22535148635334,4.14508249753556,17.152703229716));
#17098=CARTESIAN_POINT('Ctrl Pts',(4.10623220099838,4.25990465550392,17.1604901089497));
#17099=CARTESIAN_POINT('Ctrl Pts',(3.98712077744725,4.37471923527638,17.1682764742538));
#17100=CARTESIAN_POINT('Ctrl Pts',(3.8631911381307,4.48453467485856,17.176062839558));
#17101=CARTESIAN_POINT('Ctrl Pts',(3.73488711036484,4.58895945017284,17.1838492048622));
#17102=CARTESIAN_POINT('Ctrl Pts',(3.60654939256685,4.69341164531248,17.1916376147078));
#17103=CARTESIAN_POINT('Ctrl Pts',(3.47383523788627,4.79247014442481,17.1994260245534));
#17104=CARTESIAN_POINT('Ctrl Pts',(3.33722141704751,4.88578384459438,17.207214434399));
#17105=CARTESIAN_POINT('Ctrl Pts',(3.20778692009416,4.97419372703635,17.2145935480512));
#17106=CARTESIAN_POINT('Ctrl Pts',(3.0748522998765,5.05744693465817,17.2219726617034));
#17107=CARTESIAN_POINT('Ctrl Pts',(2.93884686546465,5.13528087487419,17.2293517753556));
#17108=CARTESIAN_POINT('Ctrl Pts',(2.79530313878258,5.2174288705721,17.2371398867486));
#17109=CARTESIAN_POINT('Ctrl Pts',(2.64828727028938,5.29356916200429,17.2449279981415));
#17110=CARTESIAN_POINT('Ctrl Pts',(2.49832176428621,5.36342417906638,17.2527161095345));
#17111=CARTESIAN_POINT('Ctrl Pts',(2.34838570139589,5.43326548131361,17.2605026918675));
#17112=CARTESIAN_POINT('Ctrl Pts',(2.1955014459598,5.49682383655954,17.2682892742006));
#17113=CARTESIAN_POINT('Ctrl Pts',(2.04021394041632,5.55386870927202,17.2760758565336));
#17114=CARTESIAN_POINT('Ctrl Pts',(1.88492051379484,5.6109157570928,17.2838627357674));
#17115=CARTESIAN_POINT('Ctrl Pts',(1.72722395226152,5.66144871153472,17.2916496150011));
#17116=CARTESIAN_POINT('Ctrl Pts',(1.56768761928538,5.7052858027306,17.2994364942348));
#17117=CARTESIAN_POINT('Ctrl Pts',(1.40816181561484,5.74912000070385,17.3072228595389));
#17118=CARTESIAN_POINT('Ctrl Pts',(1.24679679165303,5.78625913523272,17.3150092248431));
#17119=CARTESIAN_POINT('Ctrl Pts',(1.08416960122261,5.81657174272654,17.3227955901473));
#17120=CARTESIAN_POINT('Ctrl Pts',(0.921499708194478,5.84689230969552,17.3305839999929));
#17121=CARTESIAN_POINT('Ctrl Pts',(0.757567300422326,5.8703827073296,17.3383724098385));
#17122=CARTESIAN_POINT('Ctrl Pts',(0.592959021178191,5.88696272807153,17.3461608196841));
#17123=CARTESIAN_POINT('Ctrl Pts',(0.437001229444464,5.90267143624639,17.3535399333363));
#17124=CARTESIAN_POINT('Ctrl Pts',(0.280437034654325,5.91217736815578,17.3609190469885));
#17125=CARTESIAN_POINT('Ctrl Pts',(0.123769056454859,5.91545533185437,17.3682981606407));
#17126=CARTESIAN_POINT('Ctrl Pts',(-0.0415824645321675,5.91891498129602,
17.3760862720337));
#17127=CARTESIAN_POINT('Ctrl Pts',(-0.207108654925602,5.91543793340395,
17.3838743834266));
#17128=CARTESIAN_POINT('Ctrl Pts',(-0.372217892445571,5.9050304320167,17.3916624948196));
#17129=CARTESIAN_POINT('Ctrl Pts',(-0.537294713644905,5.89462497396093,
17.3994490771526));
#17130=CARTESIAN_POINT('Ctrl Pts',(-0.701954426610032,5.87729179744747,
17.4072356594857));
#17131=CARTESIAN_POINT('Ctrl Pts',(-0.865608208618556,5.85308918364245,
17.4150222418188));
#17132=CARTESIAN_POINT('Ctrl Pts',(-1.02926823070942,5.82888564699714,17.4228091210525));
#17133=CARTESIAN_POINT('Ctrl Pts',(-1.19192192843783,5.79781219177657,17.4305960002862));
#17134=CARTESIAN_POINT('Ctrl Pts',(-1.35298763436772,5.7599787346611,17.4383828795199));
#17135=CARTESIAN_POINT('Ctrl Pts',(-1.51404271005432,5.72214777453188,17.4461692448241));
#17136=CARTESIAN_POINT('Ctrl Pts',(-1.67350969261694,5.67755777852217,17.4539556101283));
#17137=CARTESIAN_POINT('Ctrl Pts',(-1.83081896110411,5.62636938834998,17.4617419754324));
#17138=CARTESIAN_POINT('Ctrl Pts',(-1.98816953581057,5.57516755714605,17.469530385278));
#17139=CARTESIAN_POINT('Ctrl Pts',(-2.14336095966549,5.51736396676577,17.4773187951236));
#17140=CARTESIAN_POINT('Ctrl Pts',(-2.29583971369687,5.45316885595085,17.4851072049692));
#17141=CARTESIAN_POINT('Ctrl Pts',(-2.44030541052709,5.39234732395523,17.4924863186214));
#17142=CARTESIAN_POINT('Ctrl Pts',(-2.58233597682478,5.32578886792703,17.4998654322736));
#17143=CARTESIAN_POINT('Ctrl Pts',(-2.72147799808978,5.25371183720741,17.5072445459258));
#17144=CARTESIAN_POINT('Ctrl Pts',(-2.86833216135817,5.17763983580216,17.5150326573188));
#17145=CARTESIAN_POINT('Ctrl Pts',(-3.01202094520114,5.09539299412413,17.5228207687118));
#17146=CARTESIAN_POINT('Ctrl Pts',(-3.1520278198626,5.00725984799194,17.5306088801048));
#17147=CARTESIAN_POINT('Ctrl Pts',(-3.2920072066145,4.91914400526685,17.5383954624378));
#17148=CARTESIAN_POINT('Ctrl Pts',(-3.42830585629749,4.82514433411655,17.5461820447709));
#17149=CARTESIAN_POINT('Ctrl Pts',(-3.56043459400334,4.72559372611784,17.5539686271039));
#17150=CARTESIAN_POINT('Ctrl Pts',(-3.69256836974889,4.62603932227635,17.5617555063376));
#17151=CARTESIAN_POINT('Ctrl Pts',(-3.82053165779555,4.52093374717946,17.5695423855714));
#17152=CARTESIAN_POINT('Ctrl Pts',(-3.94386627070621,4.41065181138638,17.5773292648051));
#17153=CARTESIAN_POINT('Ctrl Pts',(-4.06719274360384,4.30037715413719,17.5851156301093));
#17154=CARTESIAN_POINT('Ctrl Pts',(-4.18589091456465,4.1849270329488,17.5929019954135));
#17155=CARTESIAN_POINT('Ctrl Pts',(-4.29953744309141,4.06471503773081,17.6006883607177));
#17156=CARTESIAN_POINT('Ctrl Pts',(-4.41321381288865,3.94447147728412,17.6084767705633));
#17157=CARTESIAN_POINT('Ctrl Pts',(-4.52183566864467,3.81946377531669,17.6162651804089));
#17158=CARTESIAN_POINT('Ctrl Pts',(-4.62501753834308,3.69014137026198,17.6240535902545));
#17159=CARTESIAN_POINT('Ctrl Pts',(-4.72277699867455,3.56761511091167,17.6314327039067));
#17160=CARTESIAN_POINT('Ctrl Pts',(-4.81565336853743,3.44121617993303,17.6388118175589));
#17161=CARTESIAN_POINT('Ctrl Pts',(-4.90335296033389,3.31135324435266,17.646190931211));
#17162=CARTESIAN_POINT('Ctrl Pts',(-4.99591342521148,3.17429247312825,17.653979042604));
#17163=CARTESIAN_POINT('Ctrl Pts',(-5.0827400368267,3.03332386285053,17.661767153997));
#17164=CARTESIAN_POINT('Ctrl Pts',(-5.16351726432063,2.88894790945818,17.6695552653899));
#17165=CARTESIAN_POINT('Ctrl Pts',(-5.24427863261406,2.7446003017675,17.677341847723));
#17166=CARTESIAN_POINT('Ctrl Pts',(-5.31899283066456,2.59684696443971,17.685128430056));
#17167=CARTESIAN_POINT('Ctrl Pts',(-5.38738956988842,2.44621425569338,17.6929150123891));
#17168=CARTESIAN_POINT('Ctrl Pts',(-5.45578891706479,2.29557580335522,17.7007018916228));
#17169=CARTESIAN_POINT('Ctrl Pts',(-5.51787018771155,2.14205804920599,17.7084887708565));
#17170=CARTESIAN_POINT('Ctrl Pts',(-5.5734103595701,1.98620933598065,17.7162756500902));
#17171=CARTESIAN_POINT('Ctrl Pts',(-5.62894686580935,1.83037090868046,17.7240620153944));
#17172=CARTESIAN_POINT('Ctrl Pts',(-5.6779430300153,1.6722021312153,17.7318483806986));
#17173=CARTESIAN_POINT('Ctrl Pts',(-5.72022498323144,1.51226872734805,17.7396347460028));
#17174=CARTESIAN_POINT('Ctrl Pts',(-5.7625180388299,1.35229332821658,17.7474231558484));
#17175=CARTESIAN_POINT('Ctrl Pts',(-5.79809327696699,1.19055268542543,17.755211565694));
#17176=CARTESIAN_POINT('Ctrl Pts',(-5.82682723306159,1.02762588452792,17.7629999755396));
#17177=CARTESIAN_POINT('Ctrl Pts',(-5.85405116347902,0.873261206160452,
17.7703790891917));
#17178=CARTESIAN_POINT('Ctrl Pts',(-5.87513431802023,0.717832089112757,
17.7777582028439));
#17179=CARTESIAN_POINT('Ctrl Pts',(-5.89001432361835,0.561837903732653,
17.7851373164961));
#17180=CARTESIAN_POINT('Ctrl Pts',(-5.9067386364072,0.386508967709382,17.7934310368183));
#17181=CARTESIAN_POINT('Ctrl Pts',(-5.91563053670214,0.210427895121147,
17.8017247571405));
#17182=CARTESIAN_POINT('Ctrl Pts',(-5.91665077471695,0.0342662011513159,
17.8100184774627));
#17183=CARTESIAN_POINT('Ctrl Pts',(-5.91671664138899,0.0228931839191246,
17.8105539209068));
#17184=CARTESIAN_POINT('Ctrl Pts',(-5.91674971691492,0.0115198317854237,
17.811089364351));
#17185=CARTESIAN_POINT('Ctrl Pts',(-5.91674999819062,0.000146325857716349,
17.8116248077951));
#17186=CARTESIAN_POINT('Origin',(0.,0.,0.));
#17187=CARTESIAN_POINT('',(-5.91674999855416,-0.000130802689547563,19.8133751922466));
#17188=CARTESIAN_POINT('',(-5.91674999805254,-0.000151806595337599,19.5616248077951));
#17189=CARTESIAN_POINT('',(-5.91675,-7.2459289488551E-16,0.));
#17190=CARTESIAN_POINT('Ctrl Pts',(-5.91674999855418,-0.000130801803848009,
19.8133751922049));
#17191=CARTESIAN_POINT('Ctrl Pts',(-5.91675365556631,0.165292196264256,
19.8055894898337));
#17192=CARTESIAN_POINT('Ctrl Pts',(-5.90981551862249,0.33072426090592,19.7978037874625));
#17193=CARTESIAN_POINT('Ctrl Pts',(-5.89595937446898,0.495574027882227,
19.7900180850912));
#17194=CARTESIAN_POINT('Ctrl Pts',(-5.8821040729587,0.660413769736061,19.7822328561973));
#17195=CARTESIAN_POINT('Ctrl Pts',(-5.86133163332367,0.824670966230145,
19.7744476273033));
#17196=CARTESIAN_POINT('Ctrl Pts',(-5.83371778357321,0.987758768182621,
19.7666623984094));
#17197=CARTESIAN_POINT('Ctrl Pts',(-5.80609621641889,1.15089214923559,19.7588749937321));
#17198=CARTESIAN_POINT('Ctrl Pts',(-5.77162946994277,1.31285516693262,19.7510875890547));
#17199=CARTESIAN_POINT('Ctrl Pts',(-5.73044469308286,1.47306964601761,19.7433001843774));
#17200=CARTESIAN_POINT('Ctrl Pts',(-5.6901362979207,1.6298748790683,19.7356784899321));
#17201=CARTESIAN_POINT('Ctrl Pts',(-5.64339299006378,1.78500495803461,19.7280567954869));
#17202=CARTESIAN_POINT('Ctrl Pts',(-5.59038061120507,1.93793064487932,19.7204351010416));
#17203=CARTESIAN_POINT('Ctrl Pts',(-5.53621165565258,2.09419272765823,19.7126471232801));
#17204=CARTESIAN_POINT('Ctrl Pts',(-5.47547716308906,2.24821013749588,19.7048591455185));
#17205=CARTESIAN_POINT('Ctrl Pts',(-5.40838839782343,2.39943024503503,19.697071167757));
#17206=CARTESIAN_POINT('Ctrl Pts',(-5.34131282278406,2.55062062140498,19.6892847211786));
#17207=CARTESIAN_POINT('Ctrl Pts',(-5.26788559728104,2.69901450092035,19.6814982746002));
#17208=CARTESIAN_POINT('Ctrl Pts',(-5.1883658136253,2.8440799472772,19.6737118280218));
#17209=CARTESIAN_POINT('Ctrl Pts',(-5.10884299646939,2.98915092755322,19.6659250844081));
#17210=CARTESIAN_POINT('Ctrl Pts',(-5.02322730621899,3.13089293849438,19.6581383407944));
#17211=CARTESIAN_POINT('Ctrl Pts',(-4.93182377414891,3.2687986819686,19.6503515971806));
#17212=CARTESIAN_POINT('Ctrl Pts',(-4.8404262877386,3.40669530400968,19.6425653686017));
#17213=CARTESIAN_POINT('Ctrl Pts',(-4.74324190224314,3.54075590004021,19.6347791400228));
#17214=CARTESIAN_POINT('Ctrl Pts',(-4.64061903550317,3.67050208143595,19.6269929114439));
#17215=CARTESIAN_POINT('Ctrl Pts',(-4.53796915366221,3.80028241804782,19.6192046331684));
#17216=CARTESIAN_POINT('Ctrl Pts',(-4.42987812665055,3.9257458185392,19.6114163548928));
#17217=CARTESIAN_POINT('Ctrl Pts',(-4.31673529364155,4.04644621453559,19.6036280766172));
#17218=CARTESIAN_POINT('Ctrl Pts',(-4.20917029277264,4.16119619785267,19.5962237529212));
#17219=CARTESIAN_POINT('Ctrl Pts',(-4.09703976589781,4.27164129489342,19.5888194292251));
#17220=CARTESIAN_POINT('Ctrl Pts',(-3.98070969479159,4.37742857032439,19.5814151055291));
#17221=CARTESIAN_POINT('Ctrl Pts',(-3.85835199624035,4.48869719961906,19.5736271277676));
#17222=CARTESIAN_POINT('Ctrl Pts',(-3.73130423174891,4.59485230622068,19.5658391500061));
#17223=CARTESIAN_POINT('Ctrl Pts',(-3.60001641622602,4.69550980889223,19.5580511722446));
#17224=CARTESIAN_POINT('Ctrl Pts',(-3.468754413013,4.79614752143597,19.5502647256662));
#17225=CARTESIAN_POINT('Ctrl Pts',(-3.33325427554463,4.89128959240634,19.5424782790879));
#17226=CARTESIAN_POINT('Ctrl Pts',(-3.19399810645238,4.98059300269342,19.5346918325095));
#17227=CARTESIAN_POINT('Ctrl Pts',(-3.05473662505157,5.06989981970404,19.5269050888958));
#17228=CARTESIAN_POINT('Ctrl Pts',(-2.91171909215923,5.15336735451814,19.5191183452821));
#17229=CARTESIAN_POINT('Ctrl Pts',(-2.76545615116162,5.23069620973178,19.5113316016684));
#17230=CARTESIAN_POINT('Ctrl Pts',(-2.61920288436343,5.3080199502201,19.5035453730895));
#17231=CARTESIAN_POINT('Ctrl Pts',(-2.46970492160015,5.37920567436201,19.4957591445106));
#17232=CARTESIAN_POINT('Ctrl Pts',(-2.3174971614677,5.44400013492736,19.4879729159318));
#17233=CARTESIAN_POINT('Ctrl Pts',(-2.16524933318927,5.50881165240165,19.4801846376562));
#17234=CARTESIAN_POINT('Ctrl Pts',(-2.01029057557699,5.56722841730974,19.4723963593806));
#17235=CARTESIAN_POINT('Ctrl Pts',(-1.85317624536007,5.61904514718766,19.4646080811051));
#17236=CARTESIAN_POINT('Ctrl Pts',(-1.70380749952587,5.66830736244459,19.4572037574089));
#17237=CARTESIAN_POINT('Ctrl Pts',(-1.55249084692207,5.71160453513816,19.4497994337128));
#17238=CARTESIAN_POINT('Ctrl Pts',(-1.39971655682327,5.74880197285094,19.4423951100166));
#17239=CARTESIAN_POINT('Ctrl Pts',(-1.2390262868339,5.78792679094116,19.4346071322551));
#17240=CARTESIAN_POINT('Ctrl Pts',(-1.07666583229832,5.82031697344828,19.4268191544936));
#17241=CARTESIAN_POINT('Ctrl Pts',(-0.913214151802569,5.84585070588084,
19.419031176732));
#17242=CARTESIAN_POINT('Ctrl Pts',(-0.7497946073091,5.8713794181626,19.4112447301537));
#17243=CARTESIAN_POINT('Ctrl Pts',(-0.585284580461871,5.89005432080999,
19.4034582835754));
#17244=CARTESIAN_POINT('Ctrl Pts',(-0.420271547651839,5.90180501107367,
19.3956718369971));
#17245=CARTESIAN_POINT('Ctrl Pts',(-0.255252219966307,5.91355614959972,
19.3878850933834));
#17246=CARTESIAN_POINT('Ctrl Pts',(-0.0897301663723069,5.91838252054568,
19.3800983497697));
#17247=CARTESIAN_POINT('Ctrl Pts',(0.0757029583459906,5.91626568238764,
19.372311606156));
#17248=CARTESIAN_POINT('Ctrl Pts',(0.241125140900588,5.9141489842426,19.3645253775772));
#17249=CARTESIAN_POINT('Ctrl Pts',(0.406458086801056,5.90509000020647,19.3567391489983));
#17250=CARTESIAN_POINT('Ctrl Pts',(0.571110935857952,5.88912241861582,19.3489529204195));
#17251=CARTESIAN_POINT('Ctrl Pts',(0.735807129185999,5.87315063361667,19.3411646421439));
#17252=CARTESIAN_POINT('Ctrl Pts',(0.899822549465971,5.85026664590831,19.3333763638684));
#17253=CARTESIAN_POINT('Ctrl Pts',(1.06257133350844,5.82055604935698,19.3255880855928));
#17254=CARTESIAN_POINT('Ctrl Pts',(1.21729676005063,5.79231015645354,19.3181837618966));
#17255=CARTESIAN_POINT('Ctrl Pts',(1.37087717065595,5.75789457862528,19.3107794382004));
#17256=CARTESIAN_POINT('Ctrl Pts',(1.52281763783132,5.71742573230382,19.3033751145041));
#17257=CARTESIAN_POINT('Ctrl Pts',(1.68263088047024,5.67485999799536,19.2955871367426));
#17258=CARTESIAN_POINT('Ctrl Pts',(1.8406868890411,5.62558181545351,19.2877991589811));
#17259=CARTESIAN_POINT('Ctrl Pts',(1.99641903140144,5.56976136055739,19.2800111812195));
#17260=CARTESIAN_POINT('Ctrl Pts',(2.15212055548781,5.51395188044115,19.2722247346411));
#17261=CARTESIAN_POINT('Ctrl Pts',(2.30549882437239,5.45160280220751,19.2644382880628));
#17262=CARTESIAN_POINT('Ctrl Pts',(2.45600433643221,5.3829335182525,19.2566518414844));
#17263=CARTESIAN_POINT('Ctrl Pts',(2.60651558993775,5.31426161471922,19.2488650978707));
#17264=CARTESIAN_POINT('Ctrl Pts',(2.75415357497749,5.23926915205707,19.2410783542569));
#17265=CARTESIAN_POINT('Ctrl Pts',(2.89838999345532,5.15822314448862,19.2332916106432));
#17266=CARTESIAN_POINT('Ctrl Pts',(3.04261687177272,5.07718249750748,19.2255053820643));
#17267=CARTESIAN_POINT('Ctrl Pts',(3.18344235521173,4.9900892635211,19.2177191534855));
#17268=CARTESIAN_POINT('Ctrl Pts',(3.32036379618839,4.89725584623281,19.2099329249066));
#17269=CARTESIAN_POINT('Ctrl Pts',(3.45732128124291,4.80439799088065,19.202144646631));
#17270=CARTESIAN_POINT('Ctrl Pts',(3.59037240446021,4.70579711059089,19.1943563683554));
#17271=CARTESIAN_POINT('Ctrl Pts',(3.71904375108522,4.6018087900318,19.1865680900798));
#17272=CARTESIAN_POINT('Ctrl Pts',(3.84137172488175,4.50294699301051,19.1791637663837));
#17273=CARTESIAN_POINT('Ctrl Pts',(3.95974115228138,4.39921631685875,19.1717594426877));
#17274=CARTESIAN_POINT('Ctrl Pts',(4.07377321349348,4.2909558803981,19.1643551189916));
#17275=CARTESIAN_POINT('Ctrl Pts',(4.19371383106715,4.17708594355872,19.1565671412301));
#17276=CARTESIAN_POINT('Ctrl Pts',(4.30889857389756,4.0581636322002,19.1487791634686));
#17277=CARTESIAN_POINT('Ctrl Pts',(4.41891139866457,3.93460958841565,19.1409911857071));
#17278=CARTESIAN_POINT('Ctrl Pts',(4.52890259396773,3.81107983641461,19.1332047391287));
#17279=CARTESIAN_POINT('Ctrl Pts',(4.6337236877407,3.68292040748779,19.1254182925504));
#17280=CARTESIAN_POINT('Ctrl Pts',(4.73299723553544,3.55058695583053,19.117631845972));
#17281=CARTESIAN_POINT('Ctrl Pts',(4.83227457039175,3.41824845595105,19.1098451023583));
#17282=CARTESIAN_POINT('Ctrl Pts',(4.92600374088628,3.28173586795651,19.1020583587446));
#17283=CARTESIAN_POINT('Ctrl Pts',(5.01384871420258,3.14153650839667,19.0942716151309));
#17284=CARTESIAN_POINT('Ctrl Pts',(5.10168787723106,3.00134642197563,19.086485386552));
#17285=CARTESIAN_POINT('Ctrl Pts',(5.18364345233471,2.85747032284362,19.0786991579731));
#17286=CARTESIAN_POINT('Ctrl Pts',(5.2594236542145,2.71042310128678,19.0709129293942));
#17287=CARTESIAN_POINT('Ctrl Pts',(5.3352238049602,2.5633371700771,19.0631246511187));
#17288=CARTESIAN_POINT('Ctrl Pts',(5.40484518588127,2.41307873170581,19.0553363728431));
#17289=CARTESIAN_POINT('Ctrl Pts',(5.4680423473127,2.26018659638867,19.0475480945675));
#17290=CARTESIAN_POINT('Ctrl Pts',(5.52812394986432,2.11483189533364,19.0401437708714));
#17291=CARTESIAN_POINT('Ctrl Pts',(5.58239938977393,1.96709716298893,19.0327394471753));
#17292=CARTESIAN_POINT('Ctrl Pts',(5.63069838974732,1.81746147309837,19.0253351234791));
#17293=CARTESIAN_POINT('Ctrl Pts',(5.68149999609703,1.66007242947687,19.0175471457176));
#17294=CARTESIAN_POINT('Ctrl Pts',(5.7257075551797,1.50052390131145,19.0097591679561));
#17295=CARTESIAN_POINT('Ctrl Pts',(5.76315713010442,1.33938435716808,19.0019711901946));
#17296=CARTESIAN_POINT('Ctrl Pts',(5.80059934212158,1.17827649444091,18.9941847436163));
#17297=CARTESIAN_POINT('Ctrl Pts',(5.83128614879123,1.01557855094246,18.986398297038));
#17298=CARTESIAN_POINT('Ctrl Pts',(5.85510426204067,0.851871259717815,18.9786118504597));
#17299=CARTESIAN_POINT('Ctrl Pts',(5.87892328389751,0.688157723428518,18.9708251068459));
#17300=CARTESIAN_POINT('Ctrl Pts',(5.89587303809803,0.523435078005543,18.9630383632322));
#17301=CARTESIAN_POINT('Ctrl Pts',(5.90589175156542,0.358292033530678,18.9552516196185));
#17302=CARTESIAN_POINT('Ctrl Pts',(5.91590980236986,0.193159912032734,18.9474653910396));
#17303=CARTESIAN_POINT('Ctrl Pts',(5.91899771060221,0.0276077661245249,
18.9396791624607));
#17304=CARTESIAN_POINT('Ctrl Pts',(5.9151457509911,-0.13777266431309,18.9318929338819));
#17305=CARTESIAN_POINT('Ctrl Pts',(5.91129277736546,-0.303196630554846,
18.9241046556063));
#17306=CARTESIAN_POINT('Ctrl Pts',(5.90049629086504,-0.468448471278026,
18.9163163773307));
#17307=CARTESIAN_POINT('Ctrl Pts',(5.88279869842481,-0.632937624344924,
18.9085280990551));
#17308=CARTESIAN_POINT('Ctrl Pts',(5.86597358015943,-0.789317621402037,
18.9011237753589));
#17309=CARTESIAN_POINT('Ctrl Pts',(5.84291142907199,-0.945008056900892,
18.8937194516628));
#17310=CARTESIAN_POINT('Ctrl Pts',(5.81369205926739,-1.09950679966579,18.8863151279666));
#17311=CARTESIAN_POINT('Ctrl Pts',(5.78295869163224,-1.26201087461043,18.8785271502051));
#17312=CARTESIAN_POINT('Ctrl Pts',(5.74540209987075,-1.42325461413253,18.8707391724436));
#17313=CARTESIAN_POINT('Ctrl Pts',(5.70115045531926,-1.5826604336727,18.862951194682));
#17314=CARTESIAN_POINT('Ctrl Pts',(5.65690751102047,-1.74203491266206,18.8551647481037));
#17315=CARTESIAN_POINT('Ctrl Pts',(5.60597222577068,-1.89957188495373,18.8473783015254));
#17316=CARTESIAN_POINT('Ctrl Pts',(5.54852311098912,-2.05470724175479,18.839591854947));
#17317=CARTESIAN_POINT('Ctrl Pts',(5.49107180465324,-2.20984851662026,18.8318051113333));
#17318=CARTESIAN_POINT('Ctrl Pts',(5.42710627881486,-2.3625876916437,18.8240183677196));
#17319=CARTESIAN_POINT('Ctrl Pts',(5.35685409321845,-2.51237831276836,18.8162316241059));
#17320=CARTESIAN_POINT('Ctrl Pts',(5.28660655427863,-2.66215902636385,18.808445395527));
#17321=CARTESIAN_POINT('Ctrl Pts',(5.21007332349161,-2.80899128704693,18.8006591669481));
#17322=CARTESIAN_POINT('Ctrl Pts',(5.12752910865091,-2.95235089419222,18.7928729383692));
#17323=CARTESIAN_POINT('Ctrl Pts',(5.04496316434218,-3.0957482402391,18.7850846600937));
#17324=CARTESIAN_POINT('Ctrl Pts',(4.95638323193211,-3.23567082797014,18.7772963818181));
#17325=CARTESIAN_POINT('Ctrl Pts',(4.86210922735398,-3.37162044479791,18.7695081035425));
#17326=CARTESIAN_POINT('Ctrl Pts',(4.7724828399381,-3.50086787712427,18.7621037798463));
#17327=CARTESIAN_POINT('Ctrl Pts',(4.67771043105415,-3.62652441309787,18.7546994561502));
#17328=CARTESIAN_POINT('Ctrl Pts',(4.57810243098197,-3.74818738778319,18.747295132454));
#17329=CARTESIAN_POINT('Ctrl Pts',(4.47333325539396,-3.87615431361373,18.7395071546925));
#17330=CARTESIAN_POINT('Ctrl Pts',(4.36317659531128,-3.9997486150978,18.731719176931));
#17331=CARTESIAN_POINT('Ctrl Pts',(4.24802145555584,-4.11852452653098,18.7239311991694));
#17332=CARTESIAN_POINT('Ctrl Pts',(4.13288895628821,-4.2372770856016,18.7161447525911));
#17333=CARTESIAN_POINT('Ctrl Pts',(4.01276016050691,-4.35121291555212,18.7083583060127));
#17334=CARTESIAN_POINT('Ctrl Pts',(3.88806182103385,-4.4599221785048,18.7005718594344));
#17335=CARTESIAN_POINT('Ctrl Pts',(3.76335872460007,-4.56863558847094,18.6927851158207));
#17336=CARTESIAN_POINT('Ctrl Pts',(3.63408597392483,-4.67212181951422,18.684998372207));
#17337=CARTESIAN_POINT('Ctrl Pts',(3.50070493533526,-4.77001001238145,18.6772116285933));
#17338=CARTESIAN_POINT('Ctrl Pts',(3.36733271890335,-4.8678917306772,18.6694254000144));
#17339=CARTESIAN_POINT('Ctrl Pts',(3.22985301604037,-4.96017596276984,18.6616391714354));
#17340=CARTESIAN_POINT('Ctrl Pts',(3.08875793689795,-5.04653395606826,18.6538529428565));
#17341=CARTESIAN_POINT('Ctrl Pts',(2.94762571498308,-5.13291468279802,18.646064664581));
#17342=CARTESIAN_POINT('Ctrl Pts',(2.8028764867344,-5.2133658848067,18.6382763863054));
#17343=CARTESIAN_POINT('Ctrl Pts',(2.65502961526059,-5.28760326656503,18.6304881080298));
#17344=CARTESIAN_POINT('Ctrl Pts',(2.51447145142661,-5.35818081726851,18.6230837843337));
#17345=CARTESIAN_POINT('Ctrl Pts',(2.37111394427869,-5.42314234174564,18.6156794606376));
#17346=CARTESIAN_POINT('Ctrl Pts',(2.22542239301741,-5.48228289448444,18.6082751369415));
#17347=CARTESIAN_POINT('Ctrl Pts',(2.07218185305225,-5.5444878072407,18.60048715918));
#17348=CARTESIAN_POINT('Ctrl Pts',(1.91630415376516,-5.60027475898381,18.5926991814185));
#17349=CARTESIAN_POINT('Ctrl Pts',(1.75834421344769,-5.64943857294997,18.584911203657));
#17350=CARTESIAN_POINT('Ctrl Pts',(1.60041532940884,-5.69859272088878,18.5771247570786));
#17351=CARTESIAN_POINT('Ctrl Pts',(1.44040532611202,-5.74112623434872,18.5693383105003));
#17352=CARTESIAN_POINT('Ctrl Pts',(1.27888506697831,-5.77688354980087,18.561551863922));
#17353=CARTESIAN_POINT('Ctrl Pts',(1.11735864621065,-5.81264222931404,18.5537651203083));
#17354=CARTESIAN_POINT('Ctrl Pts',(0.954322165452405,-5.84162412063496,
18.5459783766946));
#17355=CARTESIAN_POINT('Ctrl Pts',(0.790358220861857,-5.86372445167882,
18.5381916330809));
#17356=CARTESIAN_POINT('Ctrl Pts',(0.626405121259873,-5.88582332095108,
18.530405404502));
#17357=CARTESIAN_POINT('Ctrl Pts',(0.4615249973136,-5.90104149822039,18.5226191759231));
#17358=CARTESIAN_POINT('Ctrl Pts',(0.296307283063741,-5.9093258969618,18.5148329473443));
#17359=CARTESIAN_POINT('Ctrl Pts',(0.13104607584411,-5.91761247654142,18.5070446690687));
#17360=CARTESIAN_POINT('Ctrl Pts',(-0.0345525799950898,-5.91896161230755,
18.4992563907931));
#17361=CARTESIAN_POINT('Ctrl Pts',(-0.199896602559165,-5.91337229597336,
18.4914681125176));
#17362=CARTESIAN_POINT('Ctrl Pts',(-0.357089324875416,-5.9080585275236,
18.4840637888214));
#17363=CARTESIAN_POINT('Ctrl Pts',(-0.514051652149983,-5.89647395436541,
18.4766594651252));
#17364=CARTESIAN_POINT('Ctrl Pts',(-0.670276952662783,-5.87866135861125,
18.469255141429));
#17365=CARTESIAN_POINT('Ctrl Pts',(-0.834597046719215,-5.85992580553435,
18.4614671636675));
#17366=CARTESIAN_POINT('Ctrl Pts',(-0.998160488801119,-5.83429298411085,
18.453679185906));
#17367=CARTESIAN_POINT('Ctrl Pts',(-1.16038185126092,-5.80184837114555,
18.4458912081445));
#17368=CARTESIAN_POINT('Ctrl Pts',(-1.32257131960991,-5.76941013706935,
18.4381047615662));
#17369=CARTESIAN_POINT('Ctrl Pts',(-1.48341892167171,-5.73016284629375,
18.4303183149878));
#17370=CARTESIAN_POINT('Ctrl Pts',(-1.6423489782677,-5.68424316827518,18.4225318684095));
#17371=CARTESIAN_POINT('Ctrl Pts',(-1.80128509768769,-5.63832173852423,
18.4147451247958));
#17372=CARTESIAN_POINT('Ctrl Pts',(-1.9583032171875,-5.58572749709572,18.4069583811821));
#17373=CARTESIAN_POINT('Ctrl Pts',(-2.11284166849272,-5.52664732422659,
18.3991716375683));
#17374=CARTESIAN_POINT('Ctrl Pts',(-2.26736989823559,-5.46757105906888,
18.3913854089894));
#17375=CARTESIAN_POINT('Ctrl Pts',(-2.41941848952946,-5.40200983518058,
18.3835991804105));
#17376=CARTESIAN_POINT('Ctrl Pts',(-2.56844451065284,-5.33019918560248,
18.3758129518316));
#17377=CARTESIAN_POINT('Ctrl Pts',(-2.71750976234046,-5.25836963212907,
18.3680246735561));
#17378=CARTESIAN_POINT('Ctrl Pts',(-2.86355056500712,-5.18028750267804,
18.3602363952805));
#17379=CARTESIAN_POINT('Ctrl Pts',(-3.00604659027617,-5.09623532223435,
18.3524481170049));
#17380=CARTESIAN_POINT('Ctrl Pts',(-3.14151769944448,-5.01632683291879,
18.3450437933088));
#17381=CARTESIAN_POINT('Ctrl Pts',(-3.27378489328733,-4.93102288253372,
18.3376394696127));
#17382=CARTESIAN_POINT('Ctrl Pts',(-3.40242382940286,-4.84060354166829,
18.3302351459165));
#17383=CARTESIAN_POINT('Ctrl Pts',(-3.5377281751942,-4.74549913446382,18.322447168155));
#17384=CARTESIAN_POINT('Ctrl Pts',(-3.66906668631932,-4.64470113540048,
18.3146591903935));
#17385=CARTESIAN_POINT('Ctrl Pts',(-3.79596627439377,-4.53856481788737,
18.306871212632));
#17386=CARTESIAN_POINT('Ctrl Pts',(-3.92284091292092,-4.43244936768452,
18.2990847660537));
#17387=CARTESIAN_POINT('Ctrl Pts',(-4.0452781247844,-4.3209978980971,18.2912983194754));
#17388=CARTESIAN_POINT('Ctrl Pts',(-4.16283788496959,-4.20460596322199,
18.2835118728971));
#17389=CARTESIAN_POINT('Ctrl Pts',(-4.28040212979489,-4.08820958825667,
18.2757251292834));
#17390=CARTESIAN_POINT('Ctrl Pts',(-4.39308832076967,-3.96687259288409,
18.2679383856697));
#17391=CARTESIAN_POINT('Ctrl Pts',(-4.50049276866213,-3.84102790952108,
18.260151642056));
#17392=CARTESIAN_POINT('Ctrl Pts',(-4.60789011255429,-3.71519154984192,
18.2523654134771));
#17393=CARTESIAN_POINT('Ctrl Pts',(-4.71000620508511,-3.58484834196991,
18.2445791848983));
#17394=CARTESIAN_POINT('Ctrl Pts',(-4.80647709615534,-3.45046496673044,
18.2367929563194));
#17395=CARTESIAN_POINT('Ctrl Pts',(-4.90297338284109,-3.3160462155502,18.2290046780438));
#17396=CARTESIAN_POINT('Ctrl Pts',(-4.99382131050251,-3.17758543040561,
18.2212163997682));
#17397=CARTESIAN_POINT('Ctrl Pts',(-5.07869926820291,-3.03557973139485,
18.2134281214926));
#17398=CARTESIAN_POINT('Ctrl Pts',(-5.15939282475632,-2.90057477587416,
18.2060237977964));
#17399=CARTESIAN_POINT('Ctrl Pts',(-5.23469072442586,-2.76236623480627,
18.1986194741002));
#17400=CARTESIAN_POINT('Ctrl Pts',(-5.30435445677128,-2.62140312798902,
18.191215150404));
#17401=CARTESIAN_POINT('Ctrl Pts',(-5.3774115817258,-2.47357356213026,18.183450154426));
#17402=CARTESIAN_POINT('Ctrl Pts',(-5.44429948401845,-2.32265849524358,
18.175685158448));
#17403=CARTESIAN_POINT('Ctrl Pts',(-5.50477361220699,-2.16919294689283,
18.16792016247));
#17404=CARTESIAN_POINT('Ctrl Pts',(-5.56523522785852,-2.01575915168033,
18.1601567731261));
#17405=CARTESIAN_POINT('Ctrl Pts',(-5.61928559859745,-1.85977622850732,
18.1523933837822));
#17406=CARTESIAN_POINT('Ctrl Pts',(-5.6667284601636,-1.70179878989023,18.1446299944383));
#17407=CARTESIAN_POINT('Ctrl Pts',(-5.71417181700182,-1.54381970209328,
18.1368665240498));
#17408=CARTESIAN_POINT('Ctrl Pts',(-5.75500742999307,-1.38384636573191,
18.1291030536613));
#17409=CARTESIAN_POINT('Ctrl Pts',(-5.7890888339399,-1.22244878635157,18.1213395832728));
#17410=CARTESIAN_POINT('Ctrl Pts',(-5.82316860033722,-1.06105896183154,
18.1135764859049));
#17411=CARTESIAN_POINT('Ctrl Pts',(-5.85049474115828,-0.898245347765023,
18.105813388537));
#17412=CARTESIAN_POINT('Ctrl Pts',(-5.87097182966171,-0.734588550018744,
18.0980502911692));
#17413=CARTESIAN_POINT('Ctrl Pts',(-5.89145331993988,-0.570896572449048,
18.0902855250384));
#17414=CARTESIAN_POINT('Ctrl Pts',(-5.90508277646522,-0.40636137001757,
18.0825207589076));
#17415=CARTESIAN_POINT('Ctrl Pts',(-5.91181652145501,-0.241569822518524,
18.0747559927768));
#17416=CARTESIAN_POINT('Ctrl Pts',(-5.91510639983007,-0.161058287060608,
18.0709623926004));
#17417=CARTESIAN_POINT('Ctrl Pts',(-5.91675108298957,-0.0804856220266957,
18.067168792424));
#17418=CARTESIAN_POINT('Ctrl Pts',(-5.9167499994649,7.95746161645733E-5,
18.0633751922476));
#17419=CARTESIAN_POINT('Ctrl Pts',(-5.91674999819064,0.000146325028583011,
17.8116248078341));
#17420=CARTESIAN_POINT('Ctrl Pts',(-5.9167540725871,-0.164604609812423,
17.8193809745373));
#17421=CARTESIAN_POINT('Ctrl Pts',(-5.90987261000619,-0.329380941156183,
17.8271371412406));
#17422=CARTESIAN_POINT('Ctrl Pts',(-5.89612531645656,-0.493595801380071,
17.8348933079438));
#17423=CARTESIAN_POINT('Ctrl Pts',(-5.88237802530819,-0.657810632920316,
17.8426494732922));
#17424=CARTESIAN_POINT('Ctrl Pts',(-5.86176492750662,-0.821463669676354,
17.8504056386407));
#17425=CARTESIAN_POINT('Ctrl Pts',(-5.83435771645861,-0.983971848631785,
17.8581618039891));
#17426=CARTESIAN_POINT('Ctrl Pts',(-5.80695247133969,-1.14646837081722,
17.865917412985));
#17427=CARTESIAN_POINT('Ctrl Pts',(-5.77275414191316,-1.30781987939427,
17.8736730219809));
#17428=CARTESIAN_POINT('Ctrl Pts',(-5.73188581331638,-1.46745207267648,
17.8814286309768));
#17429=CARTESIAN_POINT('Ctrl Pts',(-5.69100690643398,-1.62712558487214,
17.8891862474208));
#17430=CARTESIAN_POINT('Ctrl Pts',(-5.64345462981406,-1.78507857753726,
17.8969438638648));
#17431=CARTESIAN_POINT('Ctrl Pts',(-5.58940257527164,-1.94074970412125,
17.9047014803088));
#17432=CARTESIAN_POINT('Ctrl Pts',(-5.54438664803198,-2.0703965818754,17.9111622207996));
#17433=CARTESIAN_POINT('Ctrl Pts',(-5.4948634147778,-2.1984609143109,17.9176229612904));
#17434=CARTESIAN_POINT('Ctrl Pts',(-5.44095909162526,-2.3246278682319,17.9240837017813));
#17435=CARTESIAN_POINT('Ctrl Pts',(-5.37598002709395,-2.47671605264993,
17.9318718131742));
#17436=CARTESIAN_POINT('Ctrl Pts',(-5.30460850959539,-2.62610519568956,
17.9396599245672));
#17437=CARTESIAN_POINT('Ctrl Pts',(-5.22709400012667,-2.77225880399717,
17.9474480359602));
#17438=CARTESIAN_POINT('Ctrl Pts',(-5.14959470928051,-2.91838371759179,
17.9552346182932));
#17439=CARTESIAN_POINT('Ctrl Pts',(-5.06595498255194,-3.06127408183878,
17.9630212006263));
#17440=CARTESIAN_POINT('Ctrl Pts',(-4.97647054204924,-3.20041739568703,
17.9708077829594));
#17441=CARTESIAN_POINT('Ctrl Pts',(-4.88698268952489,-3.33956601503862,
17.9785946621931));
#17442=CARTESIAN_POINT('Ctrl Pts',(-4.79164984679594,-3.4749670272255,17.9863815414268));
#17443=CARTESIAN_POINT('Ctrl Pts',(-4.69081183623025,-3.60613572672773,
17.9941684206605));
#17444=CARTESIAN_POINT('Ctrl Pts',(-4.58998048091514,-3.73729576917142,
18.0019547859646));
#17445=CARTESIAN_POINT('Ctrl Pts',(-4.48364487971286,-3.86422380464239,
18.0097411512688));
#17446=CARTESIAN_POINT('Ctrl Pts',(-4.37218611028819,-3.98646700469263,
18.0175275165729));
#17447=CARTESIAN_POINT('Ctrl Pts',(-4.26069807405392,-4.10874230332498,
18.0253159264185));
#17448=CARTESIAN_POINT('Ctrl Pts',(-4.14408439551994,-4.2263300708761,18.0331043362641));
#17449=CARTESIAN_POINT('Ctrl Pts',(-4.02276470881542,-4.33881258641223,
18.0408927461097));
#17450=CARTESIAN_POINT('Ctrl Pts',(-3.90782060928847,-4.44538392542597,
18.0482718597619));
#17451=CARTESIAN_POINT('Ctrl Pts',(-3.78865259034154,-4.54737261642784,
18.0556509734142));
#17452=CARTESIAN_POINT('Ctrl Pts',(-3.66564642919633,-4.64445549215623,
18.0630300870664));
#17453=CARTESIAN_POINT('Ctrl Pts',(-3.53582247876412,-4.74691932265901,
18.0708181984594));
#17454=CARTESIAN_POINT('Ctrl Pts',(-3.4016764860377,-4.84395468839645,18.0786063098524));
#17455=CARTESIAN_POINT('Ctrl Pts',(-3.26368418575208,-4.93520983324638,
18.0863944212453));
#17456=CARTESIAN_POINT('Ctrl Pts',(-3.12571897784921,-5.02644706173934,
18.0941810035784));
#17457=CARTESIAN_POINT('Ctrl Pts',(-2.9839092355035,-5.11190615755588,18.1019675859115));
#17458=CARTESIAN_POINT('Ctrl Pts',(-2.8387598376241,-5.19127856570926,18.1097541682446));
#17459=CARTESIAN_POINT('Ctrl Pts',(-2.69360490523057,-5.27065400031484,
18.1175410474783));
#17460=CARTESIAN_POINT('Ctrl Pts',(-2.54511034093988,-5.34394212609427,
18.125327926712));
#17461=CARTESIAN_POINT('Ctrl Pts',(-2.39380645074351,-5.41087989507056,
18.1331148059457));
#17462=CARTESIAN_POINT('Ctrl Pts',(-2.24251254651653,-5.47781324619274,
18.1409011712499));
#17463=CARTESIAN_POINT('Ctrl Pts',(-2.08840997970543,-5.53839695005758,
18.1486875365541));
#17464=CARTESIAN_POINT('Ctrl Pts',(-1.93205003240429,-5.59241568866144,
18.1564739018583));
#17465=CARTESIAN_POINT('Ctrl Pts',(-1.77564902815592,-5.64644861148919,
18.1642623117039));
#17466=CARTESIAN_POINT('Ctrl Pts',(-1.61698976057277,-5.69391301824909,
18.1720507215495));
#17467=CARTESIAN_POINT('Ctrl Pts',(-1.45664057238756,-5.73464286641936,
18.1798391313951));
#17468=CARTESIAN_POINT('Ctrl Pts',(-1.30471804813656,-5.77323228128587,
18.1872182450472));
#17469=CARTESIAN_POINT('Ctrl Pts',(-1.15127890423576,-5.80577669632586,
18.1945973586994));
#17470=CARTESIAN_POINT('Ctrl Pts',(-0.996816515083505,-5.83217690041693,
18.2019764723515));
#17471=CARTESIAN_POINT('Ctrl Pts',(-0.833792831013664,-5.86004037290847,
18.2097645837445));
#17472=CARTESIAN_POINT('Ctrl Pts',(-0.669571031919846,-5.88106916913186,
18.2175526951374));
#17473=CARTESIAN_POINT('Ctrl Pts',(-0.504737163865283,-5.8951820122803,
18.2253408065304));
#17474=CARTESIAN_POINT('Ctrl Pts',(-0.339935658066676,-5.90929208461806,
18.2331273888635));
#17475=CARTESIAN_POINT('Ctrl Pts',(-0.174522641247447,-5.916488885908,18.2409139711966));
#17476=CARTESIAN_POINT('Ctrl Pts',(-0.00908908268880194,-5.9167430188471,
18.2487005535297));
#17477=CARTESIAN_POINT('Ctrl Pts',(0.156350783813921,-5.91699716147622,
18.2564874327634));
#17478=CARTESIAN_POINT('Ctrl Pts',(0.321810874114001,-5.9103081016057,18.2642743119971));
#17479=CARTESIAN_POINT('Ctrl Pts',(0.486699662987048,-5.89669856788935,
18.2720611912308));
#17480=CARTESIAN_POINT('Ctrl Pts',(0.651577569295335,-5.88308993239436,
18.279847556535));
#17481=CARTESIAN_POINT('Ctrl Pts',(0.815883931170508,-5.86256176347832,
18.2876339218391));
#17482=CARTESIAN_POINT('Ctrl Pts',(0.979031639496074,-5.83518873828136,
18.2954202871433));
#17483=CARTESIAN_POINT('Ctrl Pts',(1.1422221870969,-5.80780852548383,18.3032086969889));
#17484=CARTESIAN_POINT('Ctrl Pts',(1.30425315756301,-5.77357991597678,18.3109971068345));
#17485=CARTESIAN_POINT('Ctrl Pts',(1.46454603556983,-5.73262901923687,18.3187855166801));
#17486=CARTESIAN_POINT('Ctrl Pts',(1.61641520885367,-5.69383017233578,18.3261646303323));
#17487=CARTESIAN_POINT('Ctrl Pts',(1.76672401938484,-5.64899746877865,18.3335437439844));
#17488=CARTESIAN_POINT('Ctrl Pts',(1.91499175774266,-5.59827983672464,18.3409228576366));
#17489=CARTESIAN_POINT('Ctrl Pts',(2.07147744379432,-5.54475110866289,18.3487109690296));
#17490=CARTESIAN_POINT('Ctrl Pts',(2.22574527185444,-5.48464747488087,18.3564990804225));
#17491=CARTESIAN_POINT('Ctrl Pts',(2.37724173580704,-5.41817794946208,18.3642871918155));
#17492=CARTESIAN_POINT('Ctrl Pts',(2.52870845606942,-5.35172147417609,18.3720737741485));
#17493=CARTESIAN_POINT('Ctrl Pts',(2.67740460546071,-5.2789017293409,18.3798603564816));
#17494=CARTESIAN_POINT('Ctrl Pts',(2.8227971756589,-5.19997564105758,18.3876469388146));
#17495=CARTESIAN_POINT('Ctrl Pts',(2.96819528964393,-5.1210465433398,18.3954338180483));
#17496=CARTESIAN_POINT('Ctrl Pts',(3.11028928968802,-5.03601078524024,18.403220697282));
#17497=CARTESIAN_POINT('Ctrl Pts',(3.24857061817865,-4.94517133183537,18.4110075765157));
#17498=CARTESIAN_POINT('Ctrl Pts',(3.38684282018164,-4.85433787378184,18.4187939418199));
#17499=CARTESIAN_POINT('Ctrl Pts',(3.52130258717436,-4.75770166249414,18.4265803071241));
#17500=CARTESIAN_POINT('Ctrl Pts',(3.65147009341721,-4.65560916737861,18.4343666724283));
#17501=CARTESIAN_POINT('Ctrl Pts',(3.78167177900373,-4.55348986484716,18.4421550822739));
#17502=CARTESIAN_POINT('Ctrl Pts',(3.90757869895332,-4.44591161143244,18.4499434921195));
#17503=CARTESIAN_POINT('Ctrl Pts',(4.02874318097474,-4.33326192887639,18.4577319019651));
#17504=CARTESIAN_POINT('Ctrl Pts',(4.14354023212818,-4.22653220779757,18.4651110156173));
#17505=CARTESIAN_POINT('Ctrl Pts',(4.2540802833303,-4.11525055202227,18.4724901292695));
#17506=CARTESIAN_POINT('Ctrl Pts',(4.36001246514896,-3.99977772710506,18.4798692429217));
#17507=CARTESIAN_POINT('Ctrl Pts',(4.47181608696418,-3.87790465864433,18.4876573543147));
#17508=CARTESIAN_POINT('Ctrl Pts',(4.57852649029881,-3.75131911686164,18.4954454657077));
#17509=CARTESIAN_POINT('Ctrl Pts',(4.67975762850595,-3.62046945863936,18.5032335771007));
#17510=CARTESIAN_POINT('Ctrl Pts',(4.78096889174362,-3.48964549046668,18.5110201594337));
#17511=CARTESIAN_POINT('Ctrl Pts',(4.87670284091196,-3.35455932885706,18.5188067417668));
#17512=CARTESIAN_POINT('Ctrl Pts',(4.96661435174363,-3.21569159646167,18.5265933240998));
#17513=CARTESIAN_POINT('Ctrl Pts',(5.05652929088143,-3.07681856907019,18.5343802033335));
#17514=CARTESIAN_POINT('Ctrl Pts',(5.14062117047605,-2.93416394842851,18.5421670825673));
#17515=CARTESIAN_POINT('Ctrl Pts',(5.2185883636556,-2.78823708698138,18.549953961801));
#17516=CARTESIAN_POINT('Ctrl Pts',(5.29655041104549,-2.6423198566227,18.5577403271052));
#17517=CARTESIAN_POINT('Ctrl Pts',(5.36838843045436,-2.49313109954214,18.5655266924094));
#17518=CARTESIAN_POINT('Ctrl Pts',(5.4338468391293,-2.34120462398836,18.5733130577136));
#17519=CARTESIAN_POINT('Ctrl Pts',(5.49932243585305,-2.18923825562739,18.5811014675592));
#17520=CARTESIAN_POINT('Ctrl Pts',(5.55841494623099,-2.03453302521722,18.5888898774048));
#17521=CARTESIAN_POINT('Ctrl Pts',(5.61091666307221,-1.87764340665598,18.5966782872504));
#17522=CARTESIAN_POINT('Ctrl Pts',(5.66065931185227,-1.72899864486787,18.6040574009026));
#17523=CARTESIAN_POINT('Ctrl Pts',(5.70448598572576,-1.5783934242125,18.6114365145548));
#17524=CARTESIAN_POINT('Ctrl Pts',(5.74226118119846,-1.42631240946761,18.6188156282069));
#17525=CARTESIAN_POINT('Ctrl Pts',(5.78213011994918,-1.26580209082761,18.6266037395999));
#17526=CARTESIAN_POINT('Ctrl Pts',(5.81527197387513,-1.10359041712131,18.6343918509929));
#17527=CARTESIAN_POINT('Ctrl Pts',(5.84156225634684,-0.940255799090872,
18.6421799623858));
#17528=CARTESIAN_POINT('Ctrl Pts',(5.86784737717978,-0.776953248966031,
18.6499665447189));
#17529=CARTESIAN_POINT('Ctrl Pts',(5.8872835598595,-0.612528509694548,18.6577531270519));
#17530=CARTESIAN_POINT('Ctrl Pts',(5.89979768971373,-0.447568746617209,
18.6655397093849));
#17531=CARTESIAN_POINT('Ctrl Pts',(5.91231229672898,-0.282602693660528,
18.6733265886186));
#17532=CARTESIAN_POINT('Ctrl Pts',(5.91790429467534,-0.117101894378561,
18.6811134678523));
#17533=CARTESIAN_POINT('Ctrl Pts',(5.91655251028279,0.0483420682882251,
18.688900347086));
#17534=CARTESIAN_POINT('Ctrl Pts',(5.91520081510723,0.213775111749494,18.6966867123902));
#17535=CARTESIAN_POINT('Ctrl Pts',(5.90690625742143,0.37915100656057,18.7044730776944));
#17536=CARTESIAN_POINT('Ctrl Pts',(5.89169979686626,0.543878723711526,18.7122594429986));
#17537=CARTESIAN_POINT('Ctrl Pts',(5.87648934340334,0.708649695015895,18.7200478528442));
#17538=CARTESIAN_POINT('Ctrl Pts',(5.85436338792983,0.872771830005027,18.7278362626898));
#17539=CARTESIAN_POINT('Ctrl Pts',(5.82540481788583,1.03565885804763,18.7356246725353));
#17540=CARTESIAN_POINT('Ctrl Pts',(5.79796807742191,1.18998585370229,18.7430037861876));
#17541=CARTESIAN_POINT('Ctrl Pts',(5.76439843169625,1.34320396202403,18.7503828998398));
#17542=CARTESIAN_POINT('Ctrl Pts',(5.72480877271826,1.49482275815833,18.757762013492));
#17543=CARTESIAN_POINT('Ctrl Pts',(5.68302480127369,1.65484523907078,18.765550124885));
#17544=CARTESIAN_POINT('Ctrl Pts',(5.63451963482885,1.81314324410065,18.7733382362779));
#17545=CARTESIAN_POINT('Ctrl Pts',(5.57946069092875,1.96914929877876,18.7811263476709));
#17546=CARTESIAN_POINT('Ctrl Pts',(5.52441255689239,2.12512472438785,18.788912930004));
#17547=CARTESIAN_POINT('Ctrl Pts',(5.46281331906599,2.27880879637063,18.7966995123371));
#17548=CARTESIAN_POINT('Ctrl Pts',(5.39487969439156,2.42965093080089,18.8044860946702));
#17549=CARTESIAN_POINT('Ctrl Pts',(5.32694347942315,2.58049881680816,18.8122729739039));
#17550=CARTESIAN_POINT('Ctrl Pts',(5.2526725219132,2.72850425547445,18.8200598531376));
#17551=CARTESIAN_POINT('Ctrl Pts',(5.17233126327013,2.87313763427693,18.8278467323714));
#17552=CARTESIAN_POINT('Ctrl Pts',(5.09199530710365,3.01776146736008,18.8356330976756));
#17553=CARTESIAN_POINT('Ctrl Pts',(5.00559000681519,3.15901340665284,18.8434194629798));
#17554=CARTESIAN_POINT('Ctrl Pts',(4.91342531789231,3.29638926827443,18.851205828284));
#17555=CARTESIAN_POINT('Ctrl Pts',(4.82123642839389,3.43380120200731,18.8589942381296));
#17556=CARTESIAN_POINT('Ctrl Pts',(4.72328530489684,3.56733475773288,18.8667826479752));
#17557=CARTESIAN_POINT('Ctrl Pts',(4.61992522529848,3.69651477410152,18.8745710578208));
#17558=CARTESIAN_POINT('Ctrl Pts',(4.521996920347,3.81890612756933,18.8819501714729));
#17559=CARTESIAN_POINT('Ctrl Pts',(4.41921370209614,3.93738954361189,18.889329285125));
#17560=CARTESIAN_POINT('Ctrl Pts',(4.31190934014089,4.05158838048805,18.8967083987771));
#17561=CARTESIAN_POINT('Ctrl Pts',(4.19865748317581,4.17211684833235,18.9044965101701));
#17562=CARTESIAN_POINT('Ctrl Pts',(4.08032864153333,4.28791535783792,18.912284621563));
#17563=CARTESIAN_POINT('Ctrl Pts',(3.95734132817861,4.39856569517719,18.920072732956));
#17564=CARTESIAN_POINT('Ctrl Pts',(3.83437816123921,4.50919430825134,18.927859315289));
#17565=CARTESIAN_POINT('Ctrl Pts',(3.70675858489957,4.61467655233321,18.935645897622));
#17566=CARTESIAN_POINT('Ctrl Pts',(3.57493632201928,4.7146326321366,18.9434324799551));
#17567=CARTESIAN_POINT('Ctrl Pts',(3.44310903278497,4.81459252324342,18.9512193591888));
#17568=CARTESIAN_POINT('Ctrl Pts',(3.30707898856819,4.90902563223852,18.9590062384225));
#17569=CARTESIAN_POINT('Ctrl Pts',(3.16733178671294,4.99759341237138,18.9667931176562));
#17570=CARTESIAN_POINT('Ctrl Pts',(3.02759380809268,5.08615534708166,18.9745794829604));
#17571=CARTESIAN_POINT('Ctrl Pts',(2.88413943275194,5.16885255663049,18.9823658482645));
#17572=CARTESIAN_POINT('Ctrl Pts',(2.73748205902751,5.24539059927881,18.9901522135687));
#17573=CARTESIAN_POINT('Ctrl Pts',(2.59078617605451,5.32194873926308,18.9979406234143));
#17574=CARTESIAN_POINT('Ctrl Pts',(2.44088589668048,5.39234433104655,19.0057290332599));
#17575=CARTESIAN_POINT('Ctrl Pts',(2.28831877623673,5.45632914520582,19.0135174431055));
#17576=CARTESIAN_POINT('Ctrl Pts',(2.14376935682108,5.51695143204743,19.0208965567577));
#17577=CARTESIAN_POINT('Ctrl Pts',(1.99682642228916,5.5718193081064,19.02827567041));
#17578=CARTESIAN_POINT('Ctrl Pts',(1.84796326203191,5.62076172281661,19.0356547840622));
#17579=CARTESIAN_POINT('Ctrl Pts',(1.69084915198724,5.67241683961881,19.0434428954552));
#17580=CARTESIAN_POINT('Ctrl Pts',(1.53153980467278,5.71748946353226,19.0512310068482));
#17581=CARTESIAN_POINT('Ctrl Pts',(1.3706028141193,5.75581258280951,19.0590191182411));
#17582=CARTESIAN_POINT('Ctrl Pts',(1.20969742073803,5.79412817801044,19.0668057005742));
#17583=CARTESIAN_POINT('Ctrl Pts',(1.04716533237892,5.82569683866613,19.0745922829073));
#17584=CARTESIAN_POINT('Ctrl Pts',(0.883586680899844,5.85040213488239,19.0823788652404));
#17585=CARTESIAN_POINT('Ctrl Pts',(0.720001792203485,5.87510837310604,19.0901657444741));
#17586=CARTESIAN_POINT('Ctrl Pts',(0.555370575880033,5.89295067161186,19.0979526237078));
#17587=CARTESIAN_POINT('Ctrl Pts',(0.390281418745612,5.90386407166374,19.1057395029415));
#17588=CARTESIAN_POINT('Ctrl Pts',(0.225203157400029,5.91477675143752,19.1135258682457));
#17589=CARTESIAN_POINT('Ctrl Pts',(0.0596673345911858,5.91876142693074,
19.1213122335499));
#17590=CARTESIAN_POINT('Ctrl Pts',(-0.105734351571204,5.91580516999992,
19.1290985988541));
#17591=CARTESIAN_POINT('Ctrl Pts',(-0.271179468857582,5.91284813681607,
19.1368870086997));
#17592=CARTESIAN_POINT('Ctrl Pts',(-0.436490059395146,5.90294653315044,
19.1446754185453));
#17593=CARTESIAN_POINT('Ctrl Pts',(-0.601075321867329,5.88613956850686,
19.1524638283909));
#17594=CARTESIAN_POINT('Ctrl Pts',(-0.757011306404463,5.87021584277703,
19.1598429420431));
#17595=CARTESIAN_POINT('Ctrl Pts',(-0.912295978160383,5.84809389555017,
19.1672220556953));
#17596=CARTESIAN_POINT('Ctrl Pts',(-1.06643189429465,5.81984996175427,19.1746011693474));
#17597=CARTESIAN_POINT('Ctrl Pts',(-1.22911101012078,5.79004056824881,19.1823892807404));
#17598=CARTESIAN_POINT('Ctrl Pts',(-1.39056851718186,5.75340065856032,19.1901773921334));
#17599=CARTESIAN_POINT('Ctrl Pts',(-1.55022609389384,5.71005513286086,19.1979655035264));
#17600=CARTESIAN_POINT('Ctrl Pts',(-1.7098523246219,5.66671811730028,19.2057520858594));
#17601=CARTESIAN_POINT('Ctrl Pts',(-1.86767902193326,5.61667819626607,19.2135386681923));
#17602=CARTESIAN_POINT('Ctrl Pts',(-2.02314105463405,5.56011068554883,19.2213252505253));
#17603=CARTESIAN_POINT('Ctrl Pts',(-2.17860901506916,5.5035410179244,19.229112129759));
#17604=CARTESIAN_POINT('Ctrl Pts',(-2.33171182886849,5.44044336811981,19.2368990089928));
#17605=CARTESIAN_POINT('Ctrl Pts',(-2.48190174158795,5.37104219938763,19.2446858882265));
#17606=CARTESIAN_POINT('Ctrl Pts',(-2.6320817418598,5.30164561109255,19.2524722535306));
#17607=CARTESIAN_POINT('Ctrl Pts',(-2.77934893574198,5.2259464705573,19.2602586188348));
#17608=CARTESIAN_POINT('Ctrl Pts',(-2.92317755433823,5.14421651452514,19.268044984139));
#17609=CARTESIAN_POINT('Ctrl Pts',(-3.06704393940887,5.06246509786629,19.2758333939846));
#17610=CARTESIAN_POINT('Ctrl Pts',(-3.20746966606069,4.97467985768772,19.2836218038302));
#17611=CARTESIAN_POINT('Ctrl Pts',(-3.34395469738098,4.88117788493348,19.2914102136757));
#17612=CARTESIAN_POINT('Ctrl Pts',(-3.47326717295838,4.79258962399922,19.298789327328));
#17613=CARTESIAN_POINT('Ctrl Pts',(-3.59904226817873,4.69887017428683,19.3061684409802));
#17614=CARTESIAN_POINT('Ctrl Pts',(-3.72087964060683,4.60032447362331,19.3135475546325));
#17615=CARTESIAN_POINT('Ctrl Pts',(-3.84947002056502,4.49631673905857,19.3213356660255));
#17616=CARTESIAN_POINT('Ctrl Pts',(-3.97371971817014,4.38689543302841,19.3291237774184));
#17617=CARTESIAN_POINT('Ctrl Pts',(-4.09318065268493,4.27244692266455,19.3369118888114));
#17618=CARTESIAN_POINT('Ctrl Pts',(-4.21261813312735,4.15802088227095,19.3446984711445));
#17619=CARTESIAN_POINT('Ctrl Pts',(-4.32726849585139,4.03856982782181,19.3524850534775));
#17620=CARTESIAN_POINT('Ctrl Pts',(-4.43671936351229,3.91451808680649,19.3602716358106));
#17621=CARTESIAN_POINT('Ctrl Pts',(-4.54617440451051,3.79046161572578,19.3680585150443));
#17622=CARTESIAN_POINT('Ctrl Pts',(-4.65042933938387,3.66180434403611,19.375845394278));
#17623=CARTESIAN_POINT('Ctrl Pts',(-4.7491105635871,3.52900544308526,19.3836322735117));
#17624=CARTESIAN_POINT('Ctrl Pts',(-4.84778527488706,3.39621530678447,19.3914186388159));
#17625=CARTESIAN_POINT('Ctrl Pts',(-4.94088682116381,3.25928434478957,19.3992050041201));
#17626=CARTESIAN_POINT('Ctrl Pts',(-5.02808352118854,3.11870272171817,19.4069913694243));
#17627=CARTESIAN_POINT('Ctrl Pts',(-5.11530311729573,2.97808418476775,19.4147797792699));
#17628=CARTESIAN_POINT('Ctrl Pts',(-5.19661459876018,2.83381334197159,19.4225681891156));
#17629=CARTESIAN_POINT('Ctrl Pts',(-5.27173057924417,2.68640787341795,19.4303565989612));
#17630=CARTESIAN_POINT('Ctrl Pts',(-5.34289906781531,2.54674885097706,19.4377357126133));
#17631=CARTESIAN_POINT('Ctrl Pts',(-5.40850636029273,2.40427642204715,19.4451148262655));
#17632=CARTESIAN_POINT('Ctrl Pts',(-5.46834679985539,2.25944989743329,19.4524939399176));
#17633=CARTESIAN_POINT('Ctrl Pts',(-5.5312699114988,2.10716265416091,19.4602531876029));
#17634=CARTESIAN_POINT('Ctrl Pts',(-5.5878403187911,1.95221414694597,19.4680124352882));
#17635=CARTESIAN_POINT('Ctrl Pts',(-5.63785008126168,1.79515376046669,19.4757716829735));
#17636=CARTESIAN_POINT('Ctrl Pts',(-5.68785351891928,1.63811323766045,19.4835299493346));
#17637=CARTESIAN_POINT('Ctrl Pts',(-5.73129786566256,1.47896167632964,19.4912882156957));
#17638=CARTESIAN_POINT('Ctrl Pts',(-5.76802463240211,1.31826492121368,19.4990464820568));
#17639=CARTESIAN_POINT('Ctrl Pts',(-5.80474645082447,1.15758981729621,19.5068037031214));
#17640=CARTESIAN_POINT('Ctrl Pts',(-5.83475242452542,0.995370251430543,
19.5145609241859));
#17641=CARTESIAN_POINT('Ctrl Pts',(-5.85793484294928,0.832183836817834,
19.5223181452504));
#17642=CARTESIAN_POINT('Ctrl Pts',(-5.88112019170124,0.668976794946629,
19.5300763468513));
#17643=CARTESIAN_POINT('Ctrl Pts',(-5.89748021436318,0.504802981008405,
19.5378345484521));
#17644=CARTESIAN_POINT('Ctrl Pts',(-5.90695879742514,0.340247451161346,
19.5455927500529));
#17645=CARTESIAN_POINT('Ctrl Pts',(-5.91348785311707,0.226897996737223,
19.5509367693003));
#17646=CARTESIAN_POINT('Ctrl Pts',(-5.91675291062979,0.113367578874178,
19.5562807885477));
#17647=CARTESIAN_POINT('Ctrl Pts',(-5.91674999805254,-0.000151806595337599,
19.5616248077951));
#17648=CARTESIAN_POINT('Origin',(0.,0.,0.));
#17649=CARTESIAN_POINT('',(-5.91674999800917,0.00015348778061909,21.563375191845));
#17650=CARTESIAN_POINT('',(-5.91674999913571,0.000101131768199252,21.3116248077951));
#17651=CARTESIAN_POINT('',(-5.91675,-7.2459289488551E-16,0.));
#17652=CARTESIAN_POINT('Ctrl Pts',(-5.91674999800917,0.00015348778061909,
21.563375191845));
#17653=CARTESIAN_POINT('Ctrl Pts',(-5.91674549259033,0.173831397393708,
21.5551998572909));
#17654=CARTESIAN_POINT('Ctrl Pts',(-5.90908954177321,0.347471023012969,
21.5470245227368));
#17655=CARTESIAN_POINT('Ctrl Pts',(-5.89381820093561,0.520420576860854,
21.5388491881826));
#17656=CARTESIAN_POINT('Ctrl Pts',(-5.88687297008201,0.599076052517767,
21.5351311396899));
#17657=CARTESIAN_POINT('Ctrl Pts',(-5.87835333985223,0.677588845261338,
21.5314130911971));
#17658=CARTESIAN_POINT('Ctrl Pts',(-5.86826625301487,0.755897973424231,
21.5276950427043));
#17659=CARTESIAN_POINT('Ctrl Pts',(-5.84713742478124,0.919927503927489,
21.5199070649428));
#17660=CARTESIAN_POINT('Ctrl Pts',(-5.81912309060505,1.08309992255365,21.5121190871813));
#17661=CARTESIAN_POINT('Ctrl Pts',(-5.78431725188757,1.24483110983611,21.5043311094198));
#17662=CARTESIAN_POINT('Ctrl Pts',(-5.74951825629639,1.40653049938053,21.4965446628415));
#17663=CARTESIAN_POINT('Ctrl Pts',(-5.70793048760599,1.56678891075884,21.4887582162632));
#17664=CARTESIAN_POINT('Ctrl Pts',(-5.65969899232843,1.72503271816409,21.4809717696849));
#17665=CARTESIAN_POINT('Ctrl Pts',(-5.61146565712806,1.88328256221384,21.4731850260712));
#17666=CARTESIAN_POINT('Ctrl Pts',(-5.55658817757557,2.03951734169757,21.4653982824576));
#17667=CARTESIAN_POINT('Ctrl Pts',(-5.49526160139424,2.19317817213787,21.4576115388439));
#17668=CARTESIAN_POINT('Ctrl Pts',(-5.43393908150707,2.34682883906394,21.4498253102651));
#17669=CARTESIAN_POINT('Ctrl Pts',(-5.36616843716412,2.49790560086805,21.4420390816862));
#17670=CARTESIAN_POINT('Ctrl Pts',(-5.29219309060373,2.64586901683853,21.4342528531074));
#17671=CARTESIAN_POINT('Ctrl Pts',(-5.2181982702991,2.79387138364675,21.4264645748319));
#17672=CARTESIAN_POINT('Ctrl Pts',(-5.13799562521156,2.93875848004927,21.4186762965563));
#17673=CARTESIAN_POINT('Ctrl Pts',(-5.05187523504577,3.08001415127126,21.4108880182808));
#17674=CARTESIAN_POINT('Ctrl Pts',(-4.97000049674338,3.21430605464936,21.4034836945845));
#17675=CARTESIAN_POINT('Ctrl Pts',(-4.88277757354901,3.34531573440166,21.3960793708882));
#17676=CARTESIAN_POINT('Ctrl Pts',(-4.79049269186125,3.47262297575247,21.388675047192));
#17677=CARTESIAN_POINT('Ctrl Pts',(-4.69342608108215,3.60652662518631,21.3808870694305));
#17678=CARTESIAN_POINT('Ctrl Pts',(-4.59072429266484,3.73638186680453,21.3730990916689));
#17679=CARTESIAN_POINT('Ctrl Pts',(-4.48274945839955,3.86172084124662,21.3653111139074));
#17680=CARTESIAN_POINT('Ctrl Pts',(-4.37479585291232,3.98703517297184,21.3575246673291));
#17681=CARTESIAN_POINT('Ctrl Pts',(-4.26157147858543,4.10783476726198,21.3497382207507));
#17682=CARTESIAN_POINT('Ctrl Pts',(-4.14347826165807,4.22368541177809,21.3419517741724));
#17683=CARTESIAN_POINT('Ctrl Pts',(-4.02538053974076,4.33954047573507,21.3341650305587));
#17684=CARTESIAN_POINT('Ctrl Pts',(-3.90241382889769,4.45044598554865,21.3263782869449));
#17685=CARTESIAN_POINT('Ctrl Pts',(-3.7750169000562,4.55600460565944,21.3185915433312));
#17686=CARTESIAN_POINT('Ctrl Pts',(-3.64762839756833,4.66155624385736,21.3108053147523));
#17687=CARTESIAN_POINT('Ctrl Pts',(-3.51581050962268,4.76176149626284,21.3030190861734));
#17688=CARTESIAN_POINT('Ctrl Pts',(-3.38003517269896,4.85626325417166,21.2952328575945));
#17689=CARTESIAN_POINT('Ctrl Pts',(-3.24422409340564,4.9507898893287,21.2874445793189));
#17690=CARTESIAN_POINT('Ctrl Pts',(-3.10445374476293,5.03960984555176,21.2796563010433));
#17691=CARTESIAN_POINT('Ctrl Pts',(-2.96122588211857,5.12240879250876,21.2718680227677));
#17692=CARTESIAN_POINT('Ctrl Pts',(-2.82505901444918,5.20112583153527,21.2644636990716));
#17693=CARTESIAN_POINT('Ctrl Pts',(-2.68576755316882,5.27440108883777,21.2570593753754));
#17694=CARTESIAN_POINT('Ctrl Pts',(-2.54380394709372,5.34200262460161,21.2496550516793));
#17695=CARTESIAN_POINT('Ctrl Pts',(-2.3944845153085,5.41310692511313,21.2418670739178));
#17696=CARTESIAN_POINT('Ctrl Pts',(-2.24215525866555,5.4779593629277,21.2340790961562));
#17697=CARTESIAN_POINT('Ctrl Pts',(-2.08735807654392,5.53632249988987,21.2262911183947));
#17698=CARTESIAN_POINT('Ctrl Pts',(-1.93259132887547,5.59467416215894,21.2185046718164));
#17699=CARTESIAN_POINT('Ctrl Pts',(-1.77535792269628,5.64653895661215,21.210718225238));
#17700=CARTESIAN_POINT('Ctrl Pts',(-1.61621859103658,5.69172803535866,21.2029317786597));
#17701=CARTESIAN_POINT('Ctrl Pts',(-1.4570731885701,5.73691883796666,21.195145035046));
#17702=CARTESIAN_POINT('Ctrl Pts',(-1.29602202144189,5.77543332419271,21.1873582914323));
#17703=CARTESIAN_POINT('Ctrl Pts',(-1.13364052047444,5.80713266017218,21.1795715478186));
#17704=CARTESIAN_POINT('Ctrl Pts',(-0.971269759828443,5.83882989947773,
21.1717853192397));
#17705=CARTESIAN_POINT('Ctrl Pts',(-0.807569155105439,5.86371282947817,
21.1639990906608));
#17706=CARTESIAN_POINT('Ctrl Pts',(-0.643124001080646,5.88169381060711,
21.1562128620819));
#17707=CARTESIAN_POINT('Ctrl Pts',(-0.478635557459758,5.89967952516475,
21.1484245838063));
#17708=CARTESIAN_POINT('Ctrl Pts',(-0.313402490543813,5.91075962357427,
21.1406363055308));
#17709=CARTESIAN_POINT('Ctrl Pts',(-0.148015799356357,5.91489829884174,
21.1328480272552));
#17710=CARTESIAN_POINT('Ctrl Pts',(0.00921748805967901,5.91883294142501,
21.1254437035591));
#17711=CARTESIAN_POINT('Ctrl Pts',(0.166589354157765,5.91649407864731,21.118039379863));
#17712=CARTESIAN_POINT('Ctrl Pts',(0.3235915285177,5.90789464066274,21.1106350561669));
#17713=CARTESIAN_POINT('Ctrl Pts',(0.488728750039722,5.89884962392198,21.1028470784053));
#17714=CARTESIAN_POINT('Ctrl Pts',(0.653516024404402,5.88287478973465,21.0950591006438));
#17715=CARTESIAN_POINT('Ctrl Pts',(0.817363912047738,5.8600210577934,21.0872711228823));
#17716=CARTESIAN_POINT('Ctrl Pts',(0.981179585791571,5.83717181909178,21.079484676304));
#17717=CARTESIAN_POINT('Ctrl Pts',(1.14405592503593,5.80744642528962,21.0716982297256));
#17718=CARTESIAN_POINT('Ctrl Pts',(1.30541021291187,5.77094747320796,21.0639117831473));
#17719=CARTESIAN_POINT('Ctrl Pts',(1.46677065609019,5.73444712877356,21.0561250395336));
#17720=CARTESIAN_POINT('Ctrl Pts',(1.62660861917815,5.69117277564768,21.0483382959199));
#17721=CARTESIAN_POINT('Ctrl Pts',(1.78435242077902,5.6412779581368,21.0405515523062));
#17722=CARTESIAN_POINT('Ctrl Pts',(1.94208578880742,5.59138644079485,21.0327653237273));
#17723=CARTESIAN_POINT('Ctrl Pts',(2.09772496787048,5.53487543184463,21.0249790951484));
#17724=CARTESIAN_POINT('Ctrl Pts',(2.25071412109479,5.4719481455515,21.0171928665695));
#17725=CARTESIAN_POINT('Ctrl Pts',(2.40374354816416,5.40900429387628,21.0094045882939));
#17726=CARTESIAN_POINT('Ctrl Pts',(2.55412125895511,5.3396409095845,21.0016163100184));
#17727=CARTESIAN_POINT('Ctrl Pts',(2.70131121884384,5.26410944618825,20.9938280317428));
#17728=CARTESIAN_POINT('Ctrl Pts',(2.84124485619953,5.19230161081806,20.9864237080466));
#17729=CARTESIAN_POINT('Ctrl Pts',(2.97829724309839,5.11491932754957,20.9790193843505));
#17730=CARTESIAN_POINT('Ctrl Pts',(3.11202830920875,5.03221724145365,20.9716150606543));
#17731=CARTESIAN_POINT('Ctrl Pts',(3.25268863304541,4.94522995756689,20.9638270828928));
#17732=CARTESIAN_POINT('Ctrl Pts',(3.38972462737038,4.85232582752308,20.9560391051313));
#17733=CARTESIAN_POINT('Ctrl Pts',(3.52264313999077,4.75383170408629,20.9482511273697));
#17734=CARTESIAN_POINT('Ctrl Pts',(3.65553551969221,4.65535694543846,20.9404646807914));
#17735=CARTESIAN_POINT('Ctrl Pts',(3.78431177635822,4.55129457644037,20.9326782342131));
#17736=CARTESIAN_POINT('Ctrl Pts',(3.90850939645054,4.44201360425178,20.9248917876347));
#17737=CARTESIAN_POINT('Ctrl Pts',(4.03271175440191,4.33272846324059,20.917105044021));
#17738=CARTESIAN_POINT('Ctrl Pts',(4.15233488376581,4.21822452879402,20.9093183004073));
#17739=CARTESIAN_POINT('Ctrl Pts',(4.26695034700485,4.09891025745809,20.9015315567936));
#17740=CARTESIAN_POINT('Ctrl Pts',(4.38155822928846,3.9796038778686,20.8937453282147));
#17741=CARTESIAN_POINT('Ctrl Pts',(4.49115888695785,3.85548802863711,20.8859590996359));
#17742=CARTESIAN_POINT('Ctrl Pts',(4.59536156929568,3.72700719209668,20.878172871057));
#17743=CARTESIAN_POINT('Ctrl Pts',(4.69959168261532,3.59849253343756,20.8703845927814));
#17744=CARTESIAN_POINT('Ctrl Pts',(4.7984207782104,3.46561083850935,20.8625963145059));
#17745=CARTESIAN_POINT('Ctrl Pts',(4.89149858221775,3.32883946483782,20.8548080362303));
#17746=CARTESIAN_POINT('Ctrl Pts',(4.97998774059283,3.19881078748481,20.8474037125341));
#17747=CARTESIAN_POINT('Ctrl Pts',(5.06327886551453,3.06526692567246,20.839999388838));
#17748=CARTESIAN_POINT('Ctrl Pts',(5.14110746711278,2.92864210413243,20.8325950651418));
#17749=CARTESIAN_POINT('Ctrl Pts',(5.2229687475391,2.78493808530632,20.8248070873803));
#17750=CARTESIAN_POINT('Ctrl Pts',(5.29881567895497,2.63777394526328,20.8170191096188));
#17751=CARTESIAN_POINT('Ctrl Pts',(5.36837172927331,2.48767271537859,20.8092311318573));
#17752=CARTESIAN_POINT('Ctrl Pts',(5.43791410427586,2.33760099668251,20.801444685279));
#17753=CARTESIAN_POINT('Ctrl Pts',(5.50116793177215,2.18459363009707,20.7936582387006));
#17754=CARTESIAN_POINT('Ctrl Pts',(5.55790375823388,2.02919599268029,20.7858717921223));
#17755=CARTESIAN_POINT('Ctrl Pts',(5.61464174903946,1.873792427194,20.7780850485086));
#17756=CARTESIAN_POINT('Ctrl Pts',(5.66486112796053,1.7159987072197,20.7702983048949));
#17757=CARTESIAN_POINT('Ctrl Pts',(5.70838124320544,1.55637853516435,20.7625115612812));
#17758=CARTESIAN_POINT('Ctrl Pts',(5.75189847992031,1.39676892078923,20.7547253327023));
#17759=CARTESIAN_POINT('Ctrl Pts',(5.78871725572671,1.23533340443635,20.7469391041234));
#17760=CARTESIAN_POINT('Ctrl Pts',(5.81870725209061,1.07264927957283,20.7391528755446));
#17761=CARTESIAN_POINT('Ctrl Pts',(5.84870514321332,0.90992232869787,20.731364597269));
#17762=CARTESIAN_POINT('Ctrl Pts',(5.8718706029133,0.745946426626859,20.7235763189934));
#17763=CARTESIAN_POINT('Ctrl Pts',(5.8881245874673,0.581308356178614,20.7157880407178));
#17764=CARTESIAN_POINT('Ctrl Pts',(5.90357726631772,0.424786783222787,20.7083837170217));
#17765=CARTESIAN_POINT('Ctrl Pts',(5.91278348682232,0.267667019912706,20.7009793933255));
#17766=CARTESIAN_POINT('Ctrl Pts',(5.91571887703152,0.110456916636793,20.6935750696293));
#17767=CARTESIAN_POINT('Ctrl Pts',(5.91880636410107,-0.0548990076101417,
20.6857870918678));
#17768=CARTESIAN_POINT('Ctrl Pts',(5.9149570277199,-0.220414033300817,20.6779991141062));
#17769=CARTESIAN_POINT('Ctrl Pts',(5.90417843175445,-0.385496573922004,
20.6702111363447));
#17770=CARTESIAN_POINT('Ctrl Pts',(5.89340195495337,-0.550546657900466,
20.6624246897664));
#17771=CARTESIAN_POINT('Ctrl Pts',(5.87569895766807,-0.715164107794478,
20.654638243188));
#17772=CARTESIAN_POINT('Ctrl Pts',(5.85112903471598,-0.878760252630747,
20.6468517966097));
#17773=CARTESIAN_POINT('Ctrl Pts',(5.82655817447672,-1.0423626382911,20.6390650529959));
#17774=CARTESIAN_POINT('Ctrl Pts',(5.79511990793638,-1.20494332435077,20.6312783093822));
#17775=CARTESIAN_POINT('Ctrl Pts',(5.75692544940485,-1.36592091004376,20.6234915657685));
#17776=CARTESIAN_POINT('Ctrl Pts',(5.71873351715102,-1.52688784827371,20.6157053371896));
#17777=CARTESIAN_POINT('Ctrl Pts',(5.67378636104957,-1.68625158740696,20.6079191086107));
#17778=CARTESIAN_POINT('Ctrl Pts',(5.62224589342328,-1.84344288666208,20.6001328800318));
#17779=CARTESIAN_POINT('Ctrl Pts',(5.57069185795404,-2.00067556596206,20.5923446017562));
#17780=CARTESIAN_POINT('Ctrl Pts',(5.51254114050233,-2.15573435817686,20.5845563234806));
#17781=CARTESIAN_POINT('Ctrl Pts',(5.44800521473027,-2.30806623448544,20.576768045205));
#17782=CARTESIAN_POINT('Ctrl Pts',(5.38665084762466,-2.45288829675714,20.569363721509));
#17783=CARTESIAN_POINT('Ctrl Pts',(5.31952577871153,-2.5952455924653,20.5619593978129));
#17784=CARTESIAN_POINT('Ctrl Pts',(5.24685170089538,-2.73468056476643,20.5545550741168));
#17785=CARTESIAN_POINT('Ctrl Pts',(5.17041202522699,-2.88134034194989,20.5467670963553));
#17786=CARTESIAN_POINT('Ctrl Pts',(5.08780568722297,-3.02481937889032,20.5389791185938));
#17787=CARTESIAN_POINT('Ctrl Pts',(4.99932250106465,-3.1646018853639,20.5311911408323));
#17788=CARTESIAN_POINT('Ctrl Pts',(4.9108567114593,-3.30435690939833,20.523404694254));
#17789=CARTESIAN_POINT('Ctrl Pts',(4.81651654994812,-3.44041658324902,20.5156182476756));
#17790=CARTESIAN_POINT('Ctrl Pts',(4.71663611812378,-3.57229258204171,20.5078318010973));
#17791=CARTESIAN_POINT('Ctrl Pts',(4.61675187608618,-3.7041736116064,20.5000450574836));
#17792=CARTESIAN_POINT('Ctrl Pts',(4.5113271305951,-3.83187038964192,20.4922583138699));
#17793=CARTESIAN_POINT('Ctrl Pts',(4.40073782495855,-3.95492568305387,20.4844715702562));
#17794=CARTESIAN_POINT('Ctrl Pts',(4.29015583397724,-4.07797283727874,20.4766853416773));
#17795=CARTESIAN_POINT('Ctrl Pts',(4.17441018013583,-4.19637888361416,20.4688991130985));
#17796=CARTESIAN_POINT('Ctrl Pts',(4.0539154988253,-4.30972153287008,20.4611128845196));
#17797=CARTESIAN_POINT('Ctrl Pts',(3.93338909772275,-4.42309401917127,20.453324606244));
#17798=CARTESIAN_POINT('Ctrl Pts',(3.80811140263233,-4.53140022442251,20.4455363279685));
#17799=CARTESIAN_POINT('Ctrl Pts',(3.67853280348437,-4.63425581686956,20.4377480496929));
#17800=CARTESIAN_POINT('Ctrl Pts',(3.55534230383321,-4.73204072818043,20.4303437259967));
#17801=CARTESIAN_POINT('Ctrl Pts',(3.42826495227513,-4.82489933704216,20.4229394023005));
#17802=CARTESIAN_POINT('Ctrl Pts',(3.29771441188184,-4.91253602736579,20.4155350786043));
#17803=CARTESIAN_POINT('Ctrl Pts',(3.16039941228764,-5.0047136013534,20.4077471008428));
#17804=CARTESIAN_POINT('Ctrl Pts',(3.0191926220945,-5.09114671724739,20.3999591230813));
#17805=CARTESIAN_POINT('Ctrl Pts',(2.874595389023,-5.1715212376928,20.3921711453197));
#17806=CARTESIAN_POINT('Ctrl Pts',(2.73002658500716,-5.25187995581844,20.3843846987414));
#17807=CARTESIAN_POINT('Ctrl Pts',(2.5820689472871,-5.32618230007899,20.3765982521631));
#17808=CARTESIAN_POINT('Ctrl Pts',(2.43124956100348,-5.39415944653292,20.3688118055848));
#17809=CARTESIAN_POINT('Ctrl Pts',(2.28042442130029,-5.46213918616175,20.361025061971));
#17810=CARTESIAN_POINT('Ctrl Pts',(2.12673760427511,-5.52379311024771,20.3532383183573));
#17811=CARTESIAN_POINT('Ctrl Pts',(1.97073804932283,-5.57889972158052,20.3454515747436));
#17812=CARTESIAN_POINT('Ctrl Pts',(1.814748812574,-5.63400268802328,20.3376653461647));
#17813=CARTESIAN_POINT('Ctrl Pts',(1.65644744538103,-5.68255910198523,20.3298791175859));
#17814=CARTESIAN_POINT('Ctrl Pts',(1.49640013214125,-5.72439666751245,20.322092889007));
#17815=CARTESIAN_POINT('Ctrl Pts',(1.33631068702129,-5.76624524662848,20.3143046107314));
#17816=CARTESIAN_POINT('Ctrl Pts',(1.17447468632175,-5.80137136028579,20.3065163324558));
#17817=CARTESIAN_POINT('Ctrl Pts',(1.01147153781069,-5.82965315355029,20.2987280541803));
#17818=CARTESIAN_POINT('Ctrl Pts',(0.856504286722892,-5.85654068178559,
20.2913237304841));
#17819=CARTESIAN_POINT('Ctrl Pts',(0.700482453865207,-5.87724242544195,
20.2839194067879));
#17820=CARTESIAN_POINT('Ctrl Pts',(0.543910735667616,-5.89169684166841,
20.2765150830917));
#17821=CARTESIAN_POINT('Ctrl Pts',(0.379226274338735,-5.906900211584,20.2687271053302));
#17822=CARTESIAN_POINT('Ctrl Pts',(0.213874519460731,-5.91519709526017,
20.2609391275686));
#17823=CARTESIAN_POINT('Ctrl Pts',(0.0484460197901521,-5.9165516600184,
20.2531511498071));
#17824=CARTESIAN_POINT('Ctrl Pts',(-0.116949955219131,-5.91790595845758,
20.2453647032287));
#17825=CARTESIAN_POINT('Ctrl Pts',(-0.282422325571391,-5.9123206587801,
20.2375782566504));
#17826=CARTESIAN_POINT('Ctrl Pts',(-0.447379635199591,-5.89981203298111,
20.2297918100721));
#17827=CARTESIAN_POINT('Ctrl Pts',(-0.612343237577325,-5.88730293000623,
20.2220050664583));
#17828=CARTESIAN_POINT('Ctrl Pts',(-0.776791420991008,-5.86786999264067,
20.2142183228446));
#17829=CARTESIAN_POINT('Ctrl Pts',(-0.940136195178037,-5.8415815064943,
20.2064315792309));
#17830=CARTESIAN_POINT('Ctrl Pts',(-1.10347016533019,-5.81529475913462,
20.198645350652));
#17831=CARTESIAN_POINT('Ctrl Pts',(-1.26570055680538,-5.78215342129273,
20.1908591220731));
#17832=CARTESIAN_POINT('Ctrl Pts',(-1.42624778932565,-5.7422772317212,20.1830728934942));
#17833=CARTESIAN_POINT('Ctrl Pts',(-1.58683728532817,-5.70239054488601,
20.1752846152186));
#17834=CARTESIAN_POINT('Ctrl Pts',(-1.7457424261921,-5.65576553882389,20.167496336943));
#17835=CARTESIAN_POINT('Ctrl Pts',(-1.90239616603626,-5.60257256891426,
20.1597080586674));
#17836=CARTESIAN_POINT('Ctrl Pts',(-2.05132702815484,-5.55200196092769,
20.1523037349713));
#17837=CARTESIAN_POINT('Ctrl Pts',(-2.19822287625689,-5.49549546282115,
20.1448994112753));
#17838=CARTESIAN_POINT('Ctrl Pts',(-2.34261113016698,-5.43324062188652,
20.1374950875792));
#17839=CARTESIAN_POINT('Ctrl Pts',(-2.49448084259927,-5.36776005449806,
20.1297071098177));
#17840=CARTESIAN_POINT('Ctrl Pts',(-2.64363052703416,-5.29589620577876,
20.1219191320562));
#17841=CARTESIAN_POINT('Ctrl Pts',(-2.78952453188628,-5.21790029116163,
20.1141311542947));
#17842=CARTESIAN_POINT('Ctrl Pts',(-2.93538985272581,-5.13991971121024,
20.1063447077164));
#17843=CARTESIAN_POINT('Ctrl Pts',(-3.0780004895258,-5.05580962148474,20.0985582611381));
#17844=CARTESIAN_POINT('Ctrl Pts',(-3.21684493489036,-4.96586741943139,
20.0907718145598));
#17845=CARTESIAN_POINT('Ctrl Pts',(-3.35569467685802,-4.87592178628547,
20.0829850709461));
#17846=CARTESIAN_POINT('Ctrl Pts',(-3.49077766956498,-4.78014376603094,
20.0751983273324));
#17847=CARTESIAN_POINT('Ctrl Pts',(-3.62161034579687,-4.67887476491059,
20.0674115837187));
#17848=CARTESIAN_POINT('Ctrl Pts',(-3.75243436842581,-4.5776124619772,20.0596253551398));
#17849=CARTESIAN_POINT('Ctrl Pts',(-3.87900838450918,-4.470860100671,20.0518391265609));
#17850=CARTESIAN_POINT('Ctrl Pts',(-4.00088083970663,-4.35900023732144,
20.0440528979821));
#17851=CARTESIAN_POINT('Ctrl Pts',(-4.12278537739019,-4.24711092726461,
20.0362646197065));
#17852=CARTESIAN_POINT('Ctrl Pts',(-4.23998564416529,-4.13011164328848,
20.0284763414309));
#17853=CARTESIAN_POINT('Ctrl Pts',(-4.35206531937162,-4.00842338312993,
20.0206880631554));
#17854=CARTESIAN_POINT('Ctrl Pts',(-4.45861957509171,-3.89273423639395,
20.0132837394592));
#17855=CARTESIAN_POINT('Ctrl Pts',(-4.56054577928273,-3.77280749451314,
20.0058794157629));
#17856=CARTESIAN_POINT('Ctrl Pts',(-4.657518781036,-3.64903403201408,19.9984750920667));
#17857=CARTESIAN_POINT('Ctrl Pts',(-4.75951642621038,-3.51884726372052,
19.9906871143052));
#17858=CARTESIAN_POINT('Ctrl Pts',(-4.85607042852624,-3.38435798624226,
19.9828991365437));
#17859=CARTESIAN_POINT('Ctrl Pts',(-4.94683073646605,-3.24604316472452,
19.9751111587822));
#17860=CARTESIAN_POINT('Ctrl Pts',(-5.03757320015121,-3.10775553708648,
19.9673247122038));
#17861=CARTESIAN_POINT('Ctrl Pts',(-5.1225240670765,-2.96564413314225,19.9595382656255));
#17862=CARTESIAN_POINT('Ctrl Pts',(-5.2013765900554,-2.82021490864148,19.9517518190472));
#17863=CARTESIAN_POINT('Ctrl Pts',(-5.28023212108028,-2.67478013634366,
19.9439650754335));
#17864=CARTESIAN_POINT('Ctrl Pts',(-5.35298868686169,-2.52602756924558,
19.9361783318197));
#17865=CARTESIAN_POINT('Ctrl Pts',(-5.41938513716345,-2.37448842860771,
19.928391588206));
#17866=CARTESIAN_POINT('Ctrl Pts',(-5.48577719583674,-2.22295931115032,
19.9206053596272));
#17867=CARTESIAN_POINT('Ctrl Pts',(-5.54580985271459,-2.0686442817455,19.9128191310483));
#17868=CARTESIAN_POINT('Ctrl Pts',(-5.59926976194931,-1.91209536776284,
19.9050329024694));
#17869=CARTESIAN_POINT('Ctrl Pts',(-5.6527437443131,-1.75550524284093,19.8972446241938));
#17870=CARTESIAN_POINT('Ctrl Pts',(-5.69964141643763,-1.59668036024238,
19.8894563459182));
#17871=CARTESIAN_POINT('Ctrl Pts',(-5.73979876816339,-1.43618963354078,
19.8816680676427));
#17872=CARTESIAN_POINT('Ctrl Pts',(-5.77797640132398,-1.28361094430023,
19.8742637439465));
#17873=CARTESIAN_POINT('Ctrl Pts',(-5.81006222379734,-1.12952695903671,
19.8668594202504));
#17874=CARTESIAN_POINT('Ctrl Pts',(-5.83595785313665,-0.974436503273903,
19.8594550965542));
#17875=CARTESIAN_POINT('Ctrl Pts',(-5.86416048920803,-0.805529247740106,
19.8513911316348));
#17876=CARTESIAN_POINT('Ctrl Pts',(-5.88502802230486,-0.635384442677772,
19.8433271667155));
#17877=CARTESIAN_POINT('Ctrl Pts',(-5.89847849780617,-0.464631007809766,
19.8352632017961));
#17878=CARTESIAN_POINT('Ctrl Pts',(-5.91064803389095,-0.310139065348279,
19.8279671986129));
#17879=CARTESIAN_POINT('Ctrl Pts',(-5.91674657153479,-0.155149150800852,
19.8206711954297));
#17880=CARTESIAN_POINT('Ctrl Pts',(-5.91674999855416,-0.000130802689547563,
19.8133751922466));
#17881=CARTESIAN_POINT('Ctrl Pts',(-5.91680020033354,-0.000151807883381276,
19.5616248077951));
#17882=CARTESIAN_POINT('Ctrl Pts',(-5.9170183524464,-0.211270559939811,
19.5715633135977));
#17883=CARTESIAN_POINT('Ctrl Pts',(-5.85430236710503,-1.40611676514098,
19.6278172811617));
#17884=CARTESIAN_POINT('Ctrl Pts',(-5.0698198637438,-3.51270083870888,19.7303867104881));
#17885=CARTESIAN_POINT('Ctrl Pts',(-2.77132459642368,-5.51016339270765,
19.8693330957729));
#17886=CARTESIAN_POINT('Ctrl Pts',(0.202693088224149,-6.1644996670503,20.0082794810581));
#17887=CARTESIAN_POINT('Ctrl Pts',(3.12730345151057,-5.31621235046608,20.1472258663432));
#17888=CARTESIAN_POINT('Ctrl Pts',(5.28962000410132,-3.17207516387753,20.2861722516285));
#17889=CARTESIAN_POINT('Ctrl Pts',(6.16256868671121,-0.254730867081438,
20.4251186369135));
#17890=CARTESIAN_POINT('Ctrl Pts',(5.53336446324569,2.7247051858812,20.5640650221986));
#17891=CARTESIAN_POINT('Ctrl Pts',(3.55537859832565,5.03998250548997,20.7030114074838));
#17892=CARTESIAN_POINT('Ctrl Pts',(0.710753744830798,6.1267421805791,20.8419577927689));
#17893=CARTESIAN_POINT('Ctrl Pts',(-2.30712042361359,5.7200818162001,20.980904178054));
#17894=CARTESIAN_POINT('Ctrl Pts',(-4.76262395974796,3.91912664392358,21.1198505633391));
#17895=CARTESIAN_POINT('Ctrl Pts',(-5.78975558509219,1.73230762618957,21.230090769941));
#17896=CARTESIAN_POINT('Ctrl Pts',(-5.91658562683898,0.374246943367566,
21.2940155147812));
#17897=CARTESIAN_POINT('Ctrl Pts',(-5.91635768454612,0.000101336159654947,
21.3116247978597));
#17898=CARTESIAN_POINT('Origin',(0.,0.,0.));
#17899=CARTESIAN_POINT('',(-5.91674999852046,-0.000132318339550427,23.3133751922049));
#17900=CARTESIAN_POINT('',(-5.91679629007161,-2.60102882507938E-5,23.0616248077951));
#17901=CARTESIAN_POINT('',(-5.91675,-7.2459289488551E-16,0.));
#17902=CARTESIAN_POINT('Ctrl Pts',(-5.91698239427519,-0.000132148689059992,
23.3133751839731));
#17903=CARTESIAN_POINT('Ctrl Pts',(-5.91617566770858,0.831368591535416,
23.274228452267));
#17904=CARTESIAN_POINT('Ctrl Pts',(-5.52980190076119,2.64788537604627,23.1887417220566));
#17905=CARTESIAN_POINT('Ctrl Pts',(-3.73287084581987,4.9103129984913,23.0569149933421));
#17906=CARTESIAN_POINT('Ctrl Pts',(-0.927040587802708,6.0980401969232,22.9178949978296));
#17907=CARTESIAN_POINT('Ctrl Pts',(2.10499434029924,5.79780107644536,22.7788750023171));
#17908=CARTESIAN_POINT('Ctrl Pts',(4.62339528457857,4.08285617396229,22.6398550068045));
#17909=CARTESIAN_POINT('Ctrl Pts',(6.01365403229901,1.37166456341826,22.5008350112921));
#17910=CARTESIAN_POINT('Ctrl Pts',(5.9365373012305,-1.67422321266426,22.3618150157795));
#17911=CARTESIAN_POINT('Ctrl Pts',(4.41086213664457,-4.31158830435354,22.222795020267));
#17912=CARTESIAN_POINT('Ctrl Pts',(1.80890441491952,-5.89689437860388,22.0837750247545));
#17913=CARTESIAN_POINT('Ctrl Pts',(-1.2344391876144,-6.04331518181912,21.9447550292419));
#17914=CARTESIAN_POINT('Ctrl Pts',(-3.97657061794283,-4.71512296925953,
21.8057350337294));
#17915=CARTESIAN_POINT('Ctrl Pts',(-5.59680782494173,-2.44846451161869,
21.6786084213838));
#17916=CARTESIAN_POINT('Ctrl Pts',(-5.9159378649533,-0.731625187597263,
21.5978218075423));
#17917=CARTESIAN_POINT('Ctrl Pts',(-5.91666999553354,0.000153478058687734,
21.5633751922049));
#17918=CARTESIAN_POINT('Ctrl Pts',(-5.91674999913571,0.000101131768199252,
21.3116248077951));
#17919=CARTESIAN_POINT('Ctrl Pts',(-5.91675283436531,-0.165774982607078,
21.3194313027863));
#17920=CARTESIAN_POINT('Ctrl Pts',(-5.90977581898218,-0.331653191667966,
21.3272377977775));
#17921=CARTESIAN_POINT('Ctrl Pts',(-5.89584447824603,-0.496939081614436,
21.3350442927687));
#17922=CARTESIAN_POINT('Ctrl Pts',(-5.88191337714267,-0.662222128480592,
21.3428506534805));
#17923=CARTESIAN_POINT('Ctrl Pts',(-5.86102821913857,-0.826912561854687,
21.3506570141923));
#17924=CARTESIAN_POINT('Ctrl Pts',(-5.83326645319524,-0.990420642215763,
21.3584633749042));
#17925=CARTESIAN_POINT('Ctrl Pts',(-5.80549747038832,-1.15397122763628,
21.3662717649336));
#17926=CARTESIAN_POINT('Ctrl Pts',(-5.77084836046043,-1.31633853411121,
21.374080154963));
#17927=CARTESIAN_POINT('Ctrl Pts',(-5.72944794534782,-1.47694170638169,
21.3818885449924));
#17928=CARTESIAN_POINT('Ctrl Pts',(-5.70142702425242,-1.58564227872186,
21.3871734746314));
#17929=CARTESIAN_POINT('Ctrl Pts',(-5.67031442946143,-1.69353490763636,
21.3924584042704));
#17930=CARTESIAN_POINT('Ctrl Pts',(-5.63616319163506,-1.80044301208289,
21.3977433339094));
#17931=CARTESIAN_POINT('Ctrl Pts',(-5.58583638265805,-1.95798763104894,
21.4055314453024));
#17932=CARTESIAN_POINT('Ctrl Pts',(-5.52889081211639,-2.11344891743199,
21.4133195566954));
#17933=CARTESIAN_POINT('Ctrl Pts',(-5.46552416448239,-2.26626921833198,
21.4211076680883));
#17934=CARTESIAN_POINT('Ctrl Pts',(-5.40216995778514,-2.41905951562963,
21.4288942504214));
#17935=CARTESIAN_POINT('Ctrl Pts',(-5.33239731171228,-2.56920956705058,
21.4366808327544));
#17936=CARTESIAN_POINT('Ctrl Pts',(-5.2564522307488,-2.71618123628671,21.4444674150875));
#17937=CARTESIAN_POINT('Ctrl Pts',(-5.18050425401615,-2.86315850952013,
21.4522542943212));
#17938=CARTESIAN_POINT('Ctrl Pts',(-5.09838351462145,-3.00695687239445,
21.4600411735549));
#17939=CARTESIAN_POINT('Ctrl Pts',(-5.01038254501075,-3.14706169547908,
21.4678280527886));
#17940=CARTESIAN_POINT('Ctrl Pts',(-4.9223873834131,-3.28715727172648,21.4756144180927));
#17941=CARTESIAN_POINT('Ctrl Pts',(-4.82851293829791,-3.42355952546908,
21.4834007833969));
#17942=CARTESIAN_POINT('Ctrl Pts',(-4.72909582324789,-3.55578166610935,
21.4911871487011));
#17943=CARTESIAN_POINT('Ctrl Pts',(-4.62965260328237,-3.68803852559864,
21.4989755585467));
#17944=CARTESIAN_POINT('Ctrl Pts',(-4.52466399580566,-3.81611282200139,
21.5067639683923));
#17945=CARTESIAN_POINT('Ctrl Pts',(-4.41450831381967,-3.9395490744141,21.5145523782378));
#17946=CARTESIAN_POINT('Ctrl Pts',(-4.3101415286957,-4.0564985099748,21.5219314918901));
#17947=CARTESIAN_POINT('Ctrl Pts',(-4.20113695372893,-4.16928464594976,
21.5293106055423));
#17948=CARTESIAN_POINT('Ctrl Pts',(-4.08784812513602,-4.27754932973565,
21.5366897191945));
#17949=CARTESIAN_POINT('Ctrl Pts',(-3.96828010406435,-4.3918147357162,21.5444778305874));
#17950=CARTESIAN_POINT('Ctrl Pts',(-3.8438967371534,-4.5010840708657,21.5522659419804));
#17951=CARTESIAN_POINT('Ctrl Pts',(-3.71513841646305,-4.60496222666597,
21.5600540533733));
#17952=CARTESIAN_POINT('Ctrl Pts',(-3.58640537522402,-4.70881998780151,
21.5678406357064));
#17953=CARTESIAN_POINT('Ctrl Pts',(-3.45329934259107,-4.80728848102971,
21.5756272180395));
#17954=CARTESIAN_POINT('Ctrl Pts',(-3.31629380410436,-4.90001285379528,
21.5834138003725));
#17955=CARTESIAN_POINT('Ctrl Pts',(-3.17928304162731,-4.99274076212033,
21.5912006796062));
#17956=CARTESIAN_POINT('Ctrl Pts',(-3.03837273817019,-5.0797239293635,21.5989875588399));
#17957=CARTESIAN_POINT('Ctrl Pts',(-2.89406599001871,-5.16065040551257,
21.6067744380736));
#17958=CARTESIAN_POINT('Ctrl Pts',(-2.74976876602898,-5.24157154056111,
21.6145608033778));
#17959=CARTESIAN_POINT('Ctrl Pts',(-2.60207582470565,-5.31643662825231,
21.622347168682));
#17960=CARTESIAN_POINT('Ctrl Pts',(-2.45151565190734,-5.38497925445896,
21.6301335339862));
#17961=CARTESIAN_POINT('Ctrl Pts',(-2.30091594506516,-5.45353987856731,
21.6379219438318));
#17962=CARTESIAN_POINT('Ctrl Pts',(-2.14744779254099,-5.5157745896197,21.6457103536774));
#17963=CARTESIAN_POINT('Ctrl Pts',(-1.99166131774356,-5.57146441771856,
21.653498763523));
#17964=CARTESIAN_POINT('Ctrl Pts',(-1.84406172735252,-5.62422763626515,
21.6608778771752));
#17965=CARTESIAN_POINT('Ctrl Pts',(-1.69438145717131,-5.6711160842054,21.6682569908274));
#17966=CARTESIAN_POINT('Ctrl Pts',(-1.543102308257,-5.71198440375601,21.6756361044796));
#17967=CARTESIAN_POINT('Ctrl Pts',(-1.38343829998868,-5.75511790733183,
21.6834242158726));
#17968=CARTESIAN_POINT('Ctrl Pts',(-1.22193612308707,-5.79156041581149,
21.6912123272656));
#17969=CARTESIAN_POINT('Ctrl Pts',(-1.05917152972064,-5.82117567447756,
21.6990004386586));
#17970=CARTESIAN_POINT('Ctrl Pts',(-0.896438892344492,-5.8507851187039,
21.7067870209916));
#17971=CARTESIAN_POINT('Ctrl Pts',(-0.732444647217814,-5.87356993047183,
21.7145736033247));
#17972=CARTESIAN_POINT('Ctrl Pts',(-0.567774346777329,-5.8894450378318,
21.7223601856578));
#17973=CARTESIAN_POINT('Ctrl Pts',(-0.403097767495121,-5.90532075050606,
21.7301470648915));
#17974=CARTESIAN_POINT('Ctrl Pts',(-0.23774539898002,-5.91428619698674,
21.7379339441252));
#17975=CARTESIAN_POINT('Ctrl Pts',(-0.0723082694507838,-5.91630814585152,
21.745720823359));
#17976=CARTESIAN_POINT('Ctrl Pts',(0.0931179413234977,-5.91832996126884,
21.7535071886632));
#17977=CARTESIAN_POINT('Ctrl Pts',(0.258628582386181,-5.91340919234525,
21.7612935539674));
#17978=CARTESIAN_POINT('Ctrl Pts',(0.423632116328124,-5.9015647410255,21.7690799192715));
#17979=CARTESIAN_POINT('Ctrl Pts',(0.588678976847425,-5.88971717959335,
21.7768683291171));
#17980=CARTESIAN_POINT('Ctrl Pts',(0.75321814511539,-5.87094232394192,21.7846567389628));
#17981=CARTESIAN_POINT('Ctrl Pts',(0.916661782288731,-5.84531109004399,
21.7924451488084));
#17982=CARTESIAN_POINT('Ctrl Pts',(1.07151613617246,-5.82102682769429,21.7998242624605));
#17983=CARTESIAN_POINT('Ctrl Pts',(1.2253868850502,-5.79058832459067,21.8072033761127));
#17984=CARTESIAN_POINT('Ctrl Pts',(1.37778140412653,-5.75409844936139,21.8145824897648));
#17985=CARTESIAN_POINT('Ctrl Pts',(1.53862260351614,-5.71558607153424,21.8223706011578));
#17986=CARTESIAN_POINT('Ctrl Pts',(1.69787673273818,-5.67031873348632,21.8301587125507));
#17987=CARTESIAN_POINT('Ctrl Pts',(1.85497302160941,-5.61845224698059,21.8379468239437));
#17988=CARTESIAN_POINT('Ctrl Pts',(2.01203846736361,-5.56659594355509,21.8457334062768));
#17989=CARTESIAN_POINT('Ctrl Pts',(2.16694661485152,-5.50814317694852,21.8535199886099));
#17990=CARTESIAN_POINT('Ctrl Pts',(2.31914257569174,-5.44329939247456,21.861306570943));
#17991=CARTESIAN_POINT('Ctrl Pts',(2.47134433972939,-5.37845313552182,21.8690934501767));
#17992=CARTESIAN_POINT('Ctrl Pts',(2.62083341468959,-5.30721549468745,21.8768803294104));
#17993=CARTESIAN_POINT('Ctrl Pts',(2.76707490611802,-5.22984005744267,21.8846672086441));
#17994=CARTESIAN_POINT('Ctrl Pts',(2.9133067456928,-5.15246972693189,21.8924535739483));
#17995=CARTESIAN_POINT('Ctrl Pts',(3.05629114826095,-5.06896256020916,21.9002399392525));
#17996=CARTESIAN_POINT('Ctrl Pts',(3.1955177146777,-4.97961816785996,21.9080263045567));
#17997=CARTESIAN_POINT('Ctrl Pts',(3.33478083916337,-4.89025031548775,21.9158147144023));
#17998=CARTESIAN_POINT('Ctrl Pts',(3.47028388565757,-4.79504234581187,21.9236031242479));
#17999=CARTESIAN_POINT('Ctrl Pts',(3.60154458815585,-4.69433777459881,21.9313915340935));
#18000=CARTESIAN_POINT('Ctrl Pts',(3.72590728362201,-4.59892542586494,21.9387706477456));
#18001=CARTESIAN_POINT('Ctrl Pts',(3.84646184728199,-4.49857948916574,21.9461497613978));
#18002=CARTESIAN_POINT('Ctrl Pts',(3.96282491003736,-4.39362598486574,21.9535288750499));
#18003=CARTESIAN_POINT('Ctrl Pts',(4.08563755902043,-4.28285528514432,21.9613169864429));
#18004=CARTESIAN_POINT('Ctrl Pts',(4.20382475428739,-4.16691221099511,21.9691050978358));
#18005=CARTESIAN_POINT('Ctrl Pts',(4.31695983535354,-4.04620666086698,21.9768932092288));
#18006=CARTESIAN_POINT('Ctrl Pts',(4.43007270431869,-3.92552480916948,21.9846797915619));
#18007=CARTESIAN_POINT('Ctrl Pts',(4.53813521983098,-3.80008258014354,21.9924663738949));
#18008=CARTESIAN_POINT('Ctrl Pts',(4.64075841401936,-3.67032585817778,22.000252956228));
#18009=CARTESIAN_POINT('Ctrl Pts',(4.74338552120726,-3.54056418861716,22.0080398354617));
#18010=CARTESIAN_POINT('Ctrl Pts',(4.84057269076204,-3.40648794509135,22.0158267146954));
#18011=CARTESIAN_POINT('Ctrl Pts',(4.93197154484231,-3.26857572091665,22.0236135939291));
#18012=CARTESIAN_POINT('Ctrl Pts',(5.023364366651,-3.13067259886908,22.0313999592333));
#18013=CARTESIAN_POINT('Ctrl Pts',(5.10896946104505,-2.98893426924202,22.0391863245374));
#18014=CARTESIAN_POINT('Ctrl Pts',(5.1884819791543,-2.84386801987909,22.0469726898416));
#18015=CARTESIAN_POINT('Ctrl Pts',(5.26801537563628,-2.69876367906471,22.0547610996872));
#18016=CARTESIAN_POINT('Ctrl Pts',(5.34145284374213,-2.55032995184205,22.0625495095328));
#18017=CARTESIAN_POINT('Ctrl Pts',(5.40853524474125,-2.39909922030992,22.0703379193784));
#18018=CARTESIAN_POINT('Ctrl Pts',(5.47209233416618,-2.25581595995212,22.0777170330306));
#18019=CARTESIAN_POINT('Ctrl Pts',(5.52994501366636,-2.11002234793038,22.0850961466828));
#18020=CARTESIAN_POINT('Ctrl Pts',(5.58191261772456,-1.96218808746443,22.092475260335));
#18021=CARTESIAN_POINT('Ctrl Pts',(5.63676059924473,-1.80615990542622,22.100263371728));
#18022=CARTESIAN_POINT('Ctrl Pts',(5.68507221795039,-1.64780272350431,22.1080514831209));
#18023=CARTESIAN_POINT('Ctrl Pts',(5.72666892340327,-1.48768061230469,22.1158395945139));
#18024=CARTESIAN_POINT('Ctrl Pts',(5.7682574620681,-1.32758993829054,22.1236261768469));
#18025=CARTESIAN_POINT('Ctrl Pts',(5.8031336377015,-1.16573533546769,22.13141275918));
#18026=CARTESIAN_POINT('Ctrl Pts',(5.83116921555223,-1.00269444104172,22.139199341513));
#18027=CARTESIAN_POINT('Ctrl Pts',(5.85920586239332,-0.839647329902619,
22.1469862207467));
#18028=CARTESIAN_POINT('Ctrl Pts',(5.88040133149115,-0.675414150874227,
22.1547730999804));
#18029=CARTESIAN_POINT('Ctrl Pts',(5.89467868023039,-0.510581843916649,
22.1625599792141));
#18030=CARTESIAN_POINT('Ctrl Pts',(5.9089550866729,-0.345760415795667,22.1703463445183));
#18031=CARTESIAN_POINT('Ctrl Pts',(5.91631425900929,-0.180340257246796,
22.1781327098225));
#18032=CARTESIAN_POINT('Ctrl Pts',(5.91673120688126,-0.0149126797547105,
22.1859190751267));
#18033=CARTESIAN_POINT('Ctrl Pts',(5.91714826423527,0.150558335659481,22.1937074849723));
#18034=CARTESIAN_POINT('Ctrl Pts',(5.91061945186923,0.316036454176732,22.2014958948179));
#18035=CARTESIAN_POINT('Ctrl Pts',(5.8971719245184,0.480930197816694,22.2092843046635));
#18036=CARTESIAN_POINT('Ctrl Pts',(5.88443109107096,0.637158452233363,22.2166634183157));
#18037=CARTESIAN_POINT('Ctrl Pts',(5.86548004429649,0.792861912881908,22.2240425319679));
#18038=CARTESIAN_POINT('Ctrl Pts',(5.84038486026414,0.947541685889016,22.2314216456201));
#18039=CARTESIAN_POINT('Ctrl Pts',(5.81389874040172,1.11079480261757,22.2392097570131));
#18040=CARTESIAN_POINT('Ctrl Pts',(5.78055861547604,1.27296584083992,22.246997868406));
#18041=CARTESIAN_POINT('Ctrl Pts',(5.74047756754068,1.43347405245517,22.254785979799));
#18042=CARTESIAN_POINT('Ctrl Pts',(5.70040438882025,1.59395075108161,22.2625725621321));
#18043=CARTESIAN_POINT('Ctrl Pts',(5.65359300515733,1.75276496468208,22.2703591444652));
#18044=CARTESIAN_POINT('Ctrl Pts',(5.60020717269849,1.90934810481389,22.2781457267983));
#18045=CARTESIAN_POINT('Ctrl Pts',(5.54681930464972,2.06593721542604,22.285932606032));
#18046=CARTESIAN_POINT('Ctrl Pts',(5.48685658556098,2.2202947786477,22.2937194852657));
#18047=CARTESIAN_POINT('Ctrl Pts',(5.42053226314005,2.37186857704169,22.3015063644995));
#18048=CARTESIAN_POINT('Ctrl Pts',(5.35421231808629,2.52343237165208,22.3092927298036));
#18049=CARTESIAN_POINT('Ctrl Pts',(5.28153173811755,2.67221247639429,22.3170790951078));
#18050=CARTESIAN_POINT('Ctrl Pts',(5.2027514828959,2.81767769088739,22.324865460412));
#18051=CARTESIAN_POINT('Ctrl Pts',(5.12395054157881,2.96318110159224,22.3326538702576));
#18052=CARTESIAN_POINT('Ctrl Pts',(5.03904687513562,3.10536760068265,22.3404422801032));
#18053=CARTESIAN_POINT('Ctrl Pts',(4.94834731268275,3.24373078962564,22.3482306899489));
#18054=CARTESIAN_POINT('Ctrl Pts',(4.86241418990062,3.37482272196152,22.355609803601));
#18055=CARTESIAN_POINT('Ctrl Pts',(4.77127881688351,3.50248263585952,22.3629889172532));
#18056=CARTESIAN_POINT('Ctrl Pts',(4.6752379049579,3.62630405434306,22.3703680309053));
#18057=CARTESIAN_POINT('Ctrl Pts',(4.57387379056434,3.75698844889836,22.3781561422983));
#18058=CARTESIAN_POINT('Ctrl Pts',(4.46700872238724,3.88344344789723,22.3859442536913));
#18059=CARTESIAN_POINT('Ctrl Pts',(4.35501985072996,4.00521318561796,22.3937323650843));
#18060=CARTESIAN_POINT('Ctrl Pts',(4.24305296613534,4.12695901597349,22.4015189474173));
#18061=CARTESIAN_POINT('Ctrl Pts',(4.12596450143291,4.2440211854203,22.4093055297504));
#18062=CARTESIAN_POINT('Ctrl Pts',(4.00417028739454,4.35597875018311,22.4170921120835));
#18063=CARTESIAN_POINT('Ctrl Pts',(3.88237142937008,4.46794058386276,22.4248789913172));
#18064=CARTESIAN_POINT('Ctrl Pts',(3.75586669553092,4.57479720424914,22.4326658705509));
#18065=CARTESIAN_POINT('Ctrl Pts',(3.62510754385212,4.67616572182878,22.4404527497846));
#18066=CARTESIAN_POINT('Ctrl Pts',(3.49435702220181,4.7775275491448,22.4482391150888));
#18067=CARTESIAN_POINT('Ctrl Pts',(3.35935289723786,4.87340180280263,22.456025480393));
#18068=CARTESIAN_POINT('Ctrl Pts',(3.22057846859065,4.96344687592708,22.4638118456971));
#18069=CARTESIAN_POINT('Ctrl Pts',(3.08176760059654,5.05351559305921,22.4716002555427));
#18070=CARTESIAN_POINT('Ctrl Pts',(2.93918471784839,5.13775189548406,22.4793886653883));
#18071=CARTESIAN_POINT('Ctrl Pts',(2.79334153291282,5.21585790095975,22.4871770752339));
#18072=CARTESIAN_POINT('Ctrl Pts',(2.65516269302536,5.28985928285252,22.4945561888861));
#18073=CARTESIAN_POINT('Ctrl Pts',(2.51405763710387,5.35835799105085,22.5019353025382));
#18074=CARTESIAN_POINT('Ctrl Pts',(2.37048138705646,5.4211390460049,22.5093144161904));
#18075=CARTESIAN_POINT('Ctrl Pts',(2.21894722164553,5.48739982912841,22.5171025275834));
#18076=CARTESIAN_POINT('Ctrl Pts',(2.06460603512822,5.54731483319738,22.5248906389763));
#18077=CARTESIAN_POINT('Ctrl Pts',(1.90800711403173,5.60066419412058,22.5326787503693));
#18078=CARTESIAN_POINT('Ctrl Pts',(1.75143893840424,5.65400308082652,22.5404653327023));
#18079=CARTESIAN_POINT('Ctrl Pts',(1.59261421491847,5.70077879344744,22.5482519150353));
#18080=CARTESIAN_POINT('Ctrl Pts',(1.43209948841326,5.7408206397506,22.5560384973683));
#18081=CARTESIAN_POINT('Ctrl Pts',(1.2715786415162,5.78086401284071,22.563825376602));
#18082=CARTESIAN_POINT('Ctrl Pts',(1.10936797171594,5.81417292466735,22.5716122558357));
#18083=CARTESIAN_POINT('Ctrl Pts',(0.94604710241093,5.8406271446241,22.5793991350695));
#18084=CARTESIAN_POINT('Ctrl Pts',(0.782737012188957,5.86707961861761,22.5871855003736));
#18085=CARTESIAN_POINT('Ctrl Pts',(0.618317184552772,5.8866782550966,22.5949718656778));
#18086=CARTESIAN_POINT('Ctrl Pts',(0.453375452715306,5.89935430885238,22.602758230982));
#18087=CARTESIAN_POINT('Ctrl Pts',(0.288390410528627,5.91203369108247,22.6105466408276));
#18088=CARTESIAN_POINT('Ctrl Pts',(0.122883508953181,5.91778683195085,22.6183350506732));
#18089=CARTESIAN_POINT('Ctrl Pts',(-0.0425533881567151,5.91659697559808,
22.6261234605188));
#18090=CARTESIAN_POINT('Ctrl Pts',(-0.199296252265106,5.91546964852735,
22.633502574171));
#18091=CARTESIAN_POINT('Ctrl Pts',(-0.355976020328041,5.90811029313864,
22.6408816878233));
#18092=CARTESIAN_POINT('Ctrl Pts',(-0.512090273423788,5.89454782950862,
22.6482608014755));
#18093=CARTESIAN_POINT('Ctrl Pts',(-0.676857378314673,5.88023364727865,
22.6560489128685));
#18094=CARTESIAN_POINT('Ctrl Pts',(-0.841053348037998,5.85900411372562,
22.6638370242614));
#18095=CARTESIAN_POINT('Ctrl Pts',(-1.00409065082147,5.83092895921678,22.6716251356544));
#18096=CARTESIAN_POINT('Ctrl Pts',(-1.16709594407423,5.80285931677485,22.6794117179876));
#18097=CARTESIAN_POINT('Ctrl Pts',(-1.32894270958611,5.76794678928466,22.6871983003207));
#18098=CARTESIAN_POINT('Ctrl Pts',(-1.4890517862185,5.72631254302972,22.6949848826538));
#18099=CARTESIAN_POINT('Ctrl Pts',(-1.64916696777306,5.68467670927057,22.7027717618876));
#18100=CARTESIAN_POINT('Ctrl Pts',(-1.807544017641,5.63631872048542,22.7105586411213));
#18101=CARTESIAN_POINT('Ctrl Pts',(-1.96361643272343,5.58141031170783,22.718345520355));
#18102=CARTESIAN_POINT('Ctrl Pts',(-2.11967854711662,5.5265055268535,22.7261318856592));
#18103=CARTESIAN_POINT('Ctrl Pts',(-2.27343602970581,5.4650512933161,22.7339182509634));
#18104=CARTESIAN_POINT('Ctrl Pts',(-2.42433980059651,5.39726848449692,22.7417046162676));
#18105=CARTESIAN_POINT('Ctrl Pts',(-2.57528319575281,5.32946787728872,22.7494930261132));
#18106=CARTESIAN_POINT('Ctrl Pts',(-2.72337108943805,5.25533550350466,22.7572814359588));
#18107=CARTESIAN_POINT('Ctrl Pts',(-2.86807573589755,5.17513981798132,22.7650698458044));
#18108=CARTESIAN_POINT('Ctrl Pts',(-3.00517586973449,5.09915857282157,22.7724489594565));
#18109=CARTESIAN_POINT('Ctrl Pts',(-3.1392389753819,5.0177350287138,22.7798280731085));
#18110=CARTESIAN_POINT('Ctrl Pts',(-3.26983770370068,4.93113495596678,22.7872071867606));
#18111=CARTESIAN_POINT('Ctrl Pts',(-3.40767505001123,4.8397349525256,22.7949952981536));
#18112=CARTESIAN_POINT('Ctrl Pts',(-3.54170232156009,4.74253567243889,22.8027834095466));
#18113=CARTESIAN_POINT('Ctrl Pts',(-3.6714369547534,4.63987944345228,22.8105715209395));
#18114=CARTESIAN_POINT('Ctrl Pts',(-3.801146116813,4.53724336922675,22.8183581032726));
#18115=CARTESIAN_POINT('Ctrl Pts',(-3.92656407170557,4.42915268196657,22.8261446856056));
#18116=CARTESIAN_POINT('Ctrl Pts',(-4.04724021503789,4.3159908716632,22.8339312679387));
#18117=CARTESIAN_POINT('Ctrl Pts',(-4.16792095972478,4.20282474652511,22.8417181471724));
#18118=CARTESIAN_POINT('Ctrl Pts',(-4.28385929528953,4.0845873271073,22.8495050264061));
#18119=CARTESIAN_POINT('Ctrl Pts',(-4.39463992652577,3.96170045292241,22.8572919056399));
#18120=CARTESIAN_POINT('Ctrl Pts',(-4.50541324630485,3.83882168919966,22.8650782709441));
#18121=CARTESIAN_POINT('Ctrl Pts',(-4.61102932908215,3.71129432221224,22.8728646362483));
#18122=CARTESIAN_POINT('Ctrl Pts',(-4.71111168889278,3.57957500511971,22.8806510015525));
#18123=CARTESIAN_POINT('Ctrl Pts',(-4.81122032829831,3.44782110120989,22.8884394113981));
#18124=CARTESIAN_POINT('Ctrl Pts',(-4.90579214626941,3.31187330113712,22.8962278212437));
#18125=CARTESIAN_POINT('Ctrl Pts',(-4.99449215547285,3.17221983340061,22.9040162310893));
#18126=CARTESIAN_POINT('Ctrl Pts',(-5.0785308054458,3.03990542894886,22.9113953447415));
#18127=CARTESIAN_POINT('Ctrl Pts',(-5.1572987839082,2.90426503894494,22.9187744583936));
#18128=CARTESIAN_POINT('Ctrl Pts',(-5.23054797971386,2.7657365012617,22.9261535720458));
#18129=CARTESIAN_POINT('Ctrl Pts',(-5.30777049503581,2.61969364022941,22.9339329573455));
#18130=CARTESIAN_POINT('Ctrl Pts',(-5.37888704971622,2.47038729732537,22.9417123426452));
#18131=CARTESIAN_POINT('Ctrl Pts',(-5.44363799286681,2.3183476799473,22.949491727945));
#18132=CARTESIAN_POINT('Ctrl Pts',(-5.50837596849685,2.16633851118923,22.9572695552853));
#18133=CARTESIAN_POINT('Ctrl Pts',(-5.56675075047658,2.01159745524634,22.9650473826256));
#18134=CARTESIAN_POINT('Ctrl Pts',(-5.6185504355893,1.85467559568763,22.972825209966));
#18135=CARTESIAN_POINT('Ctrl Pts',(-5.67035169468284,1.69774896791468,22.9806032736427));
#18136=CARTESIAN_POINT('Ctrl Pts',(-5.71557735280554,1.53864170748293,22.9883813373194));
#18137=CARTESIAN_POINT('Ctrl Pts',(-5.75406486082589,1.37792167408336,22.9961594009962));
#18138=CARTESIAN_POINT('Ctrl Pts',(-5.79255008650999,1.21721117149464,23.0039370034283));
#18139=CARTESIAN_POINT('Ctrl Pts',(-5.82429788733408,1.05488839958225,23.0117146058604));
#18140=CARTESIAN_POINT('Ctrl Pts',(-5.84919644761066,0.891533218539163,
23.0194922082925));
#18141=CARTESIAN_POINT('Ctrl Pts',(-5.8741012472323,0.728137102223913,23.0272717597186));
#18142=CARTESIAN_POINT('Ctrl Pts',(-5.89215332718016,0.563708377132532,
23.0350513111447));
#18143=CARTESIAN_POINT('Ctrl Pts',(-5.90329242289988,0.398834717938238,
23.0428308625709));
#18144=CARTESIAN_POINT('Ctrl Pts',(-5.91226241544131,0.266066714999467,
23.0490955109789));
#18145=CARTESIAN_POINT('Ctrl Pts',(-5.91675058477204,0.133010396746608,
23.055360159387));
#18146=CARTESIAN_POINT('Ctrl Pts',(-5.91674999994283,-2.60100847582463E-5,
23.0616248077951));
#18147=CARTESIAN_POINT('Origin',(0.,0.,0.));
#18148=CARTESIAN_POINT('',(-5.91671817690238,6.02334792636984E-5,25.0633751914214));
#18149=CARTESIAN_POINT('',(-5.91628298387923,-6.23028472571992E-5,24.8116248077951));
#18150=CARTESIAN_POINT('',(-5.91675,-7.2459289488551E-16,0.));
#18151=CARTESIAN_POINT('Ctrl Pts',(-5.91674999969339,6.02350095563548E-5,
25.0633751913646));
#18152=CARTESIAN_POINT('Ctrl Pts',(-5.9167482813348,0.168850748591878,25.0554319459057));
#18153=CARTESIAN_POINT('Ctrl Pts',(-5.90951944838277,0.337616774232801,
25.0474887004468));
#18154=CARTESIAN_POINT('Ctrl Pts',(-5.89509576569253,0.505743488157823,
25.0395454549879));
#18155=CARTESIAN_POINT('Ctrl Pts',(-5.88066728875627,0.673926085233122,
25.0315995692967));
#18156=CARTESIAN_POINT('Ctrl Pts',(-5.8590392095019,0.841468655864555,25.0236536836055));
#18157=CARTESIAN_POINT('Ctrl Pts',(-5.83029570048855,1.00776118568081,25.0157077979143));
#18158=CARTESIAN_POINT('Ctrl Pts',(-5.81520765237642,1.0950514914465,25.0115368421153));
#18159=CARTESIAN_POINT('Ctrl Pts',(-5.79815987057062,1.18199747634926,25.0073658863163));
#18160=CARTESIAN_POINT('Ctrl Pts',(-5.77917018964272,1.2685119162408,25.0031949305173));
#18161=CARTESIAN_POINT('Ctrl Pts',(-5.74371279812575,1.43005103734313,24.9954069527558));
#18162=CARTESIAN_POINT('Ctrl Pts',(-5.70147182161497,1.59013145782957,24.9876189749943));
#18163=CARTESIAN_POINT('Ctrl Pts',(-5.65259221389059,1.74817957486165,24.9798309972328));
#18164=CARTESIAN_POINT('Ctrl Pts',(-5.60372221631618,1.90619661827886,24.9720445506545));
#18165=CARTESIAN_POINT('Ctrl Pts',(-5.54821628616727,2.06218185040195,24.9642581040762));
#18166=CARTESIAN_POINT('Ctrl Pts',(-5.48626930308796,2.21557660587369,24.9564716574979));
#18167=CARTESIAN_POINT('Ctrl Pts',(-5.4243199568709,2.36897721300953,24.9486849138842));
#18168=CARTESIAN_POINT('Ctrl Pts',(-5.35592918203759,2.51978684798059,24.9408981702705));
#18169=CARTESIAN_POINT('Ctrl Pts',(-5.28134037106795,2.66746592244922,24.9331114266568));
#18170=CARTESIAN_POINT('Ctrl Pts',(-5.20675649359011,2.81513522905196,24.925325198078));
#18171=CARTESIAN_POINT('Ctrl Pts',(-5.12597554453162,2.95967410431085,24.9175389694991));
#18172=CARTESIAN_POINT('Ctrl Pts',(-5.03928739568512,3.10056657825455,24.9097527409203));
#18173=CARTESIAN_POINT('Ctrl Pts',(-4.9525764264949,3.2414961416358,24.9019644626447));
#18174=CARTESIAN_POINT('Ctrl Pts',(-4.85995531610111,3.37877711224864,24.8941761843692));
#18175=CARTESIAN_POINT('Ctrl Pts',(-4.76175836765831,3.51192081495812,24.8863879060936));
#18176=CARTESIAN_POINT('Ctrl Pts',(-4.66840243371112,3.63850066201793,24.8789835823973));
#18177=CARTESIAN_POINT('Ctrl Pts',(-4.57000734182423,3.7613411293395,24.8715792587011));
#18178=CARTESIAN_POINT('Ctrl Pts',(-4.46689512826243,3.88004877232302,24.8641749350048));
#18179=CARTESIAN_POINT('Ctrl Pts',(-4.35844016882194,4.00490723632386,24.8563869572433));
#18180=CARTESIAN_POINT('Ctrl Pts',(-4.24472747883706,4.12523788601996,24.8485989794818));
#18181=CARTESIAN_POINT('Ctrl Pts',(-4.1261588921345,4.24060648485089,24.8408110017203));
#18182=CARTESIAN_POINT('Ctrl Pts',(-4.00761361703259,4.35595240122621,24.8330245551419));
#18183=CARTESIAN_POINT('Ctrl Pts',(-3.88421457902726,4.46633799060161,24.8252381085636));
#18184=CARTESIAN_POINT('Ctrl Pts',(-3.75640029658728,4.57136602935042,24.8174516619852));
#18185=CARTESIAN_POINT('Ctrl Pts',(-3.62858113832047,4.67639807468222,24.8096649183715));
#18186=CARTESIAN_POINT('Ctrl Pts',(-3.49634664295428,4.77607195449989,24.8018781747578));
#18187=CARTESIAN_POINT('Ctrl Pts',(-3.36016879150439,4.87003041623971,24.7940914311441));
#18188=CARTESIAN_POINT('Ctrl Pts',(-3.22399994720072,4.96398266333013,24.7863052025652));
#18189=CARTESIAN_POINT('Ctrl Pts',(-3.08388853186571,5.05222006744478,24.7785189739863));
#18190=CARTESIAN_POINT('Ctrl Pts',(-2.94033602984172,5.13442836098768,24.7707327454074));
#18191=CARTESIAN_POINT('Ctrl Pts',(-2.79674573813725,5.21665829556854,24.7629444671318));
#18192=CARTESIAN_POINT('Ctrl Pts',(-2.64971282616872,5.29285578753019,24.7551561888563));
#18193=CARTESIAN_POINT('Ctrl Pts',(-2.49976472370573,5.36275180188459,24.7473679105807));
#18194=CARTESIAN_POINT('Ctrl Pts',(-2.35720891753562,5.42920201039475,24.7399635868846));
#18195=CARTESIAN_POINT('Ctrl Pts',(-2.21201866798456,5.48995697688745,24.7325592631884));
#18196=CARTESIAN_POINT('Ctrl Pts',(-2.0646650507921,5.54482540667762,24.7251549394923));
#18197=CARTESIAN_POINT('Ctrl Pts',(-1.90967632516718,5.60253683699231,24.7173669617308));
#18198=CARTESIAN_POINT('Ctrl Pts',(-1.75223864807743,5.65375615905325,24.7095789839693));
#18199=CARTESIAN_POINT('Ctrl Pts',(-1.59291268300926,5.6982944594684,24.7017910062078));
#18200=CARTESIAN_POINT('Ctrl Pts',(-1.43361804279171,5.74282400327186,24.6940045596294));
#18201=CARTESIAN_POINT('Ctrl Pts',(-1.27243616291889,5.78067506036408,24.6862181130511));
#18202=CARTESIAN_POINT('Ctrl Pts',(-1.10994219897708,5.81170877431328,24.6784316664728));
#18203=CARTESIAN_POINT('Ctrl Pts',(-0.94744203625693,5.84274367212869,24.6706449228591));
#18204=CARTESIAN_POINT('Ctrl Pts',(-0.783630002435057,5.86696064257649,
24.6628581792454));
#18205=CARTESIAN_POINT('Ctrl Pts',(-0.619091500249949,5.88427194110013,
24.6550714356317));
#18206=CARTESIAN_POINT('Ctrl Pts',(-0.454563881055785,5.90158209461088,
24.6472852070528));
#18207=CARTESIAN_POINT('Ctrl Pts',(-0.289310207488934,5.9119874569139,24.6394989784739));
#18208=CARTESIAN_POINT('Ctrl Pts',(-0.123921210601472,5.91545214637589,
24.6317127498951));
#18209=CARTESIAN_POINT('Ctrl Pts',(0.041511324345274,5.91891774790493,24.6239244716195));
#18210=CARTESIAN_POINT('Ctrl Pts',(0.207078934143699,5.91543901699516,24.6161361933439));
#18211=CARTESIAN_POINT('Ctrl Pts',(0.372189759122767,5.90503220530626,24.6083479150683));
#18212=CARTESIAN_POINT('Ctrl Pts',(0.529160780268899,5.89513843935912,24.6009435913722));
#18213=CARTESIAN_POINT('Ctrl Pts',(0.685718706823125,5.87898324973805,24.593539267676));
#18214=CARTESIAN_POINT('Ctrl Pts',(0.84135836949002,5.85662416897218,24.5861349439798));
#18215=CARTESIAN_POINT('Ctrl Pts',(1.00506248095244,5.83310655535638,24.5783469662183));
#18216=CARTESIAN_POINT('Ctrl Pts',(1.16780920276732,5.80271666133896,24.5705589884567));
#18217=CARTESIAN_POINT('Ctrl Pts',(1.32901584777162,5.76555699294282,24.5627710106952));
#18218=CARTESIAN_POINT('Ctrl Pts',(1.49019079816758,5.72840463045604,24.5549845641169));
#18219=CARTESIAN_POINT('Ctrl Pts',(1.6498259647194,5.68448522105184,24.5471981175385));
#18220=CARTESIAN_POINT('Ctrl Pts',(1.80734989688456,5.63395215747626,24.5394116709602));
#18221=CARTESIAN_POINT('Ctrl Pts',(1.96487983823253,5.58341716617824,24.5316249273465));
#18222=CARTESIAN_POINT('Ctrl Pts',(2.12029807856014,5.52626810970226,24.5238381837327));
#18223=CARTESIAN_POINT('Ctrl Pts',(2.27304863594725,5.46270816181117,24.516051440119));
#18224=CARTESIAN_POINT('Ctrl Pts',(2.42578909002772,5.39915241793514,24.5082652115401));
#18225=CARTESIAN_POINT('Ctrl Pts',(2.57586191925568,5.32918675407356,24.5004789829612));
#18226=CARTESIAN_POINT('Ctrl Pts',(2.72273128855789,5.25306242993626,24.4926927543823));
#18227=CARTESIAN_POINT('Ctrl Pts',(2.869639320694,5.17691806634409,24.4849044761067));
#18228=CARTESIAN_POINT('Ctrl Pts',(3.01334192301967,5.09461194829665,24.4771161978311));
#18229=CARTESIAN_POINT('Ctrl Pts',(3.15332722404223,5.00644164857777,24.4693279195556));
#18230=CARTESIAN_POINT('Ctrl Pts',(3.28641138523839,4.922618059281,24.4619235958594));
#18231=CARTESIAN_POINT('Ctrl Pts',(3.41613571196547,4.83349469773388,24.4545192721633));
#18232=CARTESIAN_POINT('Ctrl Pts',(3.54208420636763,4.73936388532269,24.4471149484672));
#18233=CARTESIAN_POINT('Ctrl Pts',(3.67455870556014,4.64035569715858,24.4393269707057));
#18234=CARTESIAN_POINT('Ctrl Pts',(3.80290308405491,4.53577194302518,24.4315389929441));
#18235=CARTESIAN_POINT('Ctrl Pts',(3.92665481093323,4.42598153614256,24.4237510151826));
#18236=CARTESIAN_POINT('Ctrl Pts',(4.05038220716116,4.31621271499514,24.4159645686043));
#18237=CARTESIAN_POINT('Ctrl Pts',(4.16951851454271,4.20123949556612,24.408178122026));
#18238=CARTESIAN_POINT('Ctrl Pts',(4.28363542568264,4.08147009082961,24.4003916754476));
#18239=CARTESIAN_POINT('Ctrl Pts',(4.39775669012543,3.96169611716037,24.3926049318339));
#18240=CARTESIAN_POINT('Ctrl Pts',(4.50685795188849,3.83712582068368,24.3848181882202));
#18241=CARTESIAN_POINT('Ctrl Pts',(4.61054831351678,3.70820371760069,24.3770314446065));
#18242=CARTESIAN_POINT('Ctrl Pts',(4.7142318168034,3.5792901417503,24.3692452160276));
#18243=CARTESIAN_POINT('Ctrl Pts',(4.81250493594786,3.44602558440039,24.3614589874487));
#18244=CARTESIAN_POINT('Ctrl Pts',(4.90501747952483,3.30888713740071,24.3536727588699));
#18245=CARTESIAN_POINT('Ctrl Pts',(4.99755437669653,3.17171258919756,24.3458844805943));
#18246=CARTESIAN_POINT('Ctrl Pts',(5.0843274876665,3.03066237758575,24.3380962023187));
#18247=CARTESIAN_POINT('Ctrl Pts',(5.16502982950096,2.88624278654192,24.3303079240431));
#18248=CARTESIAN_POINT('Ctrl Pts',(5.24175362400793,2.7489429415293,24.322903600347));
#18249=CARTESIAN_POINT('Ctrl Pts',(5.31299066830321,2.60859815880302,24.3154992766509));
#18250=CARTESIAN_POINT('Ctrl Pts',(5.3785156424838,2.46566422005453,24.3080949529547));
#18251=CARTESIAN_POINT('Ctrl Pts',(5.44743578464466,2.31532417793549,24.3003069751932));
#18252=CARTESIAN_POINT('Ctrl Pts',(5.51006085465446,2.16206576307322,24.2925189974317));
#18253=CARTESIAN_POINT('Ctrl Pts',(5.56616133875906,2.00643427836646,24.2847310196702));
#18254=CARTESIAN_POINT('Ctrl Pts',(5.62225079302755,1.85083339214381,24.2769445730918));
#18255=CARTESIAN_POINT('Ctrl Pts',(5.67181811263725,1.69286066744404,24.2691581265135));
#18256=CARTESIAN_POINT('Ctrl Pts',(5.71468264347095,1.53307953052407,24.2613716799352));
#18257=CARTESIAN_POINT('Ctrl Pts',(5.75754880948986,1.37329229831397,24.2535849363215));
#18258=CARTESIAN_POINT('Ctrl Pts',(5.79371158846556,1.21169682344131,24.2457981927078));
#18259=CARTESIAN_POINT('Ctrl Pts',(5.82304054924039,1.04887049934782,24.2380114490941));
#18260=CARTESIAN_POINT('Ctrl Pts',(5.85236757012388,0.886054944997556,24.2302252205152));
#18261=CARTESIAN_POINT('Ctrl Pts',(5.87486162079779,0.72200901887839,24.2224389919363));
#18262=CARTESIAN_POINT('Ctrl Pts',(5.89044360274856,0.557319231086268,24.2146527633574));
#18263=CARTESIAN_POINT('Ctrl Pts',(5.9060296866001,0.392586089299144,24.2068644850818));
#18264=CARTESIAN_POINT('Ctrl Pts',(5.91470003376294,0.227209065310917,24.1990762068063));
#18265=CARTESIAN_POINT('Ctrl Pts',(5.91642745593873,0.0617796173052993,
24.1912879285307));
#18266=CARTESIAN_POINT('Ctrl Pts',(5.91806971787351,-0.0954943190601781,
24.1838836048345));
#18267=CARTESIAN_POINT('Ctrl Pts',(5.91343712095454,-0.252815371574824,
24.1764792811384));
#18268=CARTESIAN_POINT('Ctrl Pts',(5.90255000293267,-0.409675512301578,
24.1690749574422));
#18269=CARTESIAN_POINT('Ctrl Pts',(5.89109877031226,-0.574663340735441,
24.1612869796807));
#18270=CARTESIAN_POINT('Ctrl Pts',(5.87272355764134,-0.739200244435326,
24.1534990019192));
#18271=CARTESIAN_POINT('Ctrl Pts',(5.84748387136165,-0.902697588711379,
24.1457110241576));
#18272=CARTESIAN_POINT('Ctrl Pts',(5.82224914742067,-1.06616278800784,24.1379245775793));
#18273=CARTESIAN_POINT('Ctrl Pts',(5.79015269147166,-1.22858852007599,24.130138131001));
#18274=CARTESIAN_POINT('Ctrl Pts',(5.75130558359864,-1.38939362549535,24.1223516844227));
#18275=CARTESIAN_POINT('Ctrl Pts',(5.71245699379602,-1.55020486526699,24.114564940809));
#18276=CARTESIAN_POINT('Ctrl Pts',(5.66685730795468,-1.70939504314789,24.1067781971952));
#18277=CARTESIAN_POINT('Ctrl Pts',(5.61466838736882,-1.86639477667005,24.0989914535815));
#18278=CARTESIAN_POINT('Ctrl Pts',(5.56248291868962,-2.02338412583436,24.0912052250026));
#18279=CARTESIAN_POINT('Ctrl Pts',(5.50370918833982,-2.1781830173446,24.0834189964238));
#18280=CARTESIAN_POINT('Ctrl Pts',(5.43855849133229,-2.33023863560311,24.0756327678449));
#18281=CARTESIAN_POINT('Ctrl Pts',(5.37339064363782,-2.48233428195688,24.0678444895693));
#18282=CARTESIAN_POINT('Ctrl Pts',(5.30184259899911,-2.63168491734729,24.0600562112937));
#18283=CARTESIAN_POINT('Ctrl Pts',(5.22417359789647,-2.77775822949756,24.0522679330182));
#18284=CARTESIAN_POINT('Ctrl Pts',(5.15033360335965,-2.91663026876711,24.044863609322));
#18285=CARTESIAN_POINT('Ctrl Pts',(5.07096175268888,-3.05254010593703,24.0374592856259));
#18286=CARTESIAN_POINT('Ctrl Pts',(4.9863190787292,-3.18505142934948,24.0300549619297));
#18287=CARTESIAN_POINT('Ctrl Pts',(4.89729065567169,-3.32442880968005,24.0222669841682));
#18288=CARTESIAN_POINT('Ctrl Pts',(4.8023988463361,-3.4600959967259,24.0144790064067));
#18289=CARTESIAN_POINT('Ctrl Pts',(4.70197765735391,-3.59156465516697,24.0066910286451));
#18290=CARTESIAN_POINT('Ctrl Pts',(4.60157621203836,-3.72300746574274,23.9989045820668));
#18291=CARTESIAN_POINT('Ctrl Pts',(4.49564775006068,-3.85025314097573,23.9911181354884));
#18292=CARTESIAN_POINT('Ctrl Pts',(4.38456798135483,-3.97284459542254,23.9833316889101));
#18293=CARTESIAN_POINT('Ctrl Pts',(4.27348397520632,-4.09544072645685,23.9755449452964));
#18294=CARTESIAN_POINT('Ctrl Pts',(4.15724848073465,-4.21338204198094,23.9677582016827));
#18295=CARTESIAN_POINT('Ctrl Pts',(4.03627615634867,-4.32624610397874,23.9599714580689));
#18296=CARTESIAN_POINT('Ctrl Pts',(3.91531183337691,-4.43910270086322,23.9521852294901));
#18297=CARTESIAN_POINT('Ctrl Pts',(3.78961154121021,-4.54688249832685,23.9443990009112));
#18298=CARTESIAN_POINT('Ctrl Pts',(3.65962541086249,-4.64920126631119,23.9366127723323));
#18299=CARTESIAN_POINT('Ctrl Pts',(3.52960506213299,-4.75154696934357,23.9288244940567));
#18300=CARTESIAN_POINT('Ctrl Pts',(3.39529687082847,-4.8484285709596,23.9210362157811));
#18301=CARTESIAN_POINT('Ctrl Pts',(3.25718324963848,-4.9395027928704,23.9132479375055));
#18302=CARTESIAN_POINT('Ctrl Pts',(3.12587849627114,-5.02608714380615,23.9058436138094));
#18303=CARTESIAN_POINT('Ctrl Pts',(2.99113470276452,-5.10742277332757,23.8984392901133));
#18304=CARTESIAN_POINT('Ctrl Pts',(2.85338990313831,-5.18325154928529,23.8910349664172));
#18305=CARTESIAN_POINT('Ctrl Pts',(2.70850787470688,-5.26300938336715,23.8832469886557));
#18306=CARTESIAN_POINT('Ctrl Pts',(2.56025376281976,-5.33670306985653,23.8754590108942));
#18307=CARTESIAN_POINT('Ctrl Pts',(2.40915457424209,-5.40406373018568,23.8676710331327));
#18308=CARTESIAN_POINT('Ctrl Pts',(2.25808509306037,-5.4714111468315,23.8598845865543));
#18309=CARTESIAN_POINT('Ctrl Pts',(2.10417194297083,-5.53242789167951,23.852098139976));
#18310=CARTESIAN_POINT('Ctrl Pts',(1.94796378779114,-5.58689248544792,23.8443116933977));
#18311=CARTESIAN_POINT('Ctrl Pts',(1.79174967362238,-5.64135915691783,23.836524949784));
#18312=CARTESIAN_POINT('Ctrl Pts',(1.63324067959868,-5.689273068219,23.8287382061703));
#18313=CARTESIAN_POINT('Ctrl Pts',(1.47300308156508,-5.73046180374669,23.8209514625565));
#18314=CARTESIAN_POINT('Ctrl Pts',(1.31277608204974,-5.77164781494769,23.8131652339777));
#18315=CARTESIAN_POINT('Ctrl Pts',(1.15082101686754,-5.80610946107637,23.8053790053988));
#18316=CARTESIAN_POINT('Ctrl Pts',(0.987717017780421,-5.83372485255235,
23.7975927768199));
#18317=CARTESIAN_POINT('Ctrl Pts',(0.824570082151646,-5.8613475136809,23.7898044985443));
#18318=CARTESIAN_POINT('Ctrl Pts',(0.660273923203239,-5.8821202635693,23.7820162202687));
#18319=CARTESIAN_POINT('Ctrl Pts',(0.49541641361652,-5.89597262032477,23.7742279419932));
#18320=CARTESIAN_POINT('Ctrl Pts',(0.338686219659731,-5.90914206930217,
23.766823618297));
#18321=CARTESIAN_POINT('Ctrl Pts',(0.181448952454521,-5.91605700388703,
23.7594192946009));
#18322=CARTESIAN_POINT('Ctrl Pts',(0.0242127636971383,-5.91670045756705,
23.7520149709047));
#18323=CARTESIAN_POINT('Ctrl Pts',(-0.141170597647017,-5.91737725171548,
23.7442269931432));
#18324=CARTESIAN_POINT('Ctrl Pts',(-0.30661192664777,-5.91111564023968,
23.7364390153817));
#18325=CARTESIAN_POINT('Ctrl Pts',(-0.471519809903724,-5.89793180965738,
23.7286510376201));
#18326=CARTESIAN_POINT('Ctrl Pts',(-0.636395270856173,-5.88475057112919,
23.7208645910418));
#18327=CARTESIAN_POINT('Ctrl Pts',(-0.800737176992085,-5.86464985447569,
23.7130781444635));
#18328=CARTESIAN_POINT('Ctrl Pts',(-0.963957788586457,-5.83769782913808,
23.7052916978851));
#18329=CARTESIAN_POINT('Ctrl Pts',(-1.12718462667905,-5.81074477564149,
23.6975049542714));
#18330=CARTESIAN_POINT('Ctrl Pts',(-1.28928976872298,-5.77693993862877,
23.6897182106577));
#18331=CARTESIAN_POINT('Ctrl Pts',(-1.44969349687653,-5.73640299557256,
23.681931467044));
#18332=CARTESIAN_POINT('Ctrl Pts',(-1.61008661552351,-5.69586873373187,
23.6741452384651));
#18333=CARTESIAN_POINT('Ctrl Pts',(-1.76877823567306,-5.64860333532758,
23.6663590098862));
#18334=CARTESIAN_POINT('Ctrl Pts',(-1.92520153719232,-5.59477699320467,
23.6585727813074));
#18335=CARTESIAN_POINT('Ctrl Pts',(-2.08166601658374,-5.54093648149058,
23.6507845030318));
#18336=CARTESIAN_POINT('Ctrl Pts',(-2.235860681161,-5.48053167705407,23.6429962247562));
#18337=CARTESIAN_POINT('Ctrl Pts',(-2.38723564347627,-5.41378209249472,
23.6352079464806));
#18338=CARTESIAN_POINT('Ctrl Pts',(-2.5311479666905,-5.35032319783607,23.6278036227845));
#18339=CARTESIAN_POINT('Ctrl Pts',(-2.6725116666884,-5.28113014297149,23.6203992990883));
#18340=CARTESIAN_POINT('Ctrl Pts',(-2.81087246682014,-5.20643126697861,
23.6129949753921));
#18341=CARTESIAN_POINT('Ctrl Pts',(-2.95640241374202,-5.12786187848116,
23.6052069976306));
#18342=CARTESIAN_POINT('Ctrl Pts',(-3.09866206799006,-5.04317284794488,
23.597419019869));
#18343=CARTESIAN_POINT('Ctrl Pts',(-3.2371399187134,-4.9526614773445,23.5896310421075));
#18344=CARTESIAN_POINT('Ctrl Pts',(-3.37559054350388,-4.86216790205569,
23.5818445955292));
#18345=CARTESIAN_POINT('Ctrl Pts',(-3.51026058102323,-4.76585444548336,
23.5740581489508));
#18346=CARTESIAN_POINT('Ctrl Pts',(-3.64066662842203,-4.66406229195046,
23.5662717023725));
#18347=CARTESIAN_POINT('Ctrl Pts',(-3.77107765051768,-4.56226625527628,
23.5584849587588));
#18348=CARTESIAN_POINT('Ctrl Pts',(-3.8972241026844,-4.45499129692908,23.5506982151451));
#18349=CARTESIAN_POINT('Ctrl Pts',(-4.01865428046869,-4.342619985282,23.5429114715314));
#18350=CARTESIAN_POINT('Ctrl Pts',(-4.14007642655515,-4.23025610615654,
23.5351252429525));
#18351=CARTESIAN_POINT('Ctrl Pts',(-4.25678268803283,-4.11279676542965,
23.5273390143736));
#18352=CARTESIAN_POINT('Ctrl Pts',(-4.36835686464773,-3.99066271007524,
23.5195527857947));
#18353=CARTESIAN_POINT('Ctrl Pts',(-4.4799604127638,-3.86849650336952,23.5117645075191));
#18354=CARTESIAN_POINT('Ctrl Pts',(-4.5864289593144,-3.74165335779748,23.5039762292435));
#18355=CARTESIAN_POINT('Ctrl Pts',(-4.68738477863621,-3.61058921777452,
23.4961879509679));
#18356=CARTESIAN_POINT('Ctrl Pts',(-4.78336357379655,-3.48598641297699,
23.4887836272718));
#18357=CARTESIAN_POINT('Ctrl Pts',(-4.87435993194359,-3.3575689791053,23.4813793035757));
#18358=CARTESIAN_POINT('Ctrl Pts',(-4.96008429829237,-3.22575484442533,
23.4739749798796));
#18359=CARTESIAN_POINT('Ctrl Pts',(-5.05025046148925,-3.08711077756978,
23.4661870021181));
#18360=CARTESIAN_POINT('Ctrl Pts',(-5.13461604696483,-2.94465906958686,
23.4583990243566));
#18361=CARTESIAN_POINT('Ctrl Pts',(-5.21287425880004,-2.79890559405636,
23.450611046595));
#18362=CARTESIAN_POINT('Ctrl Pts',(-5.29111708439974,-2.65318077490898,
23.4428246000167));
#18363=CARTESIAN_POINT('Ctrl Pts',(-5.36325478116319,-2.50415576483357,
23.4350381534384));
#18364=CARTESIAN_POINT('Ctrl Pts',(-5.42902623694026,-2.35236151156965,
23.4272517068601));
#18365=CARTESIAN_POINT('Ctrl Pts',(-5.49480020175021,-2.20056146769693,
23.4194649632464));
#18366=CARTESIAN_POINT('Ctrl Pts',(-5.55420730894161,-2.04599226087433,
23.4116782196326));
#18367=CARTESIAN_POINT('Ctrl Pts',(-5.60703408663292,-1.88920600089999,
23.4038914760189));
#18368=CARTESIAN_POINT('Ctrl Pts',(-5.65985737022805,-1.73243011116394,
23.39610524744));
#18369=CARTESIAN_POINT('Ctrl Pts',(-5.70610109336985,-1.57343776461223,
23.3883190188612));
#18370=CARTESIAN_POINT('Ctrl Pts',(-5.74560123158306,-1.41279759701494,
23.3805327902823));
#18371=CARTESIAN_POINT('Ctrl Pts',(-5.78511176806576,-1.25211514147062,
23.3727445120067));
#18372=CARTESIAN_POINT('Ctrl Pts',(-5.81787509409511,-1.08978430813744,
23.3649562337311));
#18373=CARTESIAN_POINT('Ctrl Pts',(-5.84377781361127,-0.926386219481219,
23.3571679554556));
#18374=CARTESIAN_POINT('Ctrl Pts',(-5.86840355413074,-0.771043498416085,
23.3497636317594));
#18375=CARTESIAN_POINT('Ctrl Pts',(-5.88682879483896,-0.614736476746315,
23.3423593080633));
#18376=CARTESIAN_POINT('Ctrl Pts',(-5.89899935629682,-0.457970694378671,
23.3349549843671));
#18377=CARTESIAN_POINT('Ctrl Pts',(-5.9108229968946,-0.305673507830525,
23.3277617203131));
#18378=CARTESIAN_POINT('Ctrl Pts',(-5.91674658177293,-0.152915681688521,
23.320568456259));
#18379=CARTESIAN_POINT('Ctrl Pts',(-5.91674999852046,-0.000132318339550427,
23.3133751922049));
#18380=CARTESIAN_POINT('Ctrl Pts',(-5.91724902186819,-2.6012278470935E-5,
23.0616248077951));
#18381=CARTESIAN_POINT('Ctrl Pts',(-5.91725507970182,-0.0246275738384623,
23.0627831909737));
#18382=CARTESIAN_POINT('Ctrl Pts',(-5.91710486183363,-0.0492290611478781,
23.0639415741523));
#18383=CARTESIAN_POINT('Ctrl Pts',(-5.90452526107738,-1.05738799629361,
23.1114154190926));
#18384=CARTESIAN_POINT('Ctrl Pts',(-5.37887374875949,-3.01825410262035,
23.204046342616));
#18385=CARTESIAN_POINT('Ctrl Pts',(-3.27927262205552,-5.2238407042437,23.3429927279011));
#18386=CARTESIAN_POINT('Ctrl Pts',(-0.380334538725489,-6.15609342616977,
23.4819391131863));
#18387=CARTESIAN_POINT('Ctrl Pts',(2.61131174173346,-5.58777161492509,23.6208854984714));
#18388=CARTESIAN_POINT('Ctrl Pts',(4.96643943377135,-3.65740618249594,23.7598318837565));
#18389=CARTESIAN_POINT('Ctrl Pts',(6.11097592471195,-0.83553209433702,23.8987782690417));
#18390=CARTESIAN_POINT('Ctrl Pts',(5.76593546958871,2.19000657387534,24.0377246543268));
#18391=CARTESIAN_POINT('Ctrl Pts',(4.01542317922815,4.68172161974577,24.1766710396119));
#18392=CARTESIAN_POINT('Ctrl Pts',(1.28613403388383,6.03224666935662,24.315617424897));
#18393=CARTESIAN_POINT('Ctrl Pts',(-1.75665587304459,5.91238537113191,24.4545638101821));
#18394=CARTESIAN_POINT('Ctrl Pts',(-4.37125327473482,4.35135443755144,24.5935101954673));
#18395=CARTESIAN_POINT('Ctrl Pts',(-5.69818711861276,2.10563417864119,24.7125305280049));
#18396=CARTESIAN_POINT('Ctrl Pts',(-5.9160758600808,0.560655488508289,24.7852353987809));
#18397=CARTESIAN_POINT('Ctrl Pts',(-5.91628298387923,-6.23028472571992E-5,
24.8116248077951));
#18398=CARTESIAN_POINT('Origin',(0.,0.,0.));
#18399=CARTESIAN_POINT('',(-5.91679775669098,2.19428441319584E-5,26.8133751922049));
#18400=CARTESIAN_POINT('',(-5.91695430380796,0.0001364654751753,26.5616248077951));
#18401=CARTESIAN_POINT('',(-5.91675,-7.2459289488551E-16,0.));
#18402=CARTESIAN_POINT('Ctrl Pts',(-5.91725285177388,2.19445318853841E-5,
26.8133751922049));
#18403=CARTESIAN_POINT('Ctrl Pts',(-5.91725718695043,0.020695672166474,
26.8124017521966));
#18404=CARTESIAN_POINT('Ctrl Pts',(-5.9171511099118,0.0413693551410023,
26.8114283121884));
#18405=CARTESIAN_POINT('Ctrl Pts',(-5.90661556573244,1.04614428635966,26.7641148736759));
#18406=CARTESIAN_POINT('Ctrl Pts',(-5.38431816636206,3.00908896148112,26.6714348766675));
#18407=CARTESIAN_POINT('Ctrl Pts',(-3.28705913345889,5.21926630359759,26.532414881155));
#18408=CARTESIAN_POINT('Ctrl Pts',(-0.387733679065683,6.15590457112853,
26.3933948856425));
#18409=CARTESIAN_POINT('Ctrl Pts',(2.60620162316863,5.59045719008011,26.25437489013));
#18410=CARTESIAN_POINT('Ctrl Pts',(4.96420470614338,3.66089744874507,26.1153548946175));
#18411=CARTESIAN_POINT('Ctrl Pts',(6.110905606059,0.838052008266846,25.976334899105));
#18412=CARTESIAN_POINT('Ctrl Pts',(5.7665009333289,-2.18928423934433,25.8373149035924));
#18413=CARTESIAN_POINT('Ctrl Pts',(4.01502794197995,-4.68241915251552,25.69829490808));
#18414=CARTESIAN_POINT('Ctrl Pts',(1.28385882626606,-6.03300961452435,25.5592749125674));
#18415=CARTESIAN_POINT('Ctrl Pts',(-1.76058121420839,-5.91150169440051,
25.4202549170549));
#18416=CARTESIAN_POINT('Ctrl Pts',(-4.37542658756877,-4.34754421156596,
25.2812349215424));
#18417=CARTESIAN_POINT('Ctrl Pts',(-5.69937917119131,-2.10150200017265,
25.162275013259));
#18418=CARTESIAN_POINT('Ctrl Pts',(-5.91608000283946,-0.558332029564552,
25.0896551034799));
#18419=CARTESIAN_POINT('Ctrl Pts',(-5.91627901576061,6.02123609064198E-5,
25.0633751922049));
#18420=CARTESIAN_POINT('Ctrl Pts',(-5.91628298387923,-6.23028472571992E-5,
24.8116248077951));
#18421=CARTESIAN_POINT('Ctrl Pts',(-5.91643937842867,-0.423447770894904,
24.8315508605426));
#18422=CARTESIAN_POINT('Ctrl Pts',(-5.76745479447041,-1.83082804996811,
24.8977923750519));
#18423=CARTESIAN_POINT('Ctrl Pts',(-4.66335225933688,-4.03674204506728,
25.0103493513227));
#18424=CARTESIAN_POINT('Ctrl Pts',(-2.16367632199188,-5.77586750252553,
25.1492957366078));
#18425=CARTESIAN_POINT('Ctrl Pts',(0.863405124340446,-6.10710014854341,
25.2882421218929));
#18426=CARTESIAN_POINT('Ctrl Pts',(3.68002781839282,-4.94970058578635,25.427188507178));
#18427=CARTESIAN_POINT('Ctrl Pts',(5.59962773462851,-2.58578998889243,25.5661348924632));
#18428=CARTESIAN_POINT('Ctrl Pts',(6.15429404896376,0.40841815822461,25.7050812777483));
#18429=CARTESIAN_POINT('Ctrl Pts',(5.20882443614428,3.30307260388006,25.8440276630334));
#18430=CARTESIAN_POINT('Ctrl Pts',(2.99368122425189,5.39258874388175,25.9829740483185));
#18431=CARTESIAN_POINT('Ctrl Pts',(0.0488152004140352,6.16763793597564,
26.1219204336038));
#18432=CARTESIAN_POINT('Ctrl Pts',(-2.90794974072443,5.43929857044995,26.2608668188888));
#18433=CARTESIAN_POINT('Ctrl Pts',(-5.15588929170198,3.38510653374309,26.3998132041739));
#18434=CARTESIAN_POINT('Ctrl Pts',(-5.87103811602415,1.30761350995423,26.5000658671427));
#18435=CARTESIAN_POINT('Ctrl Pts',(-5.91711432678824,0.162029141072471,
26.5540030683498));
#18436=CARTESIAN_POINT('Ctrl Pts',(-5.91695430380796,0.0001364654751753,
26.5616248077951));
#18437=CARTESIAN_POINT('Origin',(0.,0.,0.));
#18438=CARTESIAN_POINT('',(-5.91674757964165,-9.37334433651367E-5,28.5633751922614));
#18439=CARTESIAN_POINT('',(-5.91674999800012,-0.00015383611583252,28.3116248078268));
#18440=CARTESIAN_POINT('',(-5.91675,-7.2459289488551E-16,0.));
#18441=CARTESIAN_POINT('Ctrl Pts',(-5.91674999925755,-9.3732281115321E-5,
28.5633751922049));
#18442=CARTESIAN_POINT('Ctrl Pts',(-5.91675262882337,0.165894797763913,
28.5555635075889));
#18443=CARTESIAN_POINT('Ctrl Pts',(-5.90976595002247,0.331883858816857,
28.5477518229729));
#18444=CARTESIAN_POINT('Ctrl Pts',(-5.89581587907907,0.497278274710596,
28.5399401383569));
#18445=CARTESIAN_POINT('Ctrl Pts',(-5.88186591041835,0.662671477923394,
28.5321285110166));
#18446=CARTESIAN_POINT('Ctrl Pts',(-5.86095268125918,0.827469730883103,
28.5243168836763));
#18447=CARTESIAN_POINT('Ctrl Pts',(-5.83315402760025,0.991082566081681,
28.516505256336));
#18448=CARTESIAN_POINT('Ctrl Pts',(-5.80534823376329,1.15473742578916,28.5086916225529));
#18449=CARTESIAN_POINT('Ctrl Pts',(-5.77065353462187,1.31720594854534,28.5008779887697));
#18450=CARTESIAN_POINT('Ctrl Pts',(-5.72919912930452,1.47790659355603,28.4930643549866));
#18451=CARTESIAN_POINT('Ctrl Pts',(-5.70378711174193,1.57641789970232,28.4882745094345));
#18452=CARTESIAN_POINT('Ctrl Pts',(-5.67583591392416,1.67426507088607,28.4834846638823));
#18453=CARTESIAN_POINT('Ctrl Pts',(-5.64538465570273,1.77131664353277,28.4786948183302));
#18454=CARTESIAN_POINT('Ctrl Pts',(-5.59587288768143,1.92911619703704,28.4709068405688));
#18455=CARTESIAN_POINT('Ctrl Pts',(-5.53973191207739,2.08486674110341,28.4631188628075));
#18456=CARTESIAN_POINT('Ctrl Pts',(-5.47715651414356,2.23800962510771,28.4553308850461));
#18457=CARTESIAN_POINT('Ctrl Pts',(-5.41459341906945,2.39112239990808,28.4475444384679));
#18458=CARTESIAN_POINT('Ctrl Pts',(-5.34559854663349,2.54162824198346,28.4397579918897));
#18459=CARTESIAN_POINT('Ctrl Pts',(-5.27041510263627,2.68898776650314,28.4319715453116));
#18460=CARTESIAN_POINT('Ctrl Pts',(-5.19522879056015,2.83635291245648,28.424184801698));
#18461=CARTESIAN_POINT('Ctrl Pts',(-5.11385357622112,2.98057121425195,28.4163980580844));
#18462=CARTESIAN_POINT('Ctrl Pts',(-5.02657931473763,3.12112655224869,28.4086113144709));
#18463=CARTESIAN_POINT('Ctrl Pts',(-4.93931082579369,3.26167259356124,28.4008250858922));
#18464=CARTESIAN_POINT('Ctrl Pts',(-4.8461442391848,3.39855588447202,28.3930388573135));
#18465=CARTESIAN_POINT('Ctrl Pts',(-4.7474136347221,3.53128791566968,28.3852526287347));
#18466=CARTESIAN_POINT('Ctrl Pts',(-4.64865703978238,3.66405488809782,28.3774643504593));
#18467=CARTESIAN_POINT('Ctrl Pts',(-4.5443336894687,3.79266815942464,28.3696760721839));
#18468=CARTESIAN_POINT('Ctrl Pts',(-4.43481952526852,3.91667031300786,28.3618877939085));
#18469=CARTESIAN_POINT('Ctrl Pts',(-4.33070430333401,4.0345592804758,28.3544834702116));
#18470=CARTESIAN_POINT('Ctrl Pts',(-4.22189791747622,4.14828062816423,28.3470791465147));
#18471=CARTESIAN_POINT('Ctrl Pts',(-4.10875572356729,4.25747072409817,28.3396748228178));
#18472=CARTESIAN_POINT('Ctrl Pts',(-3.98975108166709,4.37231849058331,28.3318868450562));
#18473=CARTESIAN_POINT('Ctrl Pts',(-3.86590681357093,4.48219404919458,28.3240988672946));
#18474=CARTESIAN_POINT('Ctrl Pts',(-3.73766134782034,4.58670014405889,28.316310889533));
#18475=CARTESIAN_POINT('Ctrl Pts',(-3.60944109622796,4.69118569212886,28.3085244429546));
#18476=CARTESIAN_POINT('Ctrl Pts',(-3.47682162110087,4.79030368111094,28.3007379963762));
#18477=CARTESIAN_POINT('Ctrl Pts',(-3.34027464213883,4.88369694776246,28.2929515497978));
#18478=CARTESIAN_POINT('Ctrl Pts',(-3.20372245421738,4.97709377715655,28.285164806184));
#18479=CARTESIAN_POINT('Ctrl Pts',(-3.06324272417338,5.06476526356921,28.2773780625702));
#18480=CARTESIAN_POINT('Ctrl Pts',(-2.91933699335127,5.14639700001377,28.2695913189564));
#18481=CARTESIAN_POINT('Ctrl Pts',(-2.77544078081694,5.22802333712952,28.2618050903775));
#18482=CARTESIAN_POINT('Ctrl Pts',(-2.62811929899789,5.30361056612377,28.2540188617986));
#18483=CARTESIAN_POINT('Ctrl Pts',(-2.4778997021947,5.37288969069377,28.2462326332197));
#18484=CARTESIAN_POINT('Ctrl Pts',(-2.32764056062208,5.44218705274454,28.238444354944));
#18485=CARTESIAN_POINT('Ctrl Pts',(-2.17448206914537,5.50517285647967,28.2306560766684));
#18486=CARTESIAN_POINT('Ctrl Pts',(-2.01897325341945,5.56162544266304,28.2228677983927));
#18487=CARTESIAN_POINT('Ctrl Pts',(-1.87113087177371,5.61529497099461,28.2154634746969));
#18488=CARTESIAN_POINT('Ctrl Pts',(-1.72116456873923,5.66305983748205,28.2080591510011));
#18489=CARTESIAN_POINT('Ctrl Pts',(-1.56956040421967,5.7047708718235,28.2006548273052));
#18490=CARTESIAN_POINT('Ctrl Pts',(-1.41010088970494,5.74864315796466,28.1928668495436));
#18491=CARTESIAN_POINT('Ctrl Pts',(-1.24877223449866,5.78583329281053,28.185078871782));
#18492=CARTESIAN_POINT('Ctrl Pts',(-1.08614953066657,5.81620234857186,28.1772908940204));
#18493=CARTESIAN_POINT('Ctrl Pts',(-0.923558799852407,5.84656543351644,
28.1695044474419));
#18494=CARTESIAN_POINT('Ctrl Pts',(-0.759674841984277,5.87011005660676,
28.1617180008635));
#18495=CARTESIAN_POINT('Ctrl Pts',(-0.595082787611209,5.88674842662644,
28.1539315542851));
#18496=CARTESIAN_POINT('Ctrl Pts',(-0.430484454422606,5.9033874313624,28.1461448106713));
#18497=CARTESIAN_POINT('Ctrl Pts',(-0.265178288197985,5.91311961977152,
28.1383580670575));
#18498=CARTESIAN_POINT('Ctrl Pts',(-0.0997551367588218,5.91590901512103,
28.1305713234437));
#18499=CARTESIAN_POINT('Ctrl Pts',(0.0656570731764681,5.9186982259729,28.1227850948648));
#18500=CARTESIAN_POINT('Ctrl Pts',(0.231185933308759,5.91454555744609,28.1149988662858));
#18501=CARTESIAN_POINT('Ctrl Pts',(0.396239844345193,5.90346716330779,28.1072126377069));
#18502=CARTESIAN_POINT('Ctrl Pts',(0.561337205230819,5.89238585282202,28.0994243594312));
#18503=CARTESIAN_POINT('Ctrl Pts',(0.72595904801083,5.87437519310494,28.0916360811556));
#18504=CARTESIAN_POINT('Ctrl Pts',(0.889517229130205,5.84950336879812,28.0838478028799));
#18505=CARTESIAN_POINT('Ctrl Pts',(1.04501215024488,5.82585770135368,28.0764434791842));
#18506=CARTESIAN_POINT('Ctrl Pts',(1.19954549789333,5.79601111058879,28.0690391554884));
#18507=CARTESIAN_POINT('Ctrl Pts',(1.35261911030467,5.76006528651704,28.0616348317927));
#18508=CARTESIAN_POINT('Ctrl Pts',(1.51362421195892,5.72225693426383,28.0538468540313));
#18509=CARTESIAN_POINT('Ctrl Pts',(1.67307188482846,5.67768698098481,28.0460588762699));
#18510=CARTESIAN_POINT('Ctrl Pts',(1.83039069998508,5.62650872636915,28.0382708985086));
#18511=CARTESIAN_POINT('Ctrl Pts',(1.98767858491353,5.57534053383723,28.0304844519304));
#18512=CARTESIAN_POINT('Ctrl Pts',(2.14283814357463,5.51756673114694,28.0226980053522));
#18513=CARTESIAN_POINT('Ctrl Pts',(2.29531361069508,5.45339032080576,28.0149115587741));
#18514=CARTESIAN_POINT('Ctrl Pts',(2.44779489441133,5.389211462279,28.0071248151605));
#18515=CARTESIAN_POINT('Ctrl Pts',(2.59759158564982,5.31862962767838,27.9993380715469));
#18516=CARTESIAN_POINT('Ctrl Pts',(2.74416770129323,5.24189604911038,27.9915513279334));
#18517=CARTESIAN_POINT('Ctrl Pts',(2.89073412202315,5.16516754589455,27.9837650993546));
#18518=CARTESIAN_POINT('Ctrl Pts',(3.03408011036302,5.08228826128183,27.9759788707759));
#18519=CARTESIAN_POINT('Ctrl Pts',(3.17369397657337,4.99355555747224,27.9681926421971));
#18520=CARTESIAN_POINT('Ctrl Pts',(3.31334459563241,4.90479949509717,27.9604043639217));
#18521=CARTESIAN_POINT('Ctrl Pts',(3.44926085846503,4.81018710436662,27.9526160856463));
#18522=CARTESIAN_POINT('Ctrl Pts',(3.58095901493649,4.71005977624967,27.9448278073708));
#18523=CARTESIAN_POINT('Ctrl Pts',(3.70616457980042,4.61486862846837,27.937423483674));
#18524=CARTESIAN_POINT('Ctrl Pts',(3.8275577072866,4.51469336644065,27.9300191599771));
#18525=CARTESIAN_POINT('Ctrl Pts',(3.94474968886493,4.4098617273901,27.9226148362803));
#18526=CARTESIAN_POINT('Ctrl Pts',(4.06801395765482,4.2995982506609,27.9148268585186));
#18527=CARTESIAN_POINT('Ctrl Pts',(4.18667425217489,4.18414360317922,27.907038880757));
#18528=CARTESIAN_POINT('Ctrl Pts',(4.30030223946391,4.06390590586959,27.8992509029953));
#18529=CARTESIAN_POINT('Ctrl Pts',(4.41390788651618,3.94369184832238,27.8914644564169));
#18530=CARTESIAN_POINT('Ctrl Pts',(4.52248298112377,3.8186968494063,27.8836780098385));
#18531=CARTESIAN_POINT('Ctrl Pts',(4.62563673407239,3.68936517125916,27.87589156326));
#18532=CARTESIAN_POINT('Ctrl Pts',(4.72879442210443,3.56002855939969,27.8681048196462));
#18533=CARTESIAN_POINT('Ctrl Pts',(4.82653015230451,3.42635518461736,27.8603180760324));
#18534=CARTESIAN_POINT('Ctrl Pts',(4.91849359005227,3.28882218539019,27.8525313324185));
#18535=CARTESIAN_POINT('Ctrl Pts',(5.01045094510655,3.15129828294213,27.8447451038395));
#18536=CARTESIAN_POINT('Ctrl Pts',(5.09663659419305,3.00991553263504,27.8369588752605));
#18537=CARTESIAN_POINT('Ctrl Pts',(5.17674361315702,2.86517994655449,27.8291726466816));
#18538=CARTESIAN_POINT('Ctrl Pts',(5.25687172000597,2.72040625935084,27.8213843684059));
#18539=CARTESIAN_POINT('Ctrl Pts',(5.33091784268429,2.57227825153229,27.8135960901302));
#18540=CARTESIAN_POINT('Ctrl Pts',(5.39862066304133,2.42132721850707,27.8058078118545));
#18541=CARTESIAN_POINT('Ctrl Pts',(5.46298579988965,2.27781792529263,27.7984034881589));
#18542=CARTESIAN_POINT('Ctrl Pts',(5.52161789799881,2.13175748716479,27.7909991644633));
#18543=CARTESIAN_POINT('Ctrl Pts',(5.57433254979846,1.98361971828206,27.7835948407677));
#18544=CARTESIAN_POINT('Ctrl Pts',(5.6297786044005,1.82780621024045,27.7758068630063));
#18545=CARTESIAN_POINT('Ctrl Pts',(5.67869754257536,1.66963864527529,27.7680188852448));
#18546=CARTESIAN_POINT('Ctrl Pts',(5.72090864369786,1.50968038106187,27.7602309074834));
#18547=CARTESIAN_POINT('Ctrl Pts',(5.76311144575601,1.34975356601448,27.7524444609052));
#18548=CARTESIAN_POINT('Ctrl Pts',(5.79860896070824,1.1880370629793,27.7446580143269));
#18549=CARTESIAN_POINT('Ctrl Pts',(5.82727073082005,1.02510799052,27.7368715677487));
#18550=CARTESIAN_POINT('Ctrl Pts',(5.85593359431377,0.86217270268391,27.7290848241351));
#18551=CARTESIAN_POINT('Ctrl Pts',(5.87776013190894,0.698025066884494,27.7212980805215));
#18552=CARTESIAN_POINT('Ctrl Pts',(5.89267114168673,0.533251702699923,27.7135113369078));
#18553=CARTESIAN_POINT('Ctrl Pts',(5.9075811652128,0.368489237040522,27.705725108329));
#18554=CARTESIAN_POINT('Ctrl Pts',(5.915576547579,0.203101444104479,27.6979388797502));
#18555=CARTESIAN_POINT('Ctrl Pts',(5.91663002194938,0.0376795152204819,
27.6901526511714));
#18556=CARTESIAN_POINT('Ctrl Pts',(5.91768377364311,-0.127785960391721,
27.682364372896));
#18557=CARTESIAN_POINT('Ctrl Pts',(5.91179196175398,-0.293285270164019,
27.6745760946205));
#18558=CARTESIAN_POINT('Ctrl Pts',(5.89897946365164,-0.45822685420669,27.666787816345));
#18559=CARTESIAN_POINT('Ctrl Pts',(5.88679860930157,-0.615036977841214,
27.6593834926484));
#18560=CARTESIAN_POINT('Ctrl Pts',(5.868363018147,-0.771342779077537,27.6519791689518));
#18561=CARTESIAN_POINT('Ctrl Pts',(5.84373758037036,-0.926639980934974,
27.6445748452553));
#18562=CARTESIAN_POINT('Ctrl Pts',(5.81783617875235,-1.0899838870189,27.6367868674936));
#18563=CARTESIAN_POINT('Ctrl Pts',(5.78507718260018,-1.25227032912556,27.628998889732));
#18564=CARTESIAN_POINT('Ctrl Pts',(5.74557158077637,-1.41291817621364,27.6212109119704));
#18565=CARTESIAN_POINT('Ctrl Pts',(5.70607374609244,-1.57353443855826,27.6134244653919));
#18566=CARTESIAN_POINT('Ctrl Pts',(5.65983202863783,-1.73251243857735,27.6056380188135));
#18567=CARTESIAN_POINT('Ctrl Pts',(5.60700813479728,-1.88928302242335,27.597851572235));
#18568=CARTESIAN_POINT('Ctrl Pts',(5.55418222584456,-2.04605958671284,27.5900648286212));
#18569=CARTESIAN_POINT('Ctrl Pts',(5.49477373634509,-2.20062826225394,27.5822780850074));
#18570=CARTESIAN_POINT('Ctrl Pts',(5.42899392292789,-2.35243608782727,27.5744913413936));
#18571=CARTESIAN_POINT('Ctrl Pts',(5.36321846035328,-2.50423387244855,27.5667051128146));
#18572=CARTESIAN_POINT('Ctrl Pts',(5.29107264434056,-2.65327087934423,27.5589188842357));
#18573=CARTESIAN_POINT('Ctrl Pts',(5.21281551867958,-2.79901499294187,27.5511326556567));
#18574=CARTESIAN_POINT('Ctrl Pts',(5.13453779211136,-2.94479747315392,27.5433443773811));
#18575=CARTESIAN_POINT('Ctrl Pts',(5.05014569075875,-3.08728504528919,27.5355560991054));
#18576=CARTESIAN_POINT('Ctrl Pts',(4.95994421725192,-3.22597022990746,27.5277678208298));
#18577=CARTESIAN_POINT('Ctrl Pts',(4.87418958907396,-3.35781836917131,27.520363497134));
#18578=CARTESIAN_POINT('Ctrl Pts',(4.78318472746382,-3.48622977707173,27.5129591734383));
#18579=CARTESIAN_POINT('Ctrl Pts',(4.68722798667849,-3.61079276107033,27.5055548497426));
#18580=CARTESIAN_POINT('Ctrl Pts',(4.58629925989531,-3.7418099598247,27.4977668719811));
#18581=CARTESIAN_POINT('Ctrl Pts',(4.47985576359286,-3.86861620263012,27.4899788942196));
#18582=CARTESIAN_POINT('Ctrl Pts',(4.36827311402875,-3.99075438529528,27.4821909164581));
#18583=CARTESIAN_POINT('Ctrl Pts',(4.25671240257029,-4.11286855454648,27.4744044698799));
#18584=CARTESIAN_POINT('Ctrl Pts',(4.14001476929804,-4.23031625912445,27.4666180233016));
#18585=CARTESIAN_POINT('Ctrl Pts',(4.01859462717775,-4.34267518759096,27.4588315767233));
#18586=CARTESIAN_POINT('Ctrl Pts',(3.89716985315276,-4.45503840229727,27.4510448331097));
#18587=CARTESIAN_POINT('Ctrl Pts',(3.77102244163432,-4.56231223251412,27.443258089496));
#18588=CARTESIAN_POINT('Ctrl Pts',(3.64060255963977,-4.66411230195461,27.4354713458823));
#18589=CARTESIAN_POINT('Ctrl Pts',(3.51019130394476,-4.76590563808207,27.4276851173035));
#18590=CARTESIAN_POINT('Ctrl Pts',(3.37550839527123,-4.86222574139844,27.4198988887247));
#18591=CARTESIAN_POINT('Ctrl Pts',(3.23703597945929,-4.95272941217124,27.4121126601459));
#18592=CARTESIAN_POINT('Ctrl Pts',(3.09852711128112,-5.04325690771038,27.4043243818703));
#18593=CARTESIAN_POINT('Ctrl Pts',(2.95622700919494,-5.12796473455706,27.3965361035948));
#18594=CARTESIAN_POINT('Ctrl Pts',(2.81064637822338,-5.20655332240819,27.3887478253193));
#18595=CARTESIAN_POINT('Ctrl Pts',(2.67224273142234,-5.28126756895975,27.3813435016229));
#18596=CARTESIAN_POINT('Ctrl Pts',(2.53087444983944,-5.35045126271971,27.3739391779265));
#18597=CARTESIAN_POINT('Ctrl Pts',(2.38700055118997,-5.41388575157611,27.3665348542302));
#18598=CARTESIAN_POINT('Ctrl Pts',(2.23567184527486,-5.48060709018675,27.3587468764686));
#18599=CARTESIAN_POINT('Ctrl Pts',(2.08151683887124,-5.54099148486481,27.3509588987071));
#18600=CARTESIAN_POINT('Ctrl Pts',(1.92508412252328,-5.59481739502808,27.3431709209456));
#18601=CARTESIAN_POINT('Ctrl Pts',(1.76868216218759,-5.64863272255625,27.3353844743672));
#18602=CARTESIAN_POINT('Ctrl Pts',(1.61000368741266,-5.69589203450496,27.3275980277888));
#18603=CARTESIAN_POINT('Ctrl Pts',(1.44961469795676,-5.73642290891874,27.3198115812104));
#18604=CARTESIAN_POINT('Ctrl Pts',(1.28921959002358,-5.77695532949373,27.3120248375967));
#18605=CARTESIAN_POINT('Ctrl Pts',(1.12711414566991,-5.81075871680186,27.304238093983));
#18606=CARTESIAN_POINT('Ctrl Pts',(0.963877598263364,-5.83771107010839,
27.2964513503692));
#18607=CARTESIAN_POINT('Ctrl Pts',(0.800651847733722,-5.86466164071831,
27.2886651217904));
#18608=CARTESIAN_POINT('Ctrl Pts',(0.636295459191402,-5.88476203218761,
27.2808788932115));
#18609=CARTESIAN_POINT('Ctrl Pts',(0.471396033422478,-5.89794170386361,
27.2730926646327));
#18610=CARTESIAN_POINT('Ctrl Pts',(0.306453198471773,-5.91112484504086,
27.2653043863571));
#18611=CARTESIAN_POINT('Ctrl Pts',(0.140967359235795,-5.91738359854969,
27.2575161080815));
#18612=CARTESIAN_POINT('Ctrl Pts',(-0.0244696926235903,-5.91669940056472,
27.249727829806));
#18613=CARTESIAN_POINT('Ctrl Pts',(-0.181750857979391,-5.91604893287806,
27.2423235061098));
#18614=CARTESIAN_POINT('Ctrl Pts',(-0.338987666939524,-5.90912358622243,
27.2349191824137));
#18615=CARTESIAN_POINT('Ctrl Pts',(-0.495672442003575,-5.89595110162374,
27.2275148587176));
#18616=CARTESIAN_POINT('Ctrl Pts',(-0.660475818227291,-5.88209608645566,
27.2197268809561));
#18617=CARTESIAN_POINT('Ctrl Pts',(-0.82472738795972,-5.86132439994564,
27.2119389031945));
#18618=CARTESIAN_POINT('Ctrl Pts',(-0.987839446467213,-5.83370412263969,
27.204150925433));
#18619=CARTESIAN_POINT('Ctrl Pts',(-1.1509194357451,-5.80608927571714,27.1963644788546));
#18620=CARTESIAN_POINT('Ctrl Pts',(-1.31286004594762,-5.77162857796424,
27.1885780322763));
#18621=CARTESIAN_POINT('Ctrl Pts',(-1.47308179859639,-5.73044156912397,
27.180791585698));
#18622=CARTESIAN_POINT('Ctrl Pts',(-1.63330966334435,-5.68925298909204,
27.1730048420842));
#18623=CARTESIAN_POINT('Ctrl Pts',(-1.79181822886907,-5.64133766024962,
27.1652180984705));
#18624=CARTESIAN_POINT('Ctrl Pts',(-1.9480405326223,-5.58686572648391,27.1574313548567));
#18625=CARTESIAN_POINT('Ctrl Pts',(-2.10425250343885,-5.53239739562912,
27.1496451262778));
#18626=CARTESIAN_POINT('Ctrl Pts',(-2.25817821337433,-5.47137343301536,
27.1418588976989));
#18627=CARTESIAN_POINT('Ctrl Pts',(-2.40926798557749,-5.40401316950388,
27.13407266912));
#18628=CARTESIAN_POINT('Ctrl Pts',(-2.56039753162051,-5.33663517364497,
27.1262843908444));
#18629=CARTESIAN_POINT('Ctrl Pts',(-2.70868935531687,-5.26291767227535,
27.1184961125688));
#18630=CARTESIAN_POINT('Ctrl Pts',(-2.85361497985062,-5.1831276377562,27.1107078342932));
#18631=CARTESIAN_POINT('Ctrl Pts',(-2.99139591138917,-5.10727117469862,
27.1033035105972));
#18632=CARTESIAN_POINT('Ctrl Pts',(-3.12613431863912,-5.02592662276455,
27.0958991869012));
#18633=CARTESIAN_POINT('Ctrl Pts',(-3.25739774133065,-4.93936134710491,
27.0884948632051));
#18634=CARTESIAN_POINT('Ctrl Pts',(-3.3954625611294,-4.8483107029901,27.0807068854436));
#18635=CARTESIAN_POINT('Ctrl Pts',(-3.52973211226876,-4.7514513784177,27.0729189076821));
#18636=CARTESIAN_POINT('Ctrl Pts',(-3.65972298007034,-4.64912446291181,
27.0651309299206));
#18637=CARTESIAN_POINT('Ctrl Pts',(-3.78968829055197,-4.5468176657555,27.0573444833423));
#18638=CARTESIAN_POINT('Ctrl Pts',(-3.91537634525469,-4.43904562008982,
27.0495580367641));
#18639=CARTESIAN_POINT('Ctrl Pts',(-4.03633558395846,-4.32619065878641,
27.0417715901858));
#18640=CARTESIAN_POINT('Ctrl Pts',(-4.15729943698521,-4.21333139231997,
27.0339848465721));
#18641=CARTESIAN_POINT('Ctrl Pts',(-4.27353387670501,-4.09538903730922,
27.0261981029584));
#18642=CARTESIAN_POINT('Ctrl Pts',(-4.38462255438919,-3.97278436591286,
27.0184113593447));
#18643=CARTESIAN_POINT('Ctrl Pts',(-4.49570388438817,-3.85018780389856,
27.0106251307659));
#18644=CARTESIAN_POINT('Ctrl Pts',(-4.6016399189553,-3.72292977950718,27.002838902187));
#18645=CARTESIAN_POINT('Ctrl Pts',(-4.70205303033806,-3.59146597678283,
26.9950526736082));
#18646=CARTESIAN_POINT('Ctrl Pts',(-4.80249257511188,-3.45996756668441,
26.9872643953326));
#18647=CARTESIAN_POINT('Ctrl Pts',(-4.89740609587291,-3.32426141885105,
26.979476117057));
#18648=CARTESIAN_POINT('Ctrl Pts',(-4.98645738285165,-3.18483489862572,
26.9716878387815));
#18649=CARTESIAN_POINT('Ctrl Pts',(-5.07111852759153,-3.05228197087081,
26.9642835150852));
#18650=CARTESIAN_POINT('Ctrl Pts',(-5.15048137828395,-2.91636687807601,
26.9568791913889));
#18651=CARTESIAN_POINT('Ctrl Pts',(-5.22429421535204,-2.77753137046897,
26.9494748676926));
#18652=CARTESIAN_POINT('Ctrl Pts',(-5.30185754954526,-2.63164150493682,
26.9416943236011));
#18653=CARTESIAN_POINT('Ctrl Pts',(-5.37332042517392,-2.4824735504262,26.9339137795095));
#18654=CARTESIAN_POINT('Ctrl Pts',(-5.43842194674002,-2.33055729209056,
26.926133235418));
#18655=CARTESIAN_POINT('Ctrl Pts',(-5.50351045007573,-2.17867141216702,
26.9183542471874));
#18656=CARTESIAN_POINT('Ctrl Pts',(-5.56224001114736,-2.02403861961598,
26.9105752589568));
#18657=CARTESIAN_POINT('Ctrl Pts',(-5.61439743588298,-1.86720968143661,
26.9027962707262));
#18658=CARTESIAN_POINT('Ctrl Pts',(-5.66655651357155,-1.71037577309514,
26.8950170359669));
#18659=CARTESIAN_POINT('Ctrl Pts',(-5.71214293319581,-1.55134588299275,
26.8872378012077));
#18660=CARTESIAN_POINT('Ctrl Pts',(-5.75099281623643,-1.39068766806103,
26.8794585664484));
#18661=CARTESIAN_POINT('Ctrl Pts',(-5.78984035089331,-1.23003916453923,
26.8716798019255));
#18662=CARTESIAN_POINT('Ctrl Pts',(-5.82195208878417,-1.06776284505455,
26.8639010374026));
#18663=CARTESIAN_POINT('Ctrl Pts',(-5.84721485783825,-0.904438482582201,
26.8561222728797));
#18664=CARTESIAN_POINT('Ctrl Pts',(-5.87248402761934,-0.741072739267766,
26.8483415374823));
#18665=CARTESIAN_POINT('Ctrl Pts',(-5.89090071076948,-0.576658739365433,
26.8405608020848));
#18666=CARTESIAN_POINT('Ctrl Pts',(-5.90240326791351,-0.411784197637469,
26.8327800666874));
#18667=CARTESIAN_POINT('Ctrl Pts',(-5.91196558930545,-0.274720470188791,
26.8263117751932));
#18668=CARTESIAN_POINT('Ctrl Pts',(-5.91675050937049,-0.137338687105534,
26.8198434836991));
#18669=CARTESIAN_POINT('Ctrl Pts',(-5.91674999995931,2.19426670226234E-5,
26.8133751922049));
#18670=CARTESIAN_POINT('Ctrl Pts',(-5.91695430380796,0.0001364654751753,
26.5616248077951));
#18671=CARTESIAN_POINT('Ctrl Pts',(-5.91614190595471,-0.821753377324698,
26.6003185301115));
#18672=CARTESIAN_POINT('Ctrl Pts',(-5.53662360997084,-2.6281524630163,26.6853277141895));
#18673=CARTESIAN_POINT('Ctrl Pts',(-3.75791298936681,-4.89083127877313,
26.8166523600294));
#18674=CARTESIAN_POINT('Ctrl Pts',(-0.959963023245171,-6.09266867859071,
26.9555987453144));
#18675=CARTESIAN_POINT('Ctrl Pts',(2.07198210275202,-5.80939160316744,27.0945451305995));
#18676=CARTESIAN_POINT('Ctrl Pts',(4.59887258429633,-4.11005007104363,27.2334915158847));
#18677=CARTESIAN_POINT('Ctrl Pts',(6.00476788211649,-1.40886596771288,27.3724379011698));
#18678=CARTESIAN_POINT('Ctrl Pts',(5.94697490594146,1.63573533958923,27.5113842864549));
#18679=CARTESIAN_POINT('Ctrl Pts',(4.43958094493993,4.28161904732342,27.6503306717401));
#18680=CARTESIAN_POINT('Ctrl Pts',(1.85001982974811,5.8838395000729,27.7892770570252));
#18681=CARTESIAN_POINT('Ctrl Pts',(-1.19049166098134,6.05184849762528,27.9282234423103));
#18682=CARTESIAN_POINT('Ctrl Pts',(-3.94081563427965,4.74469311649309,28.0671698275954));
#18683=CARTESIAN_POINT('Ctrl Pts',(-5.58698077633417,2.47862958568841,28.194970282757));
#18684=CARTESIAN_POINT('Ctrl Pts',(-5.91595772284066,0.74696456590951,28.276455276157));
#18685=CARTESIAN_POINT('Ctrl Pts',(-5.91671909124951,-0.000153834640280791,
28.3116248077952));
#18686=CARTESIAN_POINT('Origin',(0.,0.,0.));
#18687=CARTESIAN_POINT('',(-5.9167499981344,0.000148581922998542,30.3133751922049));
#18688=CARTESIAN_POINT('',(-5.91674999882181,0.000118076772239281,30.0616248064854));
#18689=CARTESIAN_POINT('',(-5.91675,-7.2459289488551E-16,0.));
#18690=CARTESIAN_POINT('Ctrl Pts',(-5.91685455241636,0.000148584548576164,
30.3133751922049));
#18691=CARTESIAN_POINT('Ctrl Pts',(-5.91705466625152,0.194302987475124,
30.3042350481343));
#18692=CARTESIAN_POINT('Ctrl Pts',(-5.86018956337674,1.37269220639489,30.2487549055594));
#18693=CARTESIAN_POINT('Ctrl Pts',(-5.09914682414872,3.4704754948657,30.1469347644806));
#18694=CARTESIAN_POINT('Ctrl Pts',(-2.81582907770545,5.48785979229666,30.0079147689679));
#18695=CARTESIAN_POINT('Ctrl Pts',(0.154571517014471,6.16616624336598,29.8688947734555));
#18696=CARTESIAN_POINT('Ctrl Pts',(3.08725553333882,5.33988312293554,29.7298747779429));
#18697=CARTESIAN_POINT('Ctrl Pts',(5.26662666500381,3.21062954359113,29.5908547824305));
#18698=CARTESIAN_POINT('Ctrl Pts',(6.16090244821295,0.297958920558667,29.4518347869178));
#18699=CARTESIAN_POINT('Ctrl Pts',(5.55187306434934,-2.68741585395062,29.3128147914055));
#18700=CARTESIAN_POINT('Ctrl Pts',(3.58814612851256,-5.01704154409505,29.1737947958928));
#18701=CARTESIAN_POINT('Ctrl Pts',(0.748885346697635,-6.1224724770483,29.0347748003804));
#18702=CARTESIAN_POINT('Ctrl Pts',(-2.27310892598541,-5.73397543640903,
28.8957548048678));
#18703=CARTESIAN_POINT('Ctrl Pts',(-4.74044802882859,-3.94634653580834,
28.7567348093554));
#18704=CARTESIAN_POINT('Ctrl Pts',(-5.78497019753788,-1.75425870356025,
28.6459416083429));
#18705=CARTESIAN_POINT('Ctrl Pts',(-5.91655400292455,-0.384950057342253,
28.5814884058347));
#18706=CARTESIAN_POINT('Ctrl Pts',(-5.9163378217224,-9.39302684334942E-5,
28.5633752018305));
#18707=CARTESIAN_POINT('Ctrl Pts',(-5.91674999800012,-0.00015383611583252,
28.3116248078268));
#18708=CARTESIAN_POINT('Ctrl Pts',(-5.91674546782816,-0.174390521601554,
28.3198267083227));
#18709=CARTESIAN_POINT('Ctrl Pts',(-5.90904020723868,-0.348588844823986,
28.3280286088185));
#18710=CARTESIAN_POINT('Ctrl Pts',(-5.8936703221145,-0.522092613170047,
28.3362305093143));
#18711=CARTESIAN_POINT('Ctrl Pts',(-5.88815338161512,-0.584370890375815,
28.3391745389314));
#18712=CARTESIAN_POINT('Ctrl Pts',(-5.88164940694164,-0.646559714065766,
28.3421185685486));
#18713=CARTESIAN_POINT('Ctrl Pts',(-5.87416169919864,-0.708628883244091,
28.3450625981657));
#18714=CARTESIAN_POINT('Ctrl Pts',(-5.85435377959027,-0.872826145669539,
28.3528507095587));
#18715=CARTESIAN_POINT('Ctrl Pts',(-5.82765343558209,-1.03622168171102,
28.3606388209517));
#18716=CARTESIAN_POINT('Ctrl Pts',(-5.79414997686327,-1.19823061558089,
28.3684269323447));
#18717=CARTESIAN_POINT('Ctrl Pts',(-5.76065309596446,-1.36020774182113,
28.3762135146778));
#18718=CARTESIAN_POINT('Ctrl Pts',(-5.72035583008903,-1.52079849636549,
28.3840000970109));
#18719=CARTESIAN_POINT('Ctrl Pts',(-5.67339861665725,-1.67942808688303,
28.391786679344));
#18720=CARTESIAN_POINT('Ctrl Pts',(-5.62643961275753,-1.83806372591105,
28.3995735585777));
#18721=CARTESIAN_POINT('Ctrl Pts',(-5.57282024006913,-1.99473774378487,
28.4073604378114));
#18722=CARTESIAN_POINT('Ctrl Pts',(-5.51273105390054,-2.14888968769004,
28.4151473170452));
#18723=CARTESIAN_POINT('Ctrl Pts',(-5.45264583358346,-2.30303145765614,
28.4229336823494));
#18724=CARTESIAN_POINT('Ctrl Pts',(-5.38609177045433,-2.45465118906632,
28.4307200476536));
#18725=CARTESIAN_POINT('Ctrl Pts',(-5.31330794901207,-2.60320748336838,
28.4385064129578));
#18726=CARTESIAN_POINT('Ctrl Pts',(-5.24050501601631,-2.75180278553662,
28.4462948228034));
#18727=CARTESIAN_POINT('Ctrl Pts',(-5.16146919495497,-2.89733275526208,
28.454083232649));
#18728=CARTESIAN_POINT('Ctrl Pts',(-5.07648641286356,-3.03927890502199,
28.4618716424946));
#18729=CARTESIAN_POINT('Ctrl Pts',(-4.99596964243807,-3.17376550656331,
28.4692507561467));
#18730=CARTESIAN_POINT('Ctrl Pts',(-4.9101150169179,-3.3050350502794,28.4766298697987));
#18731=CARTESIAN_POINT('Ctrl Pts',(-4.81920242797586,-3.43266929964009,
28.4840089834508));
#18732=CARTESIAN_POINT('Ctrl Pts',(-4.7232508810693,-3.56737785658398,28.4917970948438));
#18733=CARTESIAN_POINT('Ctrl Pts',(-4.6216305131412,-3.69808482040399,28.4995852062369));
#18734=CARTESIAN_POINT('Ctrl Pts',(-4.51469957426996,-3.824319327225,28.5073733176299));
#18735=CARTESIAN_POINT('Ctrl Pts',(-4.40778962942439,-3.95052905010128,
28.5151598999631));
#18736=CARTESIAN_POINT('Ctrl Pts',(-4.29557140040973,-4.07226782436561,
28.5229464822963));
#18737=CARTESIAN_POINT('Ctrl Pts',(-4.17844320945086,-4.18909810196586,
28.5307330646294));
#18738=CARTESIAN_POINT('Ctrl Pts',(-4.06131055242033,-4.3059328342784,28.5385199438632));
#18739=CARTESIAN_POINT('Ctrl Pts',(-3.93926778225771,-4.41785846698047,
28.546306823097));
#18740=CARTESIAN_POINT('Ctrl Pts',(-3.81275037031918,-4.52447402204178,
28.5540937023308));
#18741=CARTESIAN_POINT('Ctrl Pts',(-3.68624130845656,-4.63108254053821,
28.5618800676351));
#18742=CARTESIAN_POINT('Ctrl Pts',(-3.55525844024118,-4.73238147689246,
28.5696664329394));
#18743=CARTESIAN_POINT('Ctrl Pts',(-3.42027073538813,-4.82800980313292,
28.5774527982437));
#18744=CARTESIAN_POINT('Ctrl Pts',(-3.28524758550497,-4.92366323942992,
28.5852412080894));
#18745=CARTESIAN_POINT('Ctrl Pts',(-3.146217757472,-5.01364290389254,28.593029617935));
#18746=CARTESIAN_POINT('Ctrl Pts',(-3.00368039306052,-5.09763029836843,
28.6008180277807));
#18747=CARTESIAN_POINT('Ctrl Pts',(-2.86863364636253,-5.17720399074333,
28.6081971414325));
#18748=CARTESIAN_POINT('Ctrl Pts',(-2.73043876117063,-5.2513988930982,28.6155762550842));
#18749=CARTESIAN_POINT('Ctrl Pts',(-2.58954161585625,-5.31998165243533,
28.6229553687359));
#18750=CARTESIAN_POINT('Ctrl Pts',(-2.44083504831392,-5.39236570756186,
28.6307434801289));
#18751=CARTESIAN_POINT('Ctrl Pts',(-2.28906506289486,-5.45852370854368,
28.6385315915218));
#18752=CARTESIAN_POINT('Ctrl Pts',(-2.13477152505278,-5.51821357853462,
28.6463197029148));
#18753=CARTESIAN_POINT('Ctrl Pts',(-1.98050828005729,-5.57789172946006,
28.6541062852478));
#18754=CARTESIAN_POINT('Ctrl Pts',(-1.82372276904173,-5.63110416801707,
28.6618928675808));
#18755=CARTESIAN_POINT('Ctrl Pts',(-1.66497410626174,-5.67765724467213,
28.6696794499138));
#18756=CARTESIAN_POINT('Ctrl Pts',(-1.50621939043053,-5.72421209638565,
28.6774663291475));
#18757=CARTESIAN_POINT('Ctrl Pts',(-1.34550167854417,-5.76410698440258,
28.6852532083812));
#18758=CARTESIAN_POINT('Ctrl Pts',(-1.18339520997047,-5.79719814561474,
28.6930400876149));
#18759=CARTESIAN_POINT('Ctrl Pts',(-1.02129944032978,-5.83028712282942,
28.700826452919));
#18760=CARTESIAN_POINT('Ctrl Pts',(-0.857815410541906,-5.85657320804385,
28.7086128182232));
#18761=CARTESIAN_POINT('Ctrl Pts',(-0.693527662131371,-5.87596374600445,
28.7163991835274));
#18762=CARTESIAN_POINT('Ctrl Pts',(-0.529196775094446,-5.89535937552653,
28.7241875933729));
#18763=CARTESIAN_POINT('Ctrl Pts',(-0.364062065039663,-5.90785580037143,
28.7319760032185));
#18764=CARTESIAN_POINT('Ctrl Pts',(-0.198714220497542,-5.91341214706637,
28.7397644130641));
#18765=CARTESIAN_POINT('Ctrl Pts',(-0.0420557290678969,-5.91867649685876,
28.7471435267164));
#18766=CARTESIAN_POINT('Ctrl Pts',(0.114793811812508,-5.91771142788405,
28.7545226403687));
#18767=CARTESIAN_POINT('Ctrl Pts',(0.271331221864757,-5.91052535148453,
28.761901754021));
#18768=CARTESIAN_POINT('Ctrl Pts',(0.436544937778181,-5.90294097670534,
28.769689865414));
#18769=CARTESIAN_POINT('Ctrl Pts',(0.601469946999545,-5.8884237145229,28.7774779768069));
#18770=CARTESIAN_POINT('Ctrl Pts',(0.765516363250975,-5.86701928240354,
28.7852660881998));
#18771=CARTESIAN_POINT('Ctrl Pts',(0.929530571848269,-5.84561905267131,
28.7930526705328));
#18772=CARTESIAN_POINT('Ctrl Pts',(1.09266621501012,-5.81733439231027,28.8008392528659));
#18773=CARTESIAN_POINT('Ctrl Pts',(1.25433967298034,-5.78226275322106,28.8086258351989));
#18774=CARTESIAN_POINT('Ctrl Pts',(1.41601929552353,-5.74718977685805,28.8164127144326));
#18775=CARTESIAN_POINT('Ctrl Pts',(1.57623630822345,-5.70532936781408,28.8241995936662));
#18776=CARTESIAN_POINT('Ctrl Pts',(1.7344176770428,-5.65683002078562,28.8319864728999));
#18777=CARTESIAN_POINT('Ctrl Pts',(1.89258860598323,-5.60833387468603,28.8397728382041));
#18778=CARTESIAN_POINT('Ctrl Pts',(2.04872385441977,-5.55319976122519,28.8475592035082));
#18779=CARTESIAN_POINT('Ctrl Pts',(2.202265793556,-5.49162598298838,28.8553455688124));
#18780=CARTESIAN_POINT('Ctrl Pts',(2.35584804968757,-5.43003603672776,28.8631339786579));
#18781=CARTESIAN_POINT('Ctrl Pts',(2.50683533835034,-5.36200316407788,28.8709223885035));
#18782=CARTESIAN_POINT('Ctrl Pts',(2.65468940715157,-5.28777407933218,28.878710798349));
#18783=CARTESIAN_POINT('Ctrl Pts',(2.79477345502364,-5.21744587838834,28.8860899120014));
#18784=CARTESIAN_POINT('Ctrl Pts',(2.93204489416862,-5.14155607783481,28.8934690256538));
#18785=CARTESIAN_POINT('Ctrl Pts',(3.06606589478054,-5.06035280305273,28.9008481393062));
#18786=CARTESIAN_POINT('Ctrl Pts',(3.20751519762847,-4.97464872268883,28.9086362506992));
#18787=CARTESIAN_POINT('Ctrl Pts',(3.34539404272668,-4.88299484310485,28.9164243620922));
#18788=CARTESIAN_POINT('Ctrl Pts',(3.47920631031759,-4.78571353224849,28.9242124734852));
#18789=CARTESIAN_POINT('Ctrl Pts',(3.61299230620244,-4.68845132088164,28.9319990558183));
#18790=CARTESIAN_POINT('Ctrl Pts',(3.74271305934025,-4.58556407051792,28.9397856381514));
#18791=CARTESIAN_POINT('Ctrl Pts',(3.86790270432689,-4.47741658016771,28.9475722204845));
#18792=CARTESIAN_POINT('Ctrl Pts',(3.99309712276678,-4.36926496617781,28.9553590997182));
#18793=CARTESIAN_POINT('Ctrl Pts',(4.11375984297218,-4.25585291674345,28.9631459789519));
#18794=CARTESIAN_POINT('Ctrl Pts',(4.22945871577383,-4.13758498813798,28.9709328581857));
#18795=CARTESIAN_POINT('Ctrl Pts',(4.34514995251681,-4.01932486514739,28.9787192234899));
#18796=CARTESIAN_POINT('Ctrl Pts',(4.45587777407664,-3.89620973283399,28.9865055887941));
#18797=CARTESIAN_POINT('Ctrl Pts',(4.56124738882818,-3.76868051450479,28.9942919540983));
#18798=CARTESIAN_POINT('Ctrl Pts',(4.66664467150083,-3.64111780959257,29.0020803639439));
#18799=CARTESIAN_POINT('Ctrl Pts',(4.76668073081876,-3.50913894789375,29.0098687737895));
#18800=CARTESIAN_POINT('Ctrl Pts',(4.86100095188754,-3.37321809378647,29.0176571836351));
#18801=CARTESIAN_POINT('Ctrl Pts',(4.95036446058173,-3.24444014680858,29.0250362972872));
#18802=CARTESIAN_POINT('Ctrl Pts',(5.0345972879751,-3.11212408346002,29.0324154109392));
#18803=CARTESIAN_POINT('Ctrl Pts',(5.11343367765309,-2.97669726152043,29.0397945245913));
#18804=CARTESIAN_POINT('Ctrl Pts',(5.19663968498426,-2.83376421771706,29.0475826359842));
#18805=CARTESIAN_POINT('Ctrl Pts',(5.27386379810543,-2.6873147523006,29.0553707473772));
#18806=CARTESIAN_POINT('Ctrl Pts',(5.34482459512685,-2.5378693051115,29.0631588587702));
#18807=CARTESIAN_POINT('Ctrl Pts',(5.41577146023278,-2.38845319893079,29.0709454411032));
#18808=CARTESIAN_POINT('Ctrl Pts',(5.48045732587137,-2.2360425730928,29.0787320234362));
#18809=CARTESIAN_POINT('Ctrl Pts',(5.53864763770795,-2.08118065237311,29.0865186057693));
#18810=CARTESIAN_POINT('Ctrl Pts',(5.59684016832818,-1.92631282680282,29.094305485003));
#18811=CARTESIAN_POINT('Ctrl Pts',(5.64853653346676,-1.76899381703139,29.1020923642367));
#18812=CARTESIAN_POINT('Ctrl Pts',(5.69355080706104,-1.60978562855883,29.1098792434704));
#18813=CARTESIAN_POINT('Ctrl Pts',(5.73856210973932,-1.45058794773457,29.1176656087745));
#18814=CARTESIAN_POINT('Ctrl Pts',(5.77689211658219,-1.28950164525325,29.1254519740787));
#18815=CARTESIAN_POINT('Ctrl Pts',(5.80840510531055,-1.12710278817076,29.1332383393829));
#18816=CARTESIAN_POINT('Ctrl Pts',(5.83992636870982,-0.964661288446265,
29.1410267492285));
#18817=CARTESIAN_POINT('Ctrl Pts',(5.86462697436654,-0.800906858951679,
29.1488151590741));
#18818=CARTESIAN_POINT('Ctrl Pts',(5.88242238380661,-0.636425534521513,
29.1566035689197));
#18819=CARTESIAN_POINT('Ctrl Pts',(5.89928260962293,-0.480588025876346,
29.1639826825719));
#18820=CARTESIAN_POINT('Ctrl Pts',(5.90994470743427,-0.324098315344506,
29.1713617962242));
#18821=CARTESIAN_POINT('Ctrl Pts',(5.9143797734987,-0.167458822787721,29.1787409098764));
#18822=CARTESIAN_POINT('Ctrl Pts',(5.91906065933036,-0.00213736630104985,
29.1865290212694));
#18823=CARTESIAN_POINT('Ctrl Pts',(5.91680632720862,0.1634099911377,29.1943171326624));
#18824=CARTESIAN_POINT('Ctrl Pts',(5.90761865092055,0.328591597268764,29.2021052440554));
#18825=CARTESIAN_POINT('Ctrl Pts',(5.89843277847256,0.49374077287092,29.2098918263884));
#18826=CARTESIAN_POINT('Ctrl Pts',(5.88231629567359,0.658524021607163,29.2176784087215));
#18827=CARTESIAN_POINT('Ctrl Pts',(5.85932313289708,0.822352106337153,29.2254649910546));
#18828=CARTESIAN_POINT('Ctrl Pts',(5.83632909339638,0.986186437795591,29.2332518702883));
#18829=CARTESIAN_POINT('Ctrl Pts',(5.80645788974177,1.14906521540755,29.241038749522));
#18830=CARTESIAN_POINT('Ctrl Pts',(5.76981513926322,1.31040597573004,29.2488256287557));
#18831=CARTESIAN_POINT('Ctrl Pts',(5.73317480718499,1.47173608765572,29.2566119940599));
#18832=CARTESIAN_POINT('Ctrl Pts',(5.68976389352247,1.631528073834,29.2643983593641));
#18833=CARTESIAN_POINT('Ctrl Pts',(5.63973882823814,1.78921114230912,29.2721847246683));
#18834=CARTESIAN_POINT('Ctrl Pts',(5.58970062738754,1.94693561515591,29.2799731345139));
#18835=CARTESIAN_POINT('Ctrl Pts',(5.53304489938063,2.10254975841753,29.2877615443595));
#18836=CARTESIAN_POINT('Ctrl Pts',(5.46997778878417,2.25549851534152,29.2955499542052));
#18837=CARTESIAN_POINT('Ctrl Pts',(5.41022497838645,2.40040951549063,29.3029290678573));
#18838=CARTESIAN_POINT('Ctrl Pts',(5.34471741392448,2.54292782599727,29.3103081815095));
#18839=CARTESIAN_POINT('Ctrl Pts',(5.27367008974176,2.68259843194301,29.3176872951616));
#18840=CARTESIAN_POINT('Ctrl Pts',(5.1986848678045,2.8300104774413,29.3254754065546));
#18841=CARTESIAN_POINT('Ctrl Pts',(5.11750159369404,2.97430283889159,29.3332635179475));
#18842=CARTESIAN_POINT('Ctrl Pts',(5.0304049801305,3.11495686942504,29.3410516293405));
#18843=CARTESIAN_POINT('Ctrl Pts',(4.94332546646876,3.25558328499151,29.3488382116736));
#18844=CARTESIAN_POINT('Ctrl Pts',(4.85033509797285,3.39257252343312,29.3566247940066));
#18845=CARTESIAN_POINT('Ctrl Pts',(4.75176314396138,3.52543296435916,29.3644113763397));
#18846=CARTESIAN_POINT('Ctrl Pts',(4.65318743142322,3.65829847122428,29.3721982555734));
#18847=CARTESIAN_POINT('Ctrl Pts',(4.54902989471648,3.78703460659917,29.3799851348071));
#18848=CARTESIAN_POINT('Ctrl Pts',(4.43966194988044,3.91118042709408,29.3877720140408));
#18849=CARTESIAN_POINT('Ctrl Pts',(4.33030122326549,4.03531805403664,29.395558379345));
#18850=CARTESIAN_POINT('Ctrl Pts',(4.21573098801031,4.15486573266453,29.4033447446491));
#18851=CARTESIAN_POINT('Ctrl Pts',(4.0963616958356,4.26939707914254,29.4111311099533));
#18852=CARTESIAN_POINT('Ctrl Pts',(3.9769610597088,4.38395849922635,29.4189195197989));
#18853=CARTESIAN_POINT('Ctrl Pts',(3.85275907802271,4.49350073237972,29.4267079296445));
#18854=CARTESIAN_POINT('Ctrl Pts',(3.72420232975072,4.59763499742849,29.4344963394901));
#18855=CARTESIAN_POINT('Ctrl Pts',(3.60240149041853,4.69629680286982,29.4418754531423));
#18856=CARTESIAN_POINT('Ctrl Pts',(3.4766920172817,4.79010425564088,29.4492545667945));
#18857=CARTESIAN_POINT('Ctrl Pts',(3.34748039696332,4.87876065763082,29.4566336804467));
#18858=CARTESIAN_POINT('Ctrl Pts',(3.21110704106634,4.97233096524966,29.4644217918396));
#18859=CARTESIAN_POINT('Ctrl Pts',(3.07078360093657,5.06019644036851,29.4722099032325));
#18860=CARTESIAN_POINT('Ctrl Pts',(2.92700822826401,5.14203786393826,29.4799980146254));
#18861=CARTESIAN_POINT('Ctrl Pts',(2.78326108337941,5.22386321937126,29.4877845969584));
#18862=CARTESIAN_POINT('Ctrl Pts',(2.63606363573782,5.29966672515556,29.4955711792914));
#18863=CARTESIAN_POINT('Ctrl Pts',(2.48594023277524,5.36917421225735,29.5033577616244));
#18864=CARTESIAN_POINT('Ctrl Pts',(2.33581110564082,5.43868434966413,29.511144640858));
#18865=CARTESIAN_POINT('Ctrl Pts',(2.18275608822847,5.50189785018816,29.5189315200916));
#18866=CARTESIAN_POINT('Ctrl Pts',(2.02732186101265,5.55858764744788,29.5267183993253));
#18867=CARTESIAN_POINT('Ctrl Pts',(1.87189789236584,5.61527370321381,29.5345047646294));
#18868=CARTESIAN_POINT('Ctrl Pts',(1.71409532839968,5.66543680795208,29.5422911299335));
#18869=CARTESIAN_POINT('Ctrl Pts',(1.55447859320192,5.70889891886141,29.5500774952376));
#18870=CARTESIAN_POINT('Ctrl Pts',(1.39481994589086,5.75237244203847,29.5578659050831));
#18871=CARTESIAN_POINT('Ctrl Pts',(1.23334648346908,5.78914136957265,29.5656543149287));
#18872=CARTESIAN_POINT('Ctrl Pts',(1.07063636375053,5.81907796296931,29.5734427247742));
#18873=CARTESIAN_POINT('Ctrl Pts',(0.916476979533205,5.84744132974438,29.5808218384267));
#18874=CARTESIAN_POINT('Ctrl Pts',(0.76120782825153,5.86967195038614,29.5882009520792));
#18875=CARTESIAN_POINT('Ctrl Pts',(0.605327805926907,5.88570376504558,29.5955800657317));
#18876=CARTESIAN_POINT('Ctrl Pts',(0.440807914380117,5.90262416555449,29.6033681771249));
#18877=CARTESIAN_POINT('Ctrl Pts',(0.275548756743581,5.91264516283174,29.611156288518));
#18878=CARTESIAN_POINT('Ctrl Pts',(0.110140497037312,5.91572477667888,29.6189443999111));
#18879=CARTESIAN_POINT('Ctrl Pts',(-0.0552352876407673,5.91880378589753,
29.6267309822443));
#18880=CARTESIAN_POINT('Ctrl Pts',(-0.220759796703246,5.91494412497204,
29.6345175645775));
#18881=CARTESIAN_POINT('Ctrl Pts',(-0.385841416563542,5.90415590611937,
29.6423041469107));
#18882=CARTESIAN_POINT('Ctrl Pts',(-0.550929330949217,5.89336727591432,
29.6500910261445));
#18883=CARTESIAN_POINT('Ctrl Pts',(-0.715574003248115,5.87564957604523,
29.6578779053784));
#18884=CARTESIAN_POINT('Ctrl Pts',(-0.879186744292628,5.85106496555628,
29.6656647846122));
#18885=CARTESIAN_POINT('Ctrl Pts',(-1.04278868699086,5.82648197763741,29.6734511499165));
#18886=CARTESIAN_POINT('Ctrl Pts',(-1.20535851873871,5.79503303364574,29.6812375152208));
#18887=CARTESIAN_POINT('Ctrl Pts',(-1.3663154239063,5.75683183052065,29.6890238805252));
#18888=CARTESIAN_POINT('Ctrl Pts',(-1.5273145930885,5.7186205965354,29.6968122903709));
#18889=CARTESIAN_POINT('Ctrl Pts',(-1.68669967786058,5.67365363252723,29.7046007002166));
#18890=CARTESIAN_POINT('Ctrl Pts',(-1.8439018700484,5.62209537949438,29.7123891100623));
#18891=CARTESIAN_POINT('Ctrl Pts',(-1.9928427790917,5.57324661365641,29.7197682237139));
#18892=CARTESIAN_POINT('Ctrl Pts',(-2.13982407791312,5.51848159175311,29.7271473373654));
#18893=CARTESIAN_POINT('Ctrl Pts',(-2.28437606916714,5.45798099457267,29.734526451017));
#18894=CARTESIAN_POINT('Ctrl Pts',(-2.43694005762399,5.3941270667935,29.7423145624099));
#18895=CARTESIAN_POINT('Ctrl Pts',(-2.58685229470455,5.32386092458106,29.7501026738028));
#18896=CARTESIAN_POINT('Ctrl Pts',(-2.73357445910418,5.24742805944334,29.7578907851957));
#18897=CARTESIAN_POINT('Ctrl Pts',(-2.88026781716449,5.17101020056631,29.7656773675288));
#18898=CARTESIAN_POINT('Ctrl Pts',(-3.02377206902146,5.08842818206036,29.7734639498618));
#18899=CARTESIAN_POINT('Ctrl Pts',(-3.16357254332143,4.99997393249633,29.7812505321948));
#18900=CARTESIAN_POINT('Ctrl Pts',(-3.30337834818231,4.91151631019148,29.7890374114285));
#18901=CARTESIAN_POINT('Ctrl Pts',(-3.43947982077722,4.81718617629317,29.7968242906622));
#18902=CARTESIAN_POINT('Ctrl Pts',(-3.57138975878909,4.71731976373411,29.8046111698958));
#18903=CARTESIAN_POINT('Ctrl Pts',(-3.70329099082135,4.61745994230051,29.8123975352));
#18904=CARTESIAN_POINT('Ctrl Pts',(-3.83100098716438,4.51206476638862,29.8201839005041));
#18905=CARTESIAN_POINT('Ctrl Pts',(-3.95406411698081,4.40151195855524,29.8279702658083));
#18906=CARTESIAN_POINT('Ctrl Pts',(-4.07715956067603,4.29093012179957,29.8357586756538));
#18907=CARTESIAN_POINT('Ctrl Pts',(-4.19560546053188,4.17518815920172,29.8435470854994));
#18908=CARTESIAN_POINT('Ctrl Pts',(-4.30898100747911,4.05470260804468,29.8513354953449));
#18909=CARTESIAN_POINT('Ctrl Pts',(-4.41639844735659,3.94054880860553,29.8587146089973));
#18910=CARTESIAN_POINT('Ctrl Pts',(-4.51926456323526,3.82213735630032,29.8660937226497));
#18911=CARTESIAN_POINT('Ctrl Pts',(-4.6172533472149,3.69985163082694,29.8734728363021));
#18912=CARTESIAN_POINT('Ctrl Pts',(-4.72067329720334,3.57078804722963,29.881260947695));
#18913=CARTESIAN_POINT('Ctrl Pts',(-4.81869685427459,3.43736244313912,29.8890490590879));
#18914=CARTESIAN_POINT('Ctrl Pts',(-4.91096875799744,3.30004794214768,29.8968371704808));
#18915=CARTESIAN_POINT('Ctrl Pts',(-5.00322254574043,3.1627604004649,29.9046237528138));
#18916=CARTESIAN_POINT('Ctrl Pts',(-5.08972675519242,3.02158575037327,29.9124103351468));
#18917=CARTESIAN_POINT('Ctrl Pts',(-5.1701691106124,2.87702657793935,29.9201969174798));
#18918=CARTESIAN_POINT('Ctrl Pts',(-5.25061453328166,2.73246189349605,29.9279837967135));
#18919=CARTESIAN_POINT('Ctrl Pts',(-5.32499748059826,2.58451270575827,29.9357706759472));
#18920=CARTESIAN_POINT('Ctrl Pts',(-5.39305099477828,2.43370736330829,29.9435575551808));
#18921=CARTESIAN_POINT('Ctrl Pts',(-5.46110001746565,2.28291197392387,29.9513439204849));
#18922=CARTESIAN_POINT('Ctrl Pts',(-5.52282031164343,2.12926109837163,29.9591302857891));
#18923=CARTESIAN_POINT('Ctrl Pts',(-5.57799249326393,1.97330441331064,29.9669166510932));
#18924=CARTESIAN_POINT('Ctrl Pts',(-5.63317916197895,1.81730677719116,29.9747050609387));
#18925=CARTESIAN_POINT('Ctrl Pts',(-5.68181417394764,1.65900242251507,29.9824934707843));
#18926=CARTESIAN_POINT('Ctrl Pts',(-5.72372729324552,1.49895845007668,29.9902818806298));
#18927=CARTESIAN_POINT('Ctrl Pts',(-5.76343779602619,1.3473251018791,29.9976609942823));
#18928=CARTESIAN_POINT('Ctrl Pts',(-5.79711466604073,1.19413052541016,30.0050401079347));
#18929=CARTESIAN_POINT('Ctrl Pts',(-5.82465505067723,1.03986734880957,30.0124192215872));
#18930=CARTESIAN_POINT('Ctrl Pts',(-5.85526262764347,0.868423771924959,
30.0206201524036));
#18931=CARTESIAN_POINT('Ctrl Pts',(-5.87829868295137,0.695613700489109,
30.0288210832199));
#18932=CARTESIAN_POINT('Ctrl Pts',(-5.89366966581137,0.522100021829988,
30.0370220140363));
#18933=CARTESIAN_POINT('Ctrl Pts',(-5.90904064867138,0.348586343170895,
30.0452229448527));
#18934=CARTESIAN_POINT('Ctrl Pts',(-5.91674652140112,0.174369358341535,
30.053423875669));
#18935=CARTESIAN_POINT('Ctrl Pts',(-5.91674999882181,0.000118076772239281,
30.0616248064854));
#18936=CARTESIAN_POINT('Origin',(0.,0.,0.));
#18937=CARTESIAN_POINT('',(-5.91674999804183,-0.000152223442091875,32.0633751922049));
#18938=CARTESIAN_POINT('',(-5.91722096325101,-5.21647111771487E-5,31.8116248077951));
#18939=CARTESIAN_POINT('',(-5.91675,-7.2459289488551E-16,0.));
#18940=CARTESIAN_POINT('Ctrl Pts',(-5.91674999804183,-0.000152223442091875,
32.0633751922049));
#18941=CARTESIAN_POINT('Ctrl Pts',(-5.91675423770661,0.164638666811161,
32.0556175243838));
#18942=CARTESIAN_POINT('Ctrl Pts',(-5.90986960240032,0.329452771156317,
32.0478598565627));
#18943=CARTESIAN_POINT('Ctrl Pts',(-5.89611634297487,0.493702980145559,
32.0401021887416));
#18944=CARTESIAN_POINT('Ctrl Pts',(-5.88236290911205,0.657955272377488,
32.0323444225272));
#18945=CARTESIAN_POINT('Ctrl Pts',(-5.86174069949175,0.821643331426469,
32.0245866563129));
#18946=CARTESIAN_POINT('Ctrl Pts',(-5.83432194704467,0.984183916111654,
32.0168288900986));
#18947=CARTESIAN_POINT('Ctrl Pts',(-5.8069047507725,1.14671527566602,32.009071564183));
#18948=CARTESIAN_POINT('Ctrl Pts',(-5.77269183800966,1.30809897145918,32.0013142382674));
#18949=CARTESIAN_POINT('Ctrl Pts',(-5.73180682219263,1.46776057842075,31.9935569123517));
#18950=CARTESIAN_POINT('Ctrl Pts',(-5.69091162717361,1.62746193656537,31.9857976550834));
#18951=CARTESIAN_POINT('Ctrl Pts',(-5.64334108984841,1.78544003472309,31.978038397815));
#18952=CARTESIAN_POINT('Ctrl Pts',(-5.58926930129603,1.94113349362938,31.9702791405467));
#18953=CARTESIAN_POINT('Ctrl Pts',(-5.55190687059043,2.048714289927,31.9649176624122));
#18954=CARTESIAN_POINT('Ctrl Pts',(-5.51144146350675,2.1552045628405,31.9595561842777));
#18955=CARTESIAN_POINT('Ctrl Pts',(-5.46794419499389,2.26042404051377,31.9541947061432));
#18956=CARTESIAN_POINT('Ctrl Pts',(-5.40476091766596,2.41326378575352,31.9464067283818));
#18957=CARTESIAN_POINT('Ctrl Pts',(-5.33515407285044,2.56348005742101,31.9386187506204));
#18958=CARTESIAN_POINT('Ctrl Pts',(-5.25936677102741,2.71053347706918,31.930830772859));
#18959=CARTESIAN_POINT('Ctrl Pts',(-5.18359436963759,2.85755798475445,31.9230443262808));
#18960=CARTESIAN_POINT('Ctrl Pts',(-5.1016440820839,3.00142059730995,31.9152578797026));
#18961=CARTESIAN_POINT('Ctrl Pts',(-5.01380555964883,3.14160538141481,31.9074714331244));
#18962=CARTESIAN_POINT('Ctrl Pts',(-4.92596368637224,3.281795513253,31.8996846895109));
#18963=CARTESIAN_POINT('Ctrl Pts',(-4.8322332950541,3.4183072630218,31.8918979458973));
#18964=CARTESIAN_POINT('Ctrl Pts',(-4.73294846204454,3.55065197085412,31.8841112022837));
#18965=CARTESIAN_POINT('Ctrl Pts',(-4.63367019598387,3.68298792507418,31.876324973705));
#18966=CARTESIAN_POINT('Ctrl Pts',(-4.52883841529292,3.81115713334293,31.8685387451263));
#18967=CARTESIAN_POINT('Ctrl Pts',(-4.4188288244114,3.93470232457945,31.8607525165475));
#18968=CARTESIAN_POINT('Ctrl Pts',(-4.30879027390029,4.05828003864374,31.8529642382721));
#18969=CARTESIAN_POINT('Ctrl Pts',(-4.19357140074275,4.17723106323152,31.8451759599966));
#18970=CARTESIAN_POINT('Ctrl Pts',(-4.07358687765908,4.29113277732858,31.8373876817212));
#18971=CARTESIAN_POINT('Ctrl Pts',(-3.9595174753985,4.39941924719643,31.8299833580244));
#18972=CARTESIAN_POINT('Ctrl Pts',(-3.84114117931065,4.50314208483321,31.8225790343276));
#18973=CARTESIAN_POINT('Ctrl Pts',(-3.7188439169604,4.60197028280134,31.8151747106308));
#18974=CARTESIAN_POINT('Ctrl Pts',(-3.59020983794156,4.70591925093371,31.8073867328691));
#18975=CARTESIAN_POINT('Ctrl Pts',(-3.45719166119068,4.80449006697312,31.7995987551075));
#18976=CARTESIAN_POINT('Ctrl Pts',(-3.32026101966087,4.89732552765492,31.7918107773458));
#18977=CARTESIAN_POINT('Ctrl Pts',(-3.18335729986928,4.99014273608914,31.7840243307673));
#18978=CARTESIAN_POINT('Ctrl Pts',(-3.04254291445834,5.07722665989015,31.7762378841889));
#18979=CARTESIAN_POINT('Ctrl Pts',(-2.89831913661993,5.15826295808993,31.7684514376104));
#18980=CARTESIAN_POINT('Ctrl Pts',(-2.75408985696947,5.23930234764184,31.7606646939966));
#18981=CARTESIAN_POINT('Ctrl Pts',(-2.60645120127714,5.31429348997774,31.7528779503828));
#18982=CARTESIAN_POINT('Ctrl Pts',(-2.45593039287091,5.38296725495083,31.7450912067689));
#18983=CARTESIAN_POINT('Ctrl Pts',(-2.30541954029006,5.45163647766815,31.7373049781899));
#18984=CARTESIAN_POINT('Ctrl Pts',(-2.15202720727318,5.51398902665044,31.7295187496109));
#18985=CARTESIAN_POINT('Ctrl Pts',(-1.99630214167263,5.5698032569969,31.7217325210319));
#18986=CARTESIAN_POINT('Ctrl Pts',(-1.84053608200802,5.62563218023898,31.7139442427562));
#18987=CARTESIAN_POINT('Ctrl Pts',(-1.68243636304442,5.67491923581839,31.7061559644805));
#18988=CARTESIAN_POINT('Ctrl Pts',(-1.52256936078756,5.71749185430911,31.6983676862048));
#18989=CARTESIAN_POINT('Ctrl Pts',(-1.37058364699569,5.75796568391719,31.6909633625092));
#18990=CARTESIAN_POINT('Ctrl Pts',(-1.21700095777804,5.79237109173358,31.6835590388137));
#18991=CARTESIAN_POINT('Ctrl Pts',(-1.06231857857277,5.82060218535154,31.6761547151182));
#18992=CARTESIAN_POINT('Ctrl Pts',(-0.899621352077626,5.85029606940069,
31.6683667373567));
#18993=CARTESIAN_POINT('Ctrl Pts',(-0.735649249453548,5.87316943120378,
31.6605787595953));
#18994=CARTESIAN_POINT('Ctrl Pts',(-0.570987344243469,5.88913440288246,
31.6527907818339));
#18995=CARTESIAN_POINT('Ctrl Pts',(-0.406357812975587,5.90509623571085,
31.6450043352556));
#18996=CARTESIAN_POINT('Ctrl Pts',(-0.24103906758913,5.91415235770217,31.6372178886774));
#18997=CARTESIAN_POINT('Ctrl Pts',(-0.0756216888676104,5.91626672173194,
31.6294314420992));
#18998=CARTESIAN_POINT('Ctrl Pts',(0.0898020001540977,5.91838116641994,
31.6216446984855));
#18999=CARTESIAN_POINT('Ctrl Pts',(0.255324010577674,5.91355331521411,31.6138579548719));
#19000=CARTESIAN_POINT('Ctrl Pts',(0.420352618437727,5.90179923740825,31.6060712112583));
#19001=CARTESIAN_POINT('Ctrl Pts',(0.58537031089004,5.89004593704669,31.5982849826795));
#19002=CARTESIAN_POINT('Ctrl Pts',(0.749894347324935,5.87136734966515,31.5904987541007));
#19003=CARTESIAN_POINT('Ctrl Pts',(0.913336834958877,5.84583153951662,31.5827125255219));
#19004=CARTESIAN_POINT('Ctrl Pts',(1.0768223482404,5.82028900715783,31.5749242472464));
#19005=CARTESIAN_POINT('Ctrl Pts',(1.23922542757045,5.78788569241109,31.5671359689709));
#19006=CARTESIAN_POINT('Ctrl Pts',(1.39996619353742,5.74874118563815,31.5593476906954));
#19007=CARTESIAN_POINT('Ctrl Pts',(1.55278259536065,5.71152646515204,31.5519433669988));
#19008=CARTESIAN_POINT('Ctrl Pts',(1.70409638054876,5.66821927252212,31.5445390433023));
#19009=CARTESIAN_POINT('Ctrl Pts',(1.85342024706657,5.61896466889263,31.5371347196057));
#19010=CARTESIAN_POINT('Ctrl Pts',(2.0104813102203,5.56715794441072,31.529346741844));
#19011=CARTESIAN_POINT('Ctrl Pts',(2.16539694881891,5.50875258474142,31.5215587640824));
#19012=CARTESIAN_POINT('Ctrl Pts',(2.31761141094465,5.44395149779635,31.5137707863208));
#19013=CARTESIAN_POINT('Ctrl Pts',(2.46979594640208,5.37916315130057,31.5059843397424));
#19014=CARTESIAN_POINT('Ctrl Pts',(2.61928007120168,5.30798171161369,31.498197893164));
#19015=CARTESIAN_POINT('Ctrl Pts',(2.76552800299021,5.23065822121623,31.4904114465855));
#19016=CARTESIAN_POINT('Ctrl Pts',(2.91178151380771,5.1533317811019,31.4826247029717));
#19017=CARTESIAN_POINT('Ctrl Pts',(3.05479830024734,5.06986296728665,31.4748379593579));
#19018=CARTESIAN_POINT('Ctrl Pts',(3.19406652267289,4.98054912747985,31.4670512157441));
#19019=CARTESIAN_POINT('Ctrl Pts',(3.3333255335475,4.89124119511534,31.4592649871651));
#19020=CARTESIAN_POINT('Ctrl Pts',(3.46883620762272,4.79608918302724,31.4514787585862));
#19021=CARTESIAN_POINT('Ctrl Pts',(3.6001149573141,4.69543425644778,31.4436925300072));
#19022=CARTESIAN_POINT('Ctrl Pts',(3.73142826566444,4.59475283282071,31.4359042517315));
#19023=CARTESIAN_POINT('Ctrl Pts',(3.85850716859779,4.48856579306073,31.4281159734559));
#19024=CARTESIAN_POINT('Ctrl Pts',(3.98089977810571,4.37725570639618,31.4203276951802));
#19025=CARTESIAN_POINT('Ctrl Pts',(4.09725855044077,4.27143309925618,31.4129233714845));
#19026=CARTESIAN_POINT('Ctrl Pts',(4.20938176350715,4.16098057729643,31.4055190477888));
#19027=CARTESIAN_POINT('Ctrl Pts',(4.31691100392656,4.04625875923398,31.3981147240931));
#19028=CARTESIAN_POINT('Ctrl Pts',(4.4300118579012,3.92559264514468,31.3903267463317));
#19029=CARTESIAN_POINT('Ctrl Pts',(4.53807048588826,3.80015989807773,31.3825387685702));
#19030=CARTESIAN_POINT('Ctrl Pts',(4.64069606511964,3.67040469072323,31.3747507908088));
#19031=CARTESIAN_POINT('Ctrl Pts',(4.7433014672825,3.54067499435469,31.3669643442305));
#19032=CARTESIAN_POINT('Ctrl Pts',(4.84047575392274,3.40662478384465,31.3591778976523));
#19033=CARTESIAN_POINT('Ctrl Pts',(4.93186867592241,3.26873093508097,31.351391451074));
#19034=CARTESIAN_POINT('Ctrl Pts',(5.02326508435588,3.13083182597805,31.3436047074604));
#19035=CARTESIAN_POINT('Ctrl Pts',(5.10887950700577,2.98908904938508,31.3358179638468));
#19036=CARTESIAN_POINT('Ctrl Pts',(5.18840488117236,2.84400867641553,31.3280312202332));
#19037=CARTESIAN_POINT('Ctrl Pts',(5.26792499533063,2.69893789942685,31.3202449916543));
#19038=CARTESIAN_POINT('Ctrl Pts',(5.3413567134468,2.55053024812114,31.3124587630755));
#19039=CARTESIAN_POINT('Ctrl Pts',(5.40843875203596,2.39931674190294,31.3046725344967));
#19040=CARTESIAN_POINT('Ctrl Pts',(5.4755384497306,2.24806342927286,31.2968842562212));
#19041=CARTESIAN_POINT('Ctrl Pts',(5.53628499637266,2.09400307728836,31.2890959779457));
#19042=CARTESIAN_POINT('Ctrl Pts',(5.59046475932937,1.93768788436022,31.2813076996702));
#19043=CARTESIAN_POINT('Ctrl Pts',(5.641973512425,1.78907887911106,31.2739033759737));
#19044=CARTESIAN_POINT('Ctrl Pts',(5.68754727099459,1.63843224937503,31.2664990522772));
#19045=CARTESIAN_POINT('Ctrl Pts',(5.72704396579689,1.48623617784303,31.2590947285807));
#19046=CARTESIAN_POINT('Ctrl Pts',(5.76858717668051,1.32615408674753,31.2513067508191));
#19047=CARTESIAN_POINT('Ctrl Pts',(5.80342170008898,1.16430045812298,31.2435187730576));
#19048=CARTESIAN_POINT('Ctrl Pts',(5.83141700601195,1.0012523480595,31.235730795296));
#19049=CARTESIAN_POINT('Ctrl Pts',(5.85940680781769,0.838236294652721,31.2279443487177));
#19050=CARTESIAN_POINT('Ctrl Pts',(5.8805600210661,0.674026543140648,31.2201579021394));
#19051=CARTESIAN_POINT('Ctrl Pts',(5.89479739321582,0.509209441621024,31.212371455561));
#19052=CARTESIAN_POINT('Ctrl Pts',(5.90903530848922,0.344386052700126,31.2045847119473));
#19053=CARTESIAN_POINT('Ctrl Pts',(5.91635682330807,0.178955585423101,31.1967979683336));
#19054=CARTESIAN_POINT('Ctrl Pts',(5.91673457744916,0.0135093492618925,
31.1890112247198));
#19055=CARTESIAN_POINT('Ctrl Pts',(5.91711230660464,-0.151925943868504,
31.1812249961409));
#19056=CARTESIAN_POINT('Ctrl Pts',(5.91054719354971,-0.317376684219718,
31.173438767562));
#19057=CARTESIAN_POINT('Ctrl Pts',(5.89706401397647,-0.482251570825563,
31.1656525389831));
#19058=CARTESIAN_POINT('Ctrl Pts',(5.88357728500462,-0.647169860153286,
31.1578642607075));
#19059=CARTESIAN_POINT('Ctrl Pts',(5.86316887457396,-0.811511673965455,
31.1500759824319));
#19060=CARTESIAN_POINT('Ctrl Pts',(5.83591553334913,-0.974689925111726,
31.1422877041563));
#19061=CARTESIAN_POINT('Ctrl Pts',(5.81000575546414,-1.12982364644094,31.1348833804602));
#19062=CARTESIAN_POINT('Ctrl Pts',(5.77790972978252,-1.28390550667541,31.1274790567642));
#19063=CARTESIAN_POINT('Ctrl Pts',(5.73973639713207,-1.43643887929052,31.1200747330681));
#19064=CARTESIAN_POINT('Ctrl Pts',(5.69958511823431,-1.59687574869264,31.1122867553065));
#19065=CARTESIAN_POINT('Ctrl Pts',(5.65269565908585,-1.7556567920871,31.1044987775449));
#19066=CARTESIAN_POINT('Ctrl Pts',(5.59922963270945,-1.91221287588188,31.0967107997832));
#19067=CARTESIAN_POINT('Ctrl Pts',(5.54577411821231,-2.06873817940807,31.0889243532048));
#19068=CARTESIAN_POINT('Ctrl Pts',(5.48574471963275,-2.22303909395251,31.0811379066263));
#19069=CARTESIAN_POINT('Ctrl Pts',(5.41935251920459,-2.37456287242324,31.0733514600479));
#19070=CARTESIAN_POINT('Ctrl Pts',(5.35295778606354,-2.52609243118478,31.0655647164341));
#19071=CARTESIAN_POINT('Ctrl Pts',(5.28019988999216,-2.67484434761829,31.0577779728203));
#19072=CARTESIAN_POINT('Ctrl Pts',(5.20133784933792,-2.82028635772057,31.0499912292064));
#19073=CARTESIAN_POINT('Ctrl Pts',(5.12248102481789,-2.9657187479216,31.0422050006275));
#19074=CARTESIAN_POINT('Ctrl Pts',(5.03752101609575,-3.10784138901246,31.0344187720485));
#19075=CARTESIAN_POINT('Ctrl Pts',(4.94676261259091,-3.24614698021713,31.0266325434695));
#19076=CARTESIAN_POINT('Ctrl Pts',(4.85598031726238,-3.38448897987184,31.0188442651938));
#19077=CARTESIAN_POINT('Ctrl Pts',(4.75939675086768,-3.51901165337453,31.0110559869182));
#19078=CARTESIAN_POINT('Ctrl Pts',(4.65736031964647,-3.64923627838519,31.0032677086425));
#19079=CARTESIAN_POINT('Ctrl Pts',(4.56035418571463,-3.77304095543843,30.9958633849469));
#19080=CARTESIAN_POINT('Ctrl Pts',(4.4584200403325,-3.8929609476009,30.9884590612512));
#19081=CARTESIAN_POINT('Ctrl Pts',(4.35189125203963,-4.00861236501123,30.9810547375556));
#19082=CARTESIAN_POINT('Ctrl Pts',(4.23984268848743,-4.13025624551777,30.9732667597942));
#19083=CARTESIAN_POINT('Ctrl Pts',(4.12267061707401,-4.24722097011238,30.9654787820328));
#19084=CARTESIAN_POINT('Ctrl Pts',(4.00078935909797,-4.35908420045179,30.9576908042715));
#19085=CARTESIAN_POINT('Ctrl Pts',(3.87893206402275,-4.47092543752055,30.9499043576933));
#19086=CARTESIAN_POINT('Ctrl Pts',(3.75236766504075,-4.57766696566869,30.9421179111152));
#19087=CARTESIAN_POINT('Ctrl Pts',(3.62154607355516,-4.67892451313518,30.934331464537));
#19088=CARTESIAN_POINT('Ctrl Pts',(3.49071949152024,-4.78018592334923,30.9265447209235));
#19089=CARTESIAN_POINT('Ctrl Pts',(3.35563564228066,-4.87596273555414,30.9187579773099));
#19090=CARTESIAN_POINT('Ctrl Pts',(3.21677672038713,-4.96591160751734,30.9109712336963));
#19091=CARTESIAN_POINT('Ctrl Pts',(3.07792698297249,-5.05585453003556,30.9031850051176));
#19092=CARTESIAN_POINT('Ctrl Pts',(2.93530294085811,-5.13997011005445,30.8953987765389));
#19093=CARTESIAN_POINT('Ctrl Pts',(2.7894150263476,-5.21795883208043,30.8876125479601));
#19094=CARTESIAN_POINT('Ctrl Pts',(2.64348870736769,-5.29596808435732,30.8798242696847));
#19095=CARTESIAN_POINT('Ctrl Pts',(2.49429708019934,-5.36784710330527,30.8720359914093));
#19096=CARTESIAN_POINT('Ctrl Pts',(2.34237519299164,-5.43334234313994,30.8642477131339));
#19097=CARTESIAN_POINT('Ctrl Pts',(2.19794290773552,-5.49560873106195,30.856843389437));
#19098=CARTESIAN_POINT('Ctrl Pts',(2.05104331813828,-5.55210550176354,30.8494390657401));
#19099=CARTESIAN_POINT('Ctrl Pts',(1.90215287609457,-5.60265517397467,30.8420347420432));
#19100=CARTESIAN_POINT('Ctrl Pts',(1.74554769525376,-5.65582407084546,30.8342467642815));
#19101=CARTESIAN_POINT('Ctrl Pts',(1.58668385225636,-5.70243223009608,30.8264587865199));
#19102=CARTESIAN_POINT('Ctrl Pts',(1.42612727925578,-5.74230716227045,30.8186708087582));
#19103=CARTESIAN_POINT('Ctrl Pts',(1.26560227305297,-5.78217425469154,30.8108843621797));
#19104=CARTESIAN_POINT('Ctrl Pts',(1.10338551082985,-5.8153106844528,30.8030979156012));
#19105=CARTESIAN_POINT('Ctrl Pts',(0.940055951492666,-5.84159442023864,
30.7953114690227));
#19106=CARTESIAN_POINT('Ctrl Pts',(0.776720161501561,-5.86787915868966,
30.7875247254089));
#19107=CARTESIAN_POINT('Ctrl Pts',(0.61227180430364,-5.8873106253971,30.779737981795));
#19108=CARTESIAN_POINT('Ctrl Pts',(0.447298591662922,-5.89981817790992,
30.7719512381812));
#19109=CARTESIAN_POINT('Ctrl Pts',(0.282336290765825,-5.91232490314173,
30.7641650096022));
#19110=CARTESIAN_POINT('Ctrl Pts',(0.116849522567173,-5.9179086065891,30.7563787810232));
#19111=CARTESIAN_POINT('Ctrl Pts',(-0.0485701869529832,-5.9165506420075,
30.7485925524441));
#19112=CARTESIAN_POINT('Ctrl Pts',(-0.21403344261702,-5.9151923199466,30.7408042741684));
#19113=CARTESIAN_POINT('Ctrl Pts',(-0.379429284559895,-5.9068886790572,
30.7330159958927));
#19114=CARTESIAN_POINT('Ctrl Pts',(-0.544166578376835,-5.8916732171326,
30.725227717617));
#19115=CARTESIAN_POINT('Ctrl Pts',(-0.70078248306895,-5.87720786275282,
30.7178233939215));
#19116=CARTESIAN_POINT('Ctrl Pts',(-0.856802944722839,-5.85649578754204,
30.710419070226));
#19117=CARTESIAN_POINT('Ctrl Pts',(-1.0117246858293,-5.82960922554708,30.7030147465305));
#19118=CARTESIAN_POINT('Ctrl Pts',(-1.17467367673134,-5.80132953985149,
30.6952267687691));
#19119=CARTESIAN_POINT('Ctrl Pts',(-1.33646535403249,-5.76620840269573,
30.6874387910077));
#19120=CARTESIAN_POINT('Ctrl Pts',(-1.49652026630087,-5.72436526219727,
30.6796508132462));
#19121=CARTESIAN_POINT('Ctrl Pts',(-1.65654371040109,-5.68253034841901,
30.671864366668));
#19122=CARTESIAN_POINT('Ctrl Pts',(-1.81483076181751,-5.63397614906018,
30.6640779200898));
#19123=CARTESIAN_POINT('Ctrl Pts',(-1.97081468433998,-5.57887264978238,
30.6562914735116));
#19124=CARTESIAN_POINT('Ctrl Pts',(-2.12680455729794,-5.52376704843013,
30.648504729898));
#19125=CARTESIAN_POINT('Ctrl Pts',(-2.28049082294545,-5.46211174992959,
30.6407179862844));
#19126=CARTESIAN_POINT('Ctrl Pts',(-2.43132365826553,-5.39412604888487,
30.6329312426708));
#19127=CARTESIAN_POINT('Ctrl Pts',(-2.58214651712199,-5.32614484458566,
30.625145014092));
#19128=CARTESIAN_POINT('Ctrl Pts',(-2.73011603203206,-5.2518342070657,30.6173587855132));
#19129=CARTESIAN_POINT('Ctrl Pts',(-2.87470391999606,-5.1714609091493,30.6095725569345));
#19130=CARTESIAN_POINT('Ctrl Pts',(-3.0193298702023,-5.09106645325087,30.601784278659));
#19131=CARTESIAN_POINT('Ctrl Pts',(-3.16057213421785,-5.00460630151462,
30.5939960003835));
#19132=CARTESIAN_POINT('Ctrl Pts',(-3.29792773249191,-4.91239282160545,
30.586207722108));
#19133=CARTESIAN_POINT('Ctrl Pts',(-3.4285118327504,-4.82472537698032,30.5788033984114));
#19134=CARTESIAN_POINT('Ctrl Pts',(-3.55558303503887,-4.73185835338873,
30.5713990747147));
#19135=CARTESIAN_POINT('Ctrl Pts',(-3.67873403961881,-4.63409607455972,
30.5639947510181));
#19136=CARTESIAN_POINT('Ctrl Pts',(-3.80826609741086,-4.53126825602626,
30.5562067732565));
#19137=CARTESIAN_POINT('Ctrl Pts',(-3.93350725881053,-4.42298763628546,
30.5484187954949));
#19138=CARTESIAN_POINT('Ctrl Pts',(-4.05400594348632,-4.30963645481584,
30.5406308177334));
#19139=CARTESIAN_POINT('Ctrl Pts',(-4.174480937088,-4.19630755915994,30.532844371155));
#19140=CARTESIAN_POINT('Ctrl Pts',(-4.29021508179072,-4.07791030972912,
30.5250579245766));
#19141=CARTESIAN_POINT('Ctrl Pts',(-4.40079215185238,-3.95486523141996,
30.5172714779982));
#19142=CARTESIAN_POINT('Ctrl Pts',(-4.51137344017982,-3.83181545921865,
30.5094847343844));
#19143=CARTESIAN_POINT('Ctrl Pts',(-4.61679704367759,-3.70411773837552,
30.5016979907706));
#19144=CARTESIAN_POINT('Ctrl Pts',(-4.71668518890512,-3.57222779106583,
30.4939112471568));
#19145=CARTESIAN_POINT('Ctrl Pts',(-4.81656672727858,-3.44034656729019,
30.486125018578));
#19146=CARTESIAN_POINT('Ctrl Pts',(-4.91091334720752,-3.30427392676269,
30.4783387899991));
#19147=CARTESIAN_POINT('Ctrl Pts',(-4.99938891358065,-3.16449696686011,
30.4705525614202));
#19148=CARTESIAN_POINT('Ctrl Pts',(-5.08788777082924,-3.02468321117427,
30.4627642831445));
#19149=CARTESIAN_POINT('Ctrl Pts',(-5.1705123135461,-2.88116345669998,30.4549760048689));
#19150=CARTESIAN_POINT('Ctrl Pts',(-5.24697044771608,-2.73445272098352,
30.4471877265933));
#19151=CARTESIAN_POINT('Ctrl Pts',(-5.31965926988517,-2.59497468251761,
30.4397834028974));
#19152=CARTESIAN_POINT('Ctrl Pts',(-5.38677491189971,-2.45261294217291,
30.4323790792014));
#19153=CARTESIAN_POINT('Ctrl Pts',(-5.44810543590136,-2.30782965614928,
30.4249747555055));
#19154=CARTESIAN_POINT('Ctrl Pts',(-5.51236203188601,-2.15613877682301,
30.4172171724094));
#19155=CARTESIAN_POINT('Ctrl Pts',(-5.5702925797576,-2.00173137472667,30.4094595893134));
#19156=CARTESIAN_POINT('Ctrl Pts',(-5.62168432073377,-1.84515472535939,
30.4017020062173));
#19157=CARTESIAN_POINT('Ctrl Pts',(-5.67306999690491,-1.68859655380263,
30.3939453386035));
#19158=CARTESIAN_POINT('Ctrl Pts',(-5.71791830102514,-1.52986995280867,
30.3861886709897));
#19159=CARTESIAN_POINT('Ctrl Pts',(-5.75606577235692,-1.3695391147394,30.378432003376));
#19160=CARTESIAN_POINT('Ctrl Pts',(-5.79420809090005,-1.20922993343773,
30.3706763834979));
#19161=CARTESIAN_POINT('Ctrl Pts',(-5.82565130915184,-1.04731726351005,
30.3629207636199));
#19162=CARTESIAN_POINT('Ctrl Pts',(-5.85028264031402,-0.884377516075805,
30.3551651437418));
#19163=CARTESIAN_POINT('Ctrl Pts',(-5.87491763671083,-0.721413522594905,
30.3474083697984));
#19164=CARTESIAN_POINT('Ctrl Pts',(-5.89273866988787,-0.557422466907766,
30.3396515958549));
#19165=CARTESIAN_POINT('Ctrl Pts',(-5.90368448065427,-0.392988696252073,
30.3318948219115));
#19166=CARTESIAN_POINT('Ctrl Pts',(-5.91239567784829,-0.262124475034702,
30.3257216120093));
#19167=CARTESIAN_POINT('Ctrl Pts',(-5.91675329104785,-0.130980059209622,
30.3195484021071));
#19168=CARTESIAN_POINT('Ctrl Pts',(-5.9167499981344,0.000148581922998542,
30.3133751922049));
#19169=CARTESIAN_POINT('Ctrl Pts',(-5.9164103286161,0.000118042167123383,
30.0616248077951));
#19170=CARTESIAN_POINT('Ctrl Pts',(-5.91595291218416,-0.635441998150383,
30.0915384074875));
#19171=CARTESIAN_POINT('Ctrl Pts',(-5.65595799765652,-2.255409947711,30.1677674689416));
#19172=CARTESIAN_POINT('Ctrl Pts',(-4.20296797278849,-4.51411130265866,
30.2903119921576));
#19173=CARTESIAN_POINT('Ctrl Pts',(-1.53101208436,-5.97479226673378,30.4292583774426));
#19174=CARTESIAN_POINT('Ctrl Pts',(1.51413465494195,-5.97909164336706,30.5682047627277));
#19175=CARTESIAN_POINT('Ctrl Pts',(4.19020449015913,-4.52596144081387,30.7071511480129));
#19176=CARTESIAN_POINT('Ctrl Pts',(5.84489376607425,-1.96960846270841,30.8460975332978));
#19177=CARTESIAN_POINT('Ctrl Pts',(6.07486477875718,1.06684514007426,30.9850439185832));
#19178=CARTESIAN_POINT('Ctrl Pts',(4.82406109417456,3.84325060238692,31.1239903038682));
#19179=CARTESIAN_POINT('Ctrl Pts',(2.39737154769186,5.68284702375448,31.2629366891533));
#19180=CARTESIAN_POINT('Ctrl Pts',(-0.613687734916818,6.13722477974293,
31.4018830744384));
#19181=CARTESIAN_POINT('Ctrl Pts',(-3.47515796443823,5.09562731714936,31.5408294597237));
#19182=CARTESIAN_POINT('Ctrl Pts',(-5.45524486659344,2.8508322079064,31.6774100375091));
#19183=CARTESIAN_POINT('Ctrl Pts',(-5.9167884154252,0.93335663078454,31.767675153533));
#19184=CARTESIAN_POINT('Ctrl Pts',(-5.91722096325101,-5.21647111771487E-5,
31.8116248077951));
#19185=CARTESIAN_POINT('Origin',(0.,0.,0.));
#19186=CARTESIAN_POINT('',(-5.91674999904992,0.000106031776716273,33.8133751922049));
#19187=CARTESIAN_POINT('',(-5.91670774978332,-3.97126980083329E-5,33.56162480823));
#19188=CARTESIAN_POINT('',(-5.91675,-7.2459289488551E-16,0.));
#19189=CARTESIAN_POINT('Ctrl Pts',(-5.91636959244526,0.000106239940256803,
33.8133751820867));
#19190=CARTESIAN_POINT('Ctrl Pts',(-5.9166048932696,0.367823780660049,33.7960683373264));
#19191=CARTESIAN_POINT('Ctrl Pts',(-5.79252506850152,1.71996775282403,33.7324214940625));
#19192=CARTESIAN_POINT('Ctrl Pts',(-4.77454453173828,3.90502535320764,33.622434652293));
#19193=CARTESIAN_POINT('Ctrl Pts',(-2.32282463106996,5.71401647075006,33.4834146567811));
#19194=CARTESIAN_POINT('Ctrl Pts',(0.695681434355644,6.12874586164393,33.3443946612684));
#19195=CARTESIAN_POINT('Ctrl Pts',(3.54443615188194,5.04801652730713,33.2053746657559));
#19196=CARTESIAN_POINT('Ctrl Pts',(5.52832257676672,2.73553431378993,33.0663546702434));
#19197=CARTESIAN_POINT('Ctrl Pts',(6.16325794055338,-0.244438239528186,
32.9273346747308));
#19198=CARTESIAN_POINT('Ctrl Pts',(5.29431337994305,-3.16476607819079,32.7883146792184));
#19199=CARTESIAN_POINT('Ctrl Pts',(3.13351771033575,-5.31286789349685,32.6492946837058));
#19200=CARTESIAN_POINT('Ctrl Pts',(0.208120847213036,-6.16459116305909,
32.5102746881934));
#19201=CARTESIAN_POINT('Ctrl Pts',(-2.76805902175141,-5.51210919220924,
32.3712546926806));
#19202=CARTESIAN_POINT('Ctrl Pts',(-5.06881228476578,-3.51463234443077,
32.2322346971683));
#19203=CARTESIAN_POINT('Ctrl Pts',(-5.85421735044904,-1.40697777682088,
32.1296081970096));
#19204=CARTESIAN_POINT('Ctrl Pts',(-5.91701880353749,-0.211440859014669,
32.0733216953552));
#19205=CARTESIAN_POINT('Ctrl Pts',(-5.91680012105169,-0.000152224731632677,
32.0633751922049));
#19206=CARTESIAN_POINT('Ctrl Pts',(-5.91722096325101,-5.21647111771487E-5,
31.8116248077951));
#19207=CARTESIAN_POINT('Ctrl Pts',(-5.91724424727696,-0.050297509426912,
31.8139906152947));
#19208=CARTESIAN_POINT('Ctrl Pts',(-5.90434996303826,-1.08418501485665,
31.8626718845569));
#19209=CARTESIAN_POINT('Ctrl Pts',(-5.33916643390619,-3.0879511693204,31.9576686155781));
#19210=CARTESIAN_POINT('Ctrl Pts',(-3.21105918801344,-5.2660459098046,32.0966150008645));
#19211=CARTESIAN_POINT('Ctrl Pts',(-0.300242306566234,-6.16051906826172,
32.235561386149));
#19212=CARTESIAN_POINT('Ctrl Pts',(2.6837599422594,-5.55333892405331,32.3745077714344));
#19213=CARTESIAN_POINT('Ctrl Pts',(5.01358403885356,-3.59250827673778,32.5134541567195));
#19214=CARTESIAN_POINT('Ctrl Pts',(6.1213252319243,-0.755988120332833,32.6524005420046));
#19215=CARTESIAN_POINT('Ctrl Pts',(5.7369667903094,2.26480742668442,32.7913469272897));
#19216=CARTESIAN_POINT('Ctrl Pts',(3.95419775495737,4.73354631832987,32.9302933125749));
#19217=CARTESIAN_POINT('Ctrl Pts',(1.20757582793818,6.04846271814959,33.06923969786));
#19218=CARTESIAN_POINT('Ctrl Pts',(-1.8333979564773,5.889040037754,33.2081860831451));
#19219=CARTESIAN_POINT('Ctrl Pts',(-4.42747301921854,4.29413824849268,33.3471324684302));
#19220=CARTESIAN_POINT('Ctrl Pts',(-5.71192511593987,2.05430638991628,33.4649453766469));
#19221=CARTESIAN_POINT('Ctrl Pts',(-5.91613373494868,0.535029129699535,
33.5364428231019));
#19222=CARTESIAN_POINT('Ctrl Pts',(-5.9162590580326,-3.97004485813632E-5,
33.5616248077952));
#19223=CARTESIAN_POINT('Origin',(0.,0.,0.));
#19224=CARTESIAN_POINT('',(-5.91674999986659,-3.97331449317638E-5,35.5633751921781));
#19225=CARTESIAN_POINT('',(-5.91674999872832,0.00012267210750124,35.3116248077951));
#19226=CARTESIAN_POINT('',(-5.91675,-7.2459289488551E-16,0.));
#19227=CARTESIAN_POINT('Ctrl Pts',(-5.91674999986659,-3.97331450085524E-5,
35.5633751921782));
#19228=CARTESIAN_POINT('Ctrl Pts',(-5.91675110866355,0.165073659927082,
35.5556001046463));
#19229=CARTESIAN_POINT('Ctrl Pts',(-5.9098363688167,0.330218136453832,35.5478250171145));
#19230=CARTESIAN_POINT('Ctrl Pts',(-5.89602402821719,0.494804225108879,
35.5400499295826));
#19231=CARTESIAN_POINT('Ctrl Pts',(-5.88221443243717,0.659357606844919,
35.5322763871337));
#19232=CARTESIAN_POINT('Ctrl Pts',(-5.86150999764133,0.823352501753403,
35.5245028446848));
#19233=CARTESIAN_POINT('Ctrl Pts',(-5.83398094014339,0.986203301831642,
35.5167293022359));
#19234=CARTESIAN_POINT('Ctrl Pts',(-5.8064510162699,1.1490592270382,35.5089555151434));
#19235=CARTESIAN_POINT('Ctrl Pts',(-5.77209608983898,1.31077066758484,35.501181728051));
#19236=CARTESIAN_POINT('Ctrl Pts',(-5.73103784694762,1.47076026576528,35.4934079409585));
#19237=CARTESIAN_POINT('Ctrl Pts',(-5.68998178598665,1.63074136172688,35.4856345669831));
#19238=CARTESIAN_POINT('Ctrl Pts',(-5.6422232020614,1.78900048701338,35.4778611930077));
#19239=CARTESIAN_POINT('Ctrl Pts',(-5.58793423630245,1.94497340168418,35.4700878190323));
#19240=CARTESIAN_POINT('Ctrl Pts',(-5.53363178425725,2.10098506263328,35.4623125140209));
#19241=CARTESIAN_POINT('Ctrl Pts',(-5.47279581395889,2.25470907396168,35.4545372090096));
#19242=CARTESIAN_POINT('Ctrl Pts',(-5.40564767678358,2.40559841972517,35.4467619039982));
#19243=CARTESIAN_POINT('Ctrl Pts',(-5.35651613899646,2.51600245928474,35.4410728006508));
#19244=CARTESIAN_POINT('Ctrl Pts',(-5.30400629601034,2.62488925785952,35.4353836973035));
#19245=CARTESIAN_POINT('Ctrl Pts',(-5.24822092842375,2.73205191183385,35.4296945939561));
#19246=CARTESIAN_POINT('Ctrl Pts',(-5.17185472875216,2.87874996160537,35.4219066161947));
#19247=CARTESIAN_POINT('Ctrl Pts',(-5.08932027418793,3.02227036060439,35.4141186384333));
#19248=CARTESIAN_POINT('Ctrl Pts',(-5.00090712050078,3.16209717349493,35.4063306606719));
#19249=CARTESIAN_POINT('Ctrl Pts',(-4.91251134959801,3.30189649523468,35.3985442140937));
#19250=CARTESIAN_POINT('Ctrl Pts',(-4.81823935641177,3.43800340990853,35.3907577675155));
#19251=CARTESIAN_POINT('Ctrl Pts',(-4.71842499787582,3.56992942534171,35.3829713209373));
#19252=CARTESIAN_POINT('Ctrl Pts',(-4.61860683164668,3.70186047345553,35.3751845773237));
#19253=CARTESIAN_POINT('Ctrl Pts',(-4.5132460666387,3.82961004597432,35.3673978337101));
#19254=CARTESIAN_POINT('Ctrl Pts',(-4.40271841707057,3.95272072153948,35.3596110900965));
#19255=CARTESIAN_POINT('Ctrl Pts',(-4.2921980780796,4.07582325425445,35.3518248615177));
#19256=CARTESIAN_POINT('Ctrl Pts',(-4.17651175200243,4.19428726630036,35.344038632939));
#19257=CARTESIAN_POINT('Ctrl Pts',(-4.05607386264036,4.30769026083651,35.3362524043602));
#19258=CARTESIAN_POINT('Ctrl Pts',(-3.93560426843669,4.42112310830347,35.3284641260848));
#19259=CARTESIAN_POINT('Ctrl Pts',(-3.81038084298499,4.52949205542597,35.3206758478093));
#19260=CARTESIAN_POINT('Ctrl Pts',(-3.68085378363544,4.63241254488379,35.3128875695338));
#19261=CARTESIAN_POINT('Ctrl Pts',(-3.55771228290983,4.7302591538541,35.3054832458371));
#19262=CARTESIAN_POINT('Ctrl Pts',(-3.43068146302759,4.82318140803664,35.2980789221404));
#19263=CARTESIAN_POINT('Ctrl Pts',(-3.30017483892539,4.91088348416289,35.2906745984437));
#19264=CARTESIAN_POINT('Ctrl Pts',(-3.16290603114694,5.00312983190472,35.2828866206821));
#19265=CARTESIAN_POINT('Ctrl Pts',(-3.02174255568152,5.08963367179141,35.2750986429204));
#19266=CARTESIAN_POINT('Ctrl Pts',(-2.87718560282573,5.17008061536688,35.2673106651588));
#19267=CARTESIAN_POINT('Ctrl Pts',(-2.73265707110554,5.25051174238391,35.2595242185803));
#19268=CARTESIAN_POINT('Ctrl Pts',(-2.58473667228175,5.32488819386679,35.2517377720018));
#19269=CARTESIAN_POINT('Ctrl Pts',(-2.43395135676673,5.39294088187451,35.2439513254234));
#19270=CARTESIAN_POINT('Ctrl Pts',(-2.28316028913237,5.46099616593862,35.2361645818095));
#19271=CARTESIAN_POINT('Ctrl Pts',(-2.12950437573891,5.52272706875576,35.2283778381957));
#19272=CARTESIAN_POINT('Ctrl Pts',(-1.97353244495761,5.57791181816275,35.2205910945819));
#19273=CARTESIAN_POINT('Ctrl Pts',(-1.81757083055295,5.63309291751131,35.2128048660029));
#19274=CARTESIAN_POINT('Ctrl Pts',(-1.65929380662418,5.68172862341769,35.2050186374239));
#19275=CARTESIAN_POINT('Ctrl Pts',(-1.49926747118925,5.72364635633036,35.1972324088449));
#19276=CARTESIAN_POINT('Ctrl Pts',(-1.33919900939618,5.76557512393569,35.1894441305692));
#19277=CARTESIAN_POINT('Ctrl Pts',(-1.17738062475237,5.80078230182907,35.1816558522935));
#19278=CARTESIAN_POINT('Ctrl Pts',(-1.01439166391229,5.82914574484849,35.1738675740179));
#19279=CARTESIAN_POINT('Ctrl Pts',(-0.859437901071764,5.85611089758226,
35.1664632503223));
#19280=CARTESIAN_POINT('Ctrl Pts',(-0.70342645794359,5.87689079478672,35.1590589266267));
#19281=CARTESIAN_POINT('Ctrl Pts',(-0.546862000065591,5.89142364080061,
35.1516546029311));
#19282=CARTESIAN_POINT('Ctrl Pts',(-0.382185175238075,5.90670950433382,
35.1438666251696));
#19283=CARTESIAN_POINT('Ctrl Pts',(-0.216837597273207,5.91508921676225,
35.1360786474082));
#19284=CARTESIAN_POINT('Ctrl Pts',(-0.0514097969037414,5.91652664958777,
35.1282906696468));
#19285=CARTESIAN_POINT('Ctrl Pts',(0.113985478942169,5.91796379980169,35.1205042230685));
#19286=CARTESIAN_POINT('Ctrl Pts',(0.279460626380191,5.91246139103857,35.1127177764903));
#19287=CARTESIAN_POINT('Ctrl Pts',(0.44442418126637,5.90003539901293,35.104931329912));
#19288=CARTESIAN_POINT('Ctrl Pts',(0.609394029139934,5.88760893296375,35.0971445862984));
#19289=CARTESIAN_POINT('Ctrl Pts',(0.773851926476321,5.86825837520351,35.0893578426848));
#19290=CARTESIAN_POINT('Ctrl Pts',(0.937209848880338,5.84205171679109,35.0815710990711));
#19291=CARTESIAN_POINT('Ctrl Pts',(1.10055696638013,5.81584679175302,35.0737848704924));
#19292=CARTESIAN_POINT('Ctrl Pts',(1.26280393901722,5.78278672427633,35.0659986419136));
#19293=CARTESIAN_POINT('Ctrl Pts',(1.42337112660555,5.74299096276894,35.0582124133348));
#19294=CARTESIAN_POINT('Ctrl Pts',(1.58398058292904,5.70318472517032,35.0504241350593));
#19295=CARTESIAN_POINT('Ctrl Pts',(1.74290905975723,5.65663932544496,35.0426358567838));
#19296=CARTESIAN_POINT('Ctrl Pts',(1.89958942594384,5.60352483490011,35.0348475785083));
#19297=CARTESIAN_POINT('Ctrl Pts',(2.04854560176359,5.55302883731768,35.0274432548117));
#19298=CARTESIAN_POINT('Ctrl Pts',(2.19546973729231,5.49659593095798,35.0200389311152));
#19299=CARTESIAN_POINT('Ctrl Pts',(2.33988915846553,5.43441342635942,35.0126346074187));
#19300=CARTESIAN_POINT('Ctrl Pts',(2.4917916530807,5.36900894340825,35.0048466296571));
#19301=CARTESIAN_POINT('Ctrl Pts',(2.64097731762214,5.29721981738107,34.9970586518954));
#19302=CARTESIAN_POINT('Ctrl Pts',(2.78691037473011,5.219296995355,34.9892706741338));
#19303=CARTESIAN_POINT('Ctrl Pts',(2.93281474014825,5.14138949362361,34.9814842275554));
#19304=CARTESIAN_POINT('Ctrl Pts',(3.07546749239553,5.05735085251538,34.973697780977));
#19305=CARTESIAN_POINT('Ctrl Pts',(3.21435697516471,4.96747821320939,34.9659113343985));
#19306=CARTESIAN_POINT('Ctrl Pts',(3.35325175625443,4.8776021454649,34.9581245907847));
#19307=CARTESIAN_POINT('Ctrl Pts',(3.48838271017851,4.78189180446256,34.9503378471709));
#19308=CARTESIAN_POINT('Ctrl Pts',(3.61926609876232,4.68068835416863,34.9425511035571));
#19309=CARTESIAN_POINT('Ctrl Pts',(3.75014083038907,4.57949159772585,34.9347648749781));
#19310=CARTESIAN_POINT('Ctrl Pts',(3.8767683061429,4.4728026546396,34.9269786463992));
#19311=CARTESIAN_POINT('Ctrl Pts',(3.99869678010585,4.36100385499384,34.9191924178202));
#19312=CARTESIAN_POINT('Ctrl Pts',(4.12065735130146,4.24917562471578,34.9114041395445));
#19313=CARTESIAN_POINT('Ctrl Pts',(4.23791621192222,4.13223506464507,34.9036158612689));
#19314=CARTESIAN_POINT('Ctrl Pts',(4.35005683046932,4.01060296391792,34.8958275829932));
#19315=CARTESIAN_POINT('Ctrl Pts',(4.45666902507436,3.89496720801654,34.8884232592975));
#19316=CARTESIAN_POINT('Ctrl Pts',(4.55865529147366,3.77509153916883,34.8810189356017));
#19317=CARTESIAN_POINT('Ctrl Pts',(4.6556902829983,3.65136666897412,34.873614611906));
#19318=CARTESIAN_POINT('Ctrl Pts',(4.75775312994153,3.52123101078173,34.8658266341446));
#19319=CARTESIAN_POINT('Ctrl Pts',(4.85437448996887,3.38679011705594,34.8580386563831));
#19320=CARTESIAN_POINT('Ctrl Pts',(4.94520407268016,3.24852077753053,34.8502506786217));
#19321=CARTESIAN_POINT('Ctrl Pts',(5.03601579751637,3.11027862294332,34.8424642320434));
#19322=CARTESIAN_POINT('Ctrl Pts',(5.121037841767,2.96820979134034,34.8346777854652));
#19323=CARTESIAN_POINT('Ctrl Pts',(5.19996320483517,2.82282008474864,34.826891338887));
#19324=CARTESIAN_POINT('Ctrl Pts',(5.27889157872833,2.67742483186683,34.8191045952734));
#19325=CARTESIAN_POINT('Ctrl Pts',(5.35172265012908,2.52870872944132,34.8113178516598));
#19326=CARTESIAN_POINT('Ctrl Pts',(5.41819500272893,2.37720286784769,34.8035311080461));
#19327=CARTESIAN_POINT('Ctrl Pts',(5.48466295867994,2.22570702723337,34.7957448794673));
#19328=CARTESIAN_POINT('Ctrl Pts',(5.54477290918273,2.07142208940072,34.7879586508885));
#19329=CARTESIAN_POINT('Ctrl Pts',(5.59831123188888,1.91489997477854,34.7801724223098));
#19330=CARTESIAN_POINT('Ctrl Pts',(5.65186364836615,1.75833665627195,34.7723841440343));
#19331=CARTESIAN_POINT('Ctrl Pts',(5.69884087488843,1.59953528609254,34.7645958657588));
#19332=CARTESIAN_POINT('Ctrl Pts',(5.73907861633046,1.43906469558475,34.7568075874833));
#19333=CARTESIAN_POINT('Ctrl Pts',(5.77733267607449,1.28650514983369,34.7494032637867));
#19334=CARTESIAN_POINT('Ctrl Pts',(5.80949567994419,1.13243725667251,34.7419989400902));
#19335=CARTESIAN_POINT('Ctrl Pts',(5.83546899562796,0.977359792279616,34.7345946163937));
#19336=CARTESIAN_POINT('Ctrl Pts',(5.86278811527093,0.81424700932731,34.7268066386321));
#19337=CARTESIAN_POINT('Ctrl Pts',(5.88326885368145,0.649958907278902,34.7190186608704));
#19338=CARTESIAN_POINT('Ctrl Pts',(5.8968318808334,0.485081778349647,34.7112306831088));
#19339=CARTESIAN_POINT('Ctrl Pts',(5.91039224137791,0.320237065677669,34.7034442365304));
#19340=CARTESIAN_POINT('Ctrl Pts',(5.91703757824452,0.154803875474242,34.695657789952));
#19341=CARTESIAN_POINT('Ctrl Pts',(5.91674045693324,-0.0106267487721454,
34.6878713433735));
#19342=CARTESIAN_POINT('Ctrl Pts',(5.91644332428745,-0.176063683823728,
34.6800845997597));
#19343=CARTESIAN_POINT('Ctrl Pts',(5.90920320013566,-0.341497733176881,
34.672297856146));
#19344=CARTESIAN_POINT('Ctrl Pts',(5.89504477752286,-0.506337469974766,
34.6645111125322));
#19345=CARTESIAN_POINT('Ctrl Pts',(5.88088729138377,-0.671166303857542,
34.6567248839532));
#19346=CARTESIAN_POINT('Ctrl Pts',(5.85981244995845,-0.83540058545418,34.6489386553742));
#19347=CARTESIAN_POINT('Ctrl Pts',(5.83189687988024,-0.99845347660424,34.6411524267952));
#19348=CARTESIAN_POINT('Ctrl Pts',(5.80397396112855,-1.16154929084184,34.6333641485196));
#19349=CARTESIAN_POINT('Ctrl Pts',(5.76920676738394,-1.32346277768841,34.6255758702439));
#19350=CARTESIAN_POINT('Ctrl Pts',(5.72772332910448,-1.48361586259124,34.6177875919682));
#19351=CARTESIAN_POINT('Ctrl Pts',(5.68828498417602,-1.63587355543733,34.6103832682725));
#19352=CARTESIAN_POINT('Ctrl Pts',(5.64277671780008,-1.78653998237889,34.6029789445767));
#19353=CARTESIAN_POINT('Ctrl Pts',(5.59135067902643,-1.93513000768699,34.595574620881));
#19354=CARTESIAN_POINT('Ctrl Pts',(5.53726000676726,-2.09141920575841,34.5877866431195));
#19355=CARTESIAN_POINT('Ctrl Pts',(5.47660267389509,-2.24546702005026,34.5799986653581));
#19356=CARTESIAN_POINT('Ctrl Pts',(5.40958966786325,-2.39672071544583,34.5722106875966));
#19357=CARTESIAN_POINT('Ctrl Pts',(5.34258983716308,-2.54794467306778,34.5644242410184));
#19358=CARTESIAN_POINT('Ctrl Pts',(5.2692369559449,-2.69637531592374,34.5566377944402));
#19359=CARTESIAN_POINT('Ctrl Pts',(5.18978985002381,-2.8414805779892,34.548851347862));
#19360=CARTESIAN_POINT('Ctrl Pts',(5.1103397133744,-2.98659137549389,34.5410646042483));
#19361=CARTESIAN_POINT('Ctrl Pts',(5.02479503681166,-3.12837625618952,34.5332778606347));
#19362=CARTESIAN_POINT('Ctrl Pts',(4.93346059745086,-3.26632776920807,34.525491117021));
#19363=CARTESIAN_POINT('Ctrl Pts',(4.84213219917998,-3.40427015776601,34.5177048884422));
#19364=CARTESIAN_POINT('Ctrl Pts',(4.74501498096641,-3.53837941963102,34.5099186598634));
#19365=CARTESIAN_POINT('Ctrl Pts',(4.64245712096745,-3.66817699170564,34.5021324312846));
#19366=CARTESIAN_POINT('Ctrl Pts',(4.53987226298036,-3.79800873252471,34.4943441530091));
#19367=CARTESIAN_POINT('Ctrl Pts',(4.43184409801895,-3.92352626340246,34.4865558747336));
#19368=CARTESIAN_POINT('Ctrl Pts',(4.31876174175831,-4.04428332098837,34.4787675964581));
#19369=CARTESIAN_POINT('Ctrl Pts',(4.21125423618384,-4.15908717254282,34.4713632727616));
#19370=CARTESIAN_POINT('Ctrl Pts',(4.09917904872532,-4.26958842537327,34.4639589490651));
#19371=CARTESIAN_POINT('Ctrl Pts',(3.98290198431529,-4.37543396085889,34.4565546253686));
#19372=CARTESIAN_POINT('Ctrl Pts',(3.86060003900228,-4.48676386893895,34.448766647607));
#19373=CARTESIAN_POINT('Ctrl Pts',(3.73360546681623,-4.59298260436608,34.4409786698454));
#19374=CARTESIAN_POINT('Ctrl Pts',(3.60236809021128,-4.69370586052509,34.4331906920838));
#19375=CARTESIAN_POINT('Ctrl Pts',(3.47115651599929,-4.79440931362872,34.4254042455053));
#19376=CARTESIAN_POINT('Ctrl Pts',(3.33570405512727,-4.88961924886052,34.4176177989269));
#19377=CARTESIAN_POINT('Ctrl Pts',(3.19649263833734,-4.9789924056535,34.4098313523484));
#19378=CARTESIAN_POINT('Ctrl Pts',(3.05727591094641,-5.06836897183047,34.4020446087346));
#19379=CARTESIAN_POINT('Ctrl Pts',(2.9143002074586,-5.15190813806547,34.3942578651209));
#19380=CARTESIAN_POINT('Ctrl Pts',(2.76807602121874,-5.22931025119507,34.3864711215071));
#19381=CARTESIAN_POINT('Ctrl Pts',(2.6218615066143,-5.30670724475425,34.3786848929281));
#19382=CARTESIAN_POINT('Ctrl Pts',(2.47239922173012,-5.37796784810523,34.3708986643491));
#19383=CARTESIAN_POINT('Ctrl Pts',(2.32022393823567,-5.44283854610241,34.3631124357702));
#19384=CARTESIAN_POINT('Ctrl Pts',(2.16800859514482,-5.50772632107767,34.3553241574945));
#19385=CARTESIAN_POINT('Ctrl Pts',(2.01307911973145,-5.56622070227697,34.3475358792188));
#19386=CARTESIAN_POINT('Ctrl Pts',(1.85599076582274,-5.61811612906682,34.3397476009432));
#19387=CARTESIAN_POINT('Ctrl Pts',(1.70664671570023,-5.66745316155069,34.3323432772474));
#19388=CARTESIAN_POINT('Ctrl Pts',(1.55535177097899,-5.71082612798686,34.3249389535517));
#19389=CARTESIAN_POINT('Ctrl Pts',(1.40259613340041,-5.7481000903838,34.317534629856));
#19390=CARTESIAN_POINT('Ctrl Pts',(1.24192548240169,-5.78730539827653,34.3097466520945));
#19391=CARTESIAN_POINT('Ctrl Pts',(1.07958127347967,-5.8197769080782,34.3019586743331));
#19392=CARTESIAN_POINT('Ctrl Pts',(0.91614240412713,-5.84539251529443,34.2941706965716));
#19393=CARTESIAN_POINT('Ctrl Pts',(0.752735668256952,-5.87100308626276,
34.2863842499934));
#19394=CARTESIAN_POINT('Ctrl Pts',(0.588235016885216,-5.88976039471291,
34.2785978034151));
#19395=CARTESIAN_POINT('Ctrl Pts',(0.423227891062269,-5.90159374361934,
34.2708113568368));
#19396=CARTESIAN_POINT('Ctrl Pts',(0.258214470590112,-5.91342754394132,
34.2630246132232));
#19397=CARTESIAN_POINT('Ctrl Pts',(0.092694855442932,-5.91833682938305,
34.2552378696095));
#19398=CARTESIAN_POINT('Ctrl Pts',(-0.0727393089072741,-5.91630286204482,
34.2474511259959));
#19399=CARTESIAN_POINT('Ctrl Pts',(-0.238162531025157,-5.91426902923831,
34.2396648974171));
#19400=CARTESIAN_POINT('Ctrl Pts',(-0.403499994105207,-5.90529286671043,
34.2318786688383));
#19401=CARTESIAN_POINT('Ctrl Pts',(-0.568160821156598,-5.88940776681346,
34.2240924402595));
#19402=CARTESIAN_POINT('Ctrl Pts',(-0.732864994579319,-5.87351848522099,
34.216304161984));
#19403=CARTESIAN_POINT('Ctrl Pts',(-0.896891857574877,-5.85071666076646,
34.2085158837085));
#19404=CARTESIAN_POINT('Ctrl Pts',(-1.05965550415079,-5.8210875938284,34.200727605433));
#19405=CARTESIAN_POINT('Ctrl Pts',(-1.21439506052433,-5.79291921120607,
34.1933232817365));
#19406=CARTESIAN_POINT('Ctrl Pts',(-1.36799269169004,-5.75858057085879,
34.18591895804));
#19407=CARTESIAN_POINT('Ctrl Pts',(-1.51995341190027,-5.71818784127915,
34.1785146343436));
#19408=CARTESIAN_POINT('Ctrl Pts',(-1.67978795697809,-5.67570216769271,
34.170726656582));
#19409=CARTESIAN_POINT('Ctrl Pts',(-1.83786863068062,-5.62650316646222,
34.1629386788204));
#19410=CARTESIAN_POINT('Ctrl Pts',(-1.99362871569015,-5.57076072960198,
34.1551507010588));
#19411=CARTESIAN_POINT('Ctrl Pts',(-2.14935817693191,-5.51502925218261,
34.1473642544804));
#19412=CARTESIAN_POINT('Ctrl Pts',(-2.30276765914971,-5.45275701367609,
34.139577807902));
#19413=CARTESIAN_POINT('Ctrl Pts',(-2.45330755088909,-5.38416313118859,
34.1317913613236));
#19414=CARTESIAN_POINT('Ctrl Pts',(-2.60385318538635,-5.31556663199895,
34.1240046177098));
#19415=CARTESIAN_POINT('Ctrl Pts',(-2.75152871794123,-5.24064813516452,
34.1162178740959));
#19416=CARTESIAN_POINT('Ctrl Pts',(-2.89580571676823,-5.1596743902336,34.1084311304821));
#19417=CARTESIAN_POINT('Ctrl Pts',(-3.0400731727512,-5.07870600111008,34.1006449019031));
#19418=CARTESIAN_POINT('Ctrl Pts',(-3.18094226620991,-4.99168332187697,
34.0928586733242));
#19419=CARTESIAN_POINT('Ctrl Pts',(-3.31791019313083,-4.89891850440672,
34.0850724447452));
#19420=CARTESIAN_POINT('Ctrl Pts',(-3.45491417636605,-4.8061292669318,34.0772841664695));
#19421=CARTESIAN_POINT('Ctrl Pts',(-3.58801467511241,-4.70759504842265,
34.0694958881938));
#19422=CARTESIAN_POINT('Ctrl Pts',(-3.71673809655088,-4.60367119635485,
34.0617076099182));
#19423=CARTESIAN_POINT('Ctrl Pts',(-3.83911557791681,-4.50487068959563,
34.0543032862224));
#19424=CARTESIAN_POINT('Ctrl Pts',(-3.95753695235454,-4.40119932135926,
34.0468989625267));
#19425=CARTESIAN_POINT('Ctrl Pts',(-4.07162323024594,-4.29299602066222,
34.039494638831));
#19426=CARTESIAN_POINT('Ctrl Pts',(-4.19162087373384,-4.17918618006405,
34.0317066610695));
#19427=CARTESIAN_POINT('Ctrl Pts',(-4.30686517396541,-4.06032158321635,
34.023918683308));
#19428=CARTESIAN_POINT('Ctrl Pts',(-4.41693987696012,-3.93682266375049,
34.0161307055465));
#19429=CARTESIAN_POINT('Ctrl Pts',(-4.52699293832519,-3.81334802523024,
34.0083442589681));
#19430=CARTESIAN_POINT('Ctrl Pts',(-4.63187821795671,-3.68524112050179,
34.0005578123898));
#19431=CARTESIAN_POINT('Ctrl Pts',(-4.73121804320277,-3.55295741462976,
33.9927713658114));
#19432=CARTESIAN_POINT('Ctrl Pts',(-4.83056165803863,-3.42066866243333,
33.9849846221977));
#19433=CARTESIAN_POINT('Ctrl Pts',(-4.92435920013832,-3.28420304339894,
33.977197878584));
#19434=CARTESIAN_POINT('Ctrl Pts',(-5.01227439261565,-3.144047705686,33.9694111349703));
#19435=CARTESIAN_POINT('Ctrl Pts',(-5.10018377016078,-3.00390163820001,
33.9616249063915));
#19436=CARTESIAN_POINT('Ctrl Pts',(-5.18221140695674,-2.86006661119489,
33.9538386778126));
#19437=CARTESIAN_POINT('Ctrl Pts',(-5.25806525981668,-2.71305736872793,
33.9460524492337));
#19438=CARTESIAN_POINT('Ctrl Pts',(-5.33393908093073,-2.56600942660631,
33.9382641709582));
#19439=CARTESIAN_POINT('Ctrl Pts',(-5.4036357222021,-2.41578588258479,33.9304758926827));
#19440=CARTESIAN_POINT('Ctrl Pts',(-5.46690946408993,-2.26292542385823,
33.9226876144071));
#19441=CARTESIAN_POINT('Ctrl Pts',(-5.52706387175656,-2.11760083776615,
33.9152832907109));
#19442=CARTESIAN_POINT('Ctrl Pts',(-5.58141330974059,-1.96989331219703,
33.9078789670147));
#19443=CARTESIAN_POINT('Ctrl Pts',(-5.62978726078636,-1.82028183553745,
33.9004746433185));
#19444=CARTESIAN_POINT('Ctrl Pts',(-5.68077981371215,-1.66257151878761,
33.8926695052266));
#19445=CARTESIAN_POINT('Ctrl Pts',(-5.72515014096265,-1.50268947405148,
33.8848643671348));
#19446=CARTESIAN_POINT('Ctrl Pts',(-5.76273333894475,-1.34120655631962,
33.877059229043));
#19447=CARTESIAN_POINT('Ctrl Pts',(-5.8003080494266,-1.17976010664736,33.8692558536035));
#19448=CARTESIAN_POINT('Ctrl Pts',(-5.8310986179747,-1.01671381375499,33.8614524781641));
#19449=CARTESIAN_POINT('Ctrl Pts',(-5.85499079240215,-0.852650798032842,
33.8536491027246));
#19450=CARTESIAN_POINT('Ctrl Pts',(-5.87888163475403,-0.688596929420129,
33.8458461623516));
#19451=CARTESIAN_POINT('Ctrl Pts',(-5.89587480235716,-0.523526763995115,
33.8380432219787));
#19452=CARTESIAN_POINT('Ctrl Pts',(-5.90590756190641,-0.358031329239078,
33.8302402816058));
#19453=CARTESIAN_POINT('Ctrl Pts',(-5.91313575105257,-0.238798699435666,
33.8246185851388));
#19454=CARTESIAN_POINT('Ctrl Pts',(-5.91675213969457,-0.119345510029993,
33.8189968886719));
#19455=CARTESIAN_POINT('Ctrl Pts',(-5.91674999904992,0.000106031776716273,
33.8133751922049));
#19456=CARTESIAN_POINT('Ctrl Pts',(-5.91674999986672,-3.97138514489972E-5,
33.5616248082709));
#19457=CARTESIAN_POINT('Ctrl Pts',(-5.9167488701323,-0.168352679007752,
33.569545476781));
#19458=CARTESIAN_POINT('Ctrl Pts',(-5.90956143709304,-0.336644184720461,
33.5774661452911));
#19459=CARTESIAN_POINT('Ctrl Pts',(-5.89521918275979,-0.504302835329105,
33.5853868138013));
#19460=CARTESIAN_POINT('Ctrl Pts',(-5.88087213540043,-0.672017515643508,
33.593310129313));
#19461=CARTESIAN_POINT('Ctrl Pts',(-5.85936551470131,-0.839098623772593,
33.6012334448248));
#19462=CARTESIAN_POINT('Ctrl Pts',(-5.83078272279159,-1.00493950170897,
33.6091567603366));
#19463=CARTESIAN_POINT('Ctrl Pts',(-5.81170125692052,-1.11565251611173,
33.6144462532245));
#19464=CARTESIAN_POINT('Ctrl Pts',(-5.78946721870051,-1.22581291257659,
33.6197357461125));
#19465=CARTESIAN_POINT('Ctrl Pts',(-5.76411814781709,-1.3352425025087,33.6250252390004));
#19466=CARTESIAN_POINT('Ctrl Pts',(-5.72679483688146,-1.496363777106,33.6328133503934));
#19467=CARTESIAN_POINT('Ctrl Pts',(-5.6827050274659,-1.65594791878048,33.6406014617864));
#19468=CARTESIAN_POINT('Ctrl Pts',(-5.63200031122108,-1.81342302205131,
33.6483895731793));
#19469=CARTESIAN_POINT('Ctrl Pts',(-5.58130554996344,-1.97086720783061,
33.6561761555124));
#19470=CARTESIAN_POINT('Ctrl Pts',(-5.52399857108406,-2.12620287744186,
33.6639627378455));
#19471=CARTESIAN_POINT('Ctrl Pts',(-5.46028071573764,-2.27887364016606,
33.6717493201785));
#19472=CARTESIAN_POINT('Ctrl Pts',(-5.39656043084349,-2.43155022419266,
33.6795361994123));
#19473=CARTESIAN_POINT('Ctrl Pts',(-5.32642889976689,-2.58156140161961,
33.687323078646));
#19474=CARTESIAN_POINT('Ctrl Pts',(-5.2501357521873,-2.72837041951872,33.6951099578797));
#19475=CARTESIAN_POINT('Ctrl Pts',(-5.17384763991122,-2.87516974810775,
33.7028963231839));
#19476=CARTESIAN_POINT('Ctrl Pts',(-5.09139887238669,-3.01876705659778,
33.7106826884881));
#19477=CARTESIAN_POINT('Ctrl Pts',(-5.00308528208094,-3.15864974676286,
33.7184690537924));
#19478=CARTESIAN_POINT('Ctrl Pts',(-4.91474850241982,-3.29856916728168,
33.726257463638));
#19479=CARTESIAN_POINT('Ctrl Pts',(-4.82054399182033,-3.43477174905532,
33.7340458734836));
#19480=CARTESIAN_POINT('Ctrl Pts',(-4.72081169453193,-3.56677270193526,
33.7418342833292));
#19481=CARTESIAN_POINT('Ctrl Pts',(-4.62632052482366,-3.69183674617524,
33.7492133969813));
#19482=CARTESIAN_POINT('Ctrl Pts',(-4.5268677738479,-3.81312920329694,33.7565925106335));
#19483=CARTESIAN_POINT('Ctrl Pts',(-4.42277662140855,-3.93026430658575,
33.7639716242856));
#19484=CARTESIAN_POINT('Ctrl Pts',(-4.31291607061109,-4.0538917875335,33.7717597356786));
#19485=CARTESIAN_POINT('Ctrl Pts',(-4.19784912163827,-4.1729321454896,33.7795478470716));
#19486=CARTESIAN_POINT('Ctrl Pts',(-4.07798251032837,-4.28695570398808,
33.7873359584645));
#19487=CARTESIAN_POINT('Ctrl Pts',(-3.9581394327382,-4.4009568759484,33.7951225407976));
#19488=CARTESIAN_POINT('Ctrl Pts',(-3.83349880440956,-4.50994299364982,
33.8029091231306));
#19489=CARTESIAN_POINT('Ctrl Pts',(-3.70450362454666,-4.61352180641001,
33.8106957054637));
#19490=CARTESIAN_POINT('Ctrl Pts',(-3.5755035261262,-4.71710456860731,33.8184825846974));
#19491=CARTESIAN_POINT('Ctrl Pts',(-3.44214879059609,-4.81527941016946,
33.8262694639311));
#19492=CARTESIAN_POINT('Ctrl Pts',(-3.30491542500478,-4.90769442773951,
33.8340563431648));
#19493=CARTESIAN_POINT('Ctrl Pts',(-3.16769111673621,-5.00010334597187,
33.841842708469));
#19494=CARTESIAN_POINT('Ctrl Pts',(-3.02658895579834,-5.0867530225459,33.8496290737731));
#19495=CARTESIAN_POINT('Ctrl Pts',(-2.88211396450086,-5.16733486994303,
33.8574154390773));
#19496=CARTESIAN_POINT('Ctrl Pts',(-2.73760103700449,-5.24793787649692,
33.8652038489229));
#19497=CARTESIAN_POINT('Ctrl Pts',(-2.58971378775667,-5.3224697127073,33.8729922587685));
#19498=CARTESIAN_POINT('Ctrl Pts',(-2.43898267026516,-5.39066731459531,
33.8807806686141));
#19499=CARTESIAN_POINT('Ctrl Pts',(-2.29617276825122,-5.45528099891807,
33.8881597822663));
#19500=CARTESIAN_POINT('Ctrl Pts',(-2.15081044874833,-5.51420897105778,
33.8955388959185));
#19501=CARTESIAN_POINT('Ctrl Pts',(-2.0033640677192,-5.56726710107137,33.9029180095707));
#19502=CARTESIAN_POINT('Ctrl Pts',(-1.84774526388196,-5.62326605247949,
33.9107061209636));
#19503=CARTESIAN_POINT('Ctrl Pts',(-1.68974924436139,-5.67274602199669,
33.9184942323565));
#19504=CARTESIAN_POINT('Ctrl Pts',(-1.52993874555476,-5.71552429767824,
33.9262823437494));
#19505=CARTESIAN_POINT('Ctrl Pts',(-1.37015962275342,-5.75829417459116,
33.9340689260824));
#19506=CARTESIAN_POINT('Ctrl Pts',(-1.20856703994434,-5.79436490043047,
33.9418555084154));
#19507=CARTESIAN_POINT('Ctrl Pts',(-1.04573767139948,-5.82360397735938,
33.9496420907484));
#19508=CARTESIAN_POINT('Ctrl Pts',(-0.882902094207371,-5.85284416916773,
33.9574289699821));
#19509=CARTESIAN_POINT('Ctrl Pts',(-0.718829950703475,-5.87525213046855,
33.9652158492157));
#19510=CARTESIAN_POINT('Ctrl Pts',(-0.554107596518002,-5.89074658544917,
33.9730027284493));
#19511=CARTESIAN_POINT('Ctrl Pts',(-0.3893961139125,-5.90624001780474,33.9807890937535));
#19512=CARTESIAN_POINT('Ctrl Pts',(-0.224034824661971,-5.91482082713235,
33.9885754590576));
#19513=CARTESIAN_POINT('Ctrl Pts',(-0.0586148395352926,-5.91645965616992,
33.9963618243617));
#19514=CARTESIAN_POINT('Ctrl Pts',(0.106848581520312,-5.91809891553071,
34.0041502342073));
#19515=CARTESIAN_POINT('Ctrl Pts',(0.272370409545367,-5.91279254711233,
34.0119386440528));
#19516=CARTESIAN_POINT('Ctrl Pts',(0.437358982122217,-5.90056333609402,
34.0197270538983));
#19517=CARTESIAN_POINT('Ctrl Pts',(0.593677082036207,-5.88897679406888,
34.0271061675508));
#19518=CARTESIAN_POINT('Ctrl Pts',(0.749516272802175,-5.87117633185597,
34.0344852812033));
#19519=CARTESIAN_POINT('Ctrl Pts',(0.904377186100404,-5.84722433875776,
34.0418643948558));
#19520=CARTESIAN_POINT('Ctrl Pts',(1.06782148307199,-5.82194477279352,34.0496525062489));
#19521=CARTESIAN_POINT('Ctrl Pts',(1.23023435657831,-5.78980339621259,34.057440617642));
#19522=CARTESIAN_POINT('Ctrl Pts',(1.39103423910614,-5.75090899842229,34.0652287290351));
#19523=CARTESIAN_POINT('Ctrl Pts',(1.55180255138019,-5.71202223686896,34.0730153113683));
#19524=CARTESIAN_POINT('Ctrl Pts',(1.71095819417121,-5.66638517462235,34.0808018937014));
#19525=CARTESIAN_POINT('Ctrl Pts',(1.86793138500003,-5.61415736361494,34.0885884760346));
#19526=CARTESIAN_POINT('Ctrl Pts',(2.02491056118163,-5.56192756117274,34.0963753552685));
#19527=CARTESIAN_POINT('Ctrl Pts',(2.17970681446322,-5.50310660423615,34.1041622345023));
#19528=CARTESIAN_POINT('Ctrl Pts',(2.33176636736659,-5.43790365586942,34.1119491137361));
#19529=CARTESIAN_POINT('Ctrl Pts',(2.48381588442738,-5.37270501085959,34.1197354790405));
#19530=CARTESIAN_POINT('Ctrl Pts',(2.63312876891438,-5.30112534336405,34.1275218443448));
#19531=CARTESIAN_POINT('Ctrl Pts',(2.77917190741901,-5.22342168233745,34.1353082096491));
#19532=CARTESIAN_POINT('Ctrl Pts',(2.92525339388609,-5.1456976179074,34.1430966194948));
#19533=CARTESIAN_POINT('Ctrl Pts',(3.06806313558781,-5.06184649522597,34.1508850293405));
#19534=CARTESIAN_POINT('Ctrl Pts',(3.20709248148285,-4.97217139464401,34.1586734391862));
#19535=CARTESIAN_POINT('Ctrl Pts',(3.33881556290646,-4.88720889626222,34.1660525528378));
#19536=CARTESIAN_POINT('Ctrl Pts',(3.46714514473233,-4.79701893974729,34.1734316664894));
#19537=CARTESIAN_POINT('Ctrl Pts',(3.59167256948262,-4.70189522598347,34.1808107801411));
#19538=CARTESIAN_POINT('Ctrl Pts',(3.72310210170258,-4.60149914674169,34.188598891534));
#19539=CARTESIAN_POINT('Ctrl Pts',(3.85034298526206,-4.49557102432411,34.1963870029269));
#19540=CARTESIAN_POINT('Ctrl Pts',(3.97293658114135,-4.38448463159912,34.2041751143198));
#19541=CARTESIAN_POINT('Ctrl Pts',(4.09550610790508,-4.27342004875094,34.2119616966528));
#19542=CARTESIAN_POINT('Ctrl Pts',(4.21342993089196,-4.15719943072787,34.2197482789858));
#19543=CARTESIAN_POINT('Ctrl Pts',(4.32628404637179,-4.03623548775451,34.2275348613189));
#19544=CARTESIAN_POINT('Ctrl Pts',(4.43914246495403,-3.91526693245282,34.2353217405525));
#19545=CARTESIAN_POINT('Ctrl Pts',(4.54693056837072,-3.78955492123015,34.2431086197862));
#19546=CARTESIAN_POINT('Ctrl Pts',(4.64926214296325,-3.65954807162151,34.2508954990199));
#19547=CARTESIAN_POINT('Ctrl Pts',(4.75158696373108,-3.52954980238971,34.258681864324));
#19548=CARTESIAN_POINT('Ctrl Pts',(4.84845577879255,-3.39525751318412,34.2664682296282));
#19549=CARTESIAN_POINT('Ctrl Pts',(4.93952342081019,-3.25715196725108,34.2742545949323));
#19550=CARTESIAN_POINT('Ctrl Pts',(5.03061497534125,-3.11901015760628,34.2820430047779));
#19551=CARTESIAN_POINT('Ctrl Pts',(5.11590213538125,-2.97705335632145,34.2898314146234));
#19552=CARTESIAN_POINT('Ctrl Pts',(5.19508324716767,-2.83179106176601,34.297619824469));
#19553=CARTESIAN_POINT('Ctrl Pts',(5.27010323643119,-2.69416258532658,34.3049989381213));
#19554=CARTESIAN_POINT('Ctrl Pts',(5.33964231592452,-2.55356732845023,34.3123780517737));
#19555=CARTESIAN_POINT('Ctrl Pts',(5.4034821510481,-2.41045871273593,34.3197571654261));
#19556=CARTESIAN_POINT('Ctrl Pts',(5.47086039871731,-2.25941810095286,34.327545276819));
#19557=CARTESIAN_POINT('Ctrl Pts',(5.53191377384975,-2.10552367300649,34.335333388212));
#19558=CARTESIAN_POINT('Ctrl Pts',(5.58641836117397,-1.94932307646484,34.3431214996049));
#19559=CARTESIAN_POINT('Ctrl Pts',(5.64091224747261,-1.79315314718736,34.3509080819379));
#19560=CARTESIAN_POINT('Ctrl Pts',(5.68885980619092,-1.63467825424026,34.358694664271));
#19561=CARTESIAN_POINT('Ctrl Pts',(5.73008616510002,-1.47446366622898,34.366481246604));
#19562=CARTESIAN_POINT('Ctrl Pts',(5.771314095961,-1.31424296927113,34.3742681258377));
#19563=CARTESIAN_POINT('Ctrl Pts',(5.80582023075301,-1.15228275296601,34.3820550050714));
#19564=CARTESIAN_POINT('Ctrl Pts',(5.83348006089518,-0.989161736845068,
34.389841884305));
#19565=CARTESIAN_POINT('Ctrl Pts',(5.86113806550457,-0.826051486616828,
34.3976282496092));
#19566=CARTESIAN_POINT('Ctrl Pts',(5.88195061638305,-0.661780904961187,
34.4054146149133));
#19567=CARTESIAN_POINT('Ctrl Pts',(5.89584462830319,-0.496937301285056,
34.4132009802175));
#19568=CARTESIAN_POINT('Ctrl Pts',(5.9097422885087,-0.33205041302612,34.4209893900631));
#19569=CARTESIAN_POINT('Ctrl Pts',(5.91671775088616,-0.166590520534307,
34.4287777999086));
#19570=CARTESIAN_POINT('Ctrl Pts',(5.91674988836775,-0.0011493477552802,
34.4365662097542));
#19571=CARTESIAN_POINT('Ctrl Pts',(5.91678033696172,0.155597567330028,34.4439453234065));
#19572=CARTESIAN_POINT('Ctrl Pts',(5.9105784611958,0.312327419526829,34.4513244370589));
#19573=CARTESIAN_POINT('Ctrl Pts',(5.89816946935658,0.468537590007321,34.4587035507112));
#19574=CARTESIAN_POINT('Ctrl Pts',(5.88507269171204,0.63340592863688,34.4664916621042));
#19575=CARTESIAN_POINT('Ctrl Pts',(5.86505653282944,0.797754226321862,34.4742797734972));
#19576=CARTESIAN_POINT('Ctrl Pts',(5.83818638150636,0.96099445226995,34.4820678848902));
#19577=CARTESIAN_POINT('Ctrl Pts',(5.81132150566908,1.12420262884537,34.4898544672233));
#19578=CARTESIAN_POINT('Ctrl Pts',(5.77760537425251,1.28630285267095,34.4976410495564));
#19579=CARTESIAN_POINT('Ctrl Pts',(5.73715487239508,1.4467150834402,34.5054276318894));
#19580=CARTESIAN_POINT('Ctrl Pts',(5.69670282816903,1.60713343069206,34.5132145111232));
#19581=CARTESIAN_POINT('Ctrl Pts',(5.64951597398198,1.76586334531487,34.5210013903569));
#19582=CARTESIAN_POINT('Ctrl Pts',(5.59576185583864,1.92233707118217,34.5287882695907));
#19583=CARTESIAN_POINT('Ctrl Pts',(5.54201128543601,2.07880046987409,34.5365746348949));
#19584=CARTESIAN_POINT('Ctrl Pts',(5.48169442238196,2.23300767561758,34.5443610001991));
#19585=CARTESIAN_POINT('Ctrl Pts',(5.41502807840099,2.38440799206614,34.5521473655033));
#19586=CARTESIAN_POINT('Ctrl Pts',(5.34834422919189,2.53584806316329,34.5599357753489));
#19587=CARTESIAN_POINT('Ctrl Pts',(5.27530769462908,2.68447947881351,34.5677241851945));
#19588=CARTESIAN_POINT('Ctrl Pts',(5.19618302415405,2.82977252477885,34.5755125950401));
#19589=CARTESIAN_POINT('Ctrl Pts',(5.121216510104,2.9674301365748,34.5828917086922));
#19590=CARTESIAN_POINT('Ctrl Pts',(5.04078541325933,3.10209100131029,34.5902708223443));
#19591=CARTESIAN_POINT('Ctrl Pts',(4.95515234016332,3.23332581845288,34.5976499359964));
#19592=CARTESIAN_POINT('Ctrl Pts',(4.8647729336875,3.37183450970365,34.6054380473894));
#19593=CARTESIAN_POINT('Ctrl Pts',(4.76856626652781,3.50657606514283,34.6132261587823));
#19594=CARTESIAN_POINT('Ctrl Pts',(4.66687109274718,3.63706540581562,34.6210142701753));
#19595=CARTESIAN_POINT('Ctrl Pts',(4.56519588504112,3.76752912718114,34.6288008525083));
#19596=CARTESIAN_POINT('Ctrl Pts',(4.4580345170868,3.89374204767642,34.6365874348414));
#19597=CARTESIAN_POINT('Ctrl Pts',(4.34576714012937,4.01525074264009,34.6443740171744));
#19598=CARTESIAN_POINT('Ctrl Pts',(4.23349548244188,4.13676407070322,34.6521608964081));
#19599=CARTESIAN_POINT('Ctrl Pts',(4.1161176401057,4.25357257695394,34.6599477756418));
#19600=CARTESIAN_POINT('Ctrl Pts',(3.99405237364415,4.36525786169471,34.6677346548755));
#19601=CARTESIAN_POINT('Ctrl Pts',(3.8719951634196,4.47693577527128,34.6755210201797));
#19602=CARTESIAN_POINT('Ctrl Pts',(3.74525138400069,4.58349092836249,34.6833073854839));
#19603=CARTESIAN_POINT('Ctrl Pts',(3.61427489526354,4.68454347231058,34.691093750788));
#19604=CARTESIAN_POINT('Ctrl Pts',(3.4832640147602,4.78562255060464,34.6988821606336));
#19605=CARTESIAN_POINT('Ctrl Pts',(3.34801845604771,4.88119593574642,34.7066705704792));
#19606=CARTESIAN_POINT('Ctrl Pts',(3.20902396000049,4.97092504335388,34.7144589803248));
#19607=CARTESIAN_POINT('Ctrl Pts',(3.0773338969834,5.05593871059491,34.721838093977));
#19608=CARTESIAN_POINT('Ctrl Pts',(2.94227900854711,5.13570641672617,34.7292172076293));
#19609=CARTESIAN_POINT('Ctrl Pts',(2.80429528800515,5.20997682338147,34.7365963212815));
#19610=CARTESIAN_POINT('Ctrl Pts',(2.65866362590547,5.28836377166456,34.7443844326745));
#19611=CARTESIAN_POINT('Ctrl Pts',(2.50971724379881,5.36065474499884,34.7521725440674));
#19612=CARTESIAN_POINT('Ctrl Pts',(2.35798568823811,5.42658585637086,34.7599606554604));
#19613=CARTESIAN_POINT('Ctrl Pts',(2.20628392252322,5.49250402331854,34.7677472377935));
#19614=CARTESIAN_POINT('Ctrl Pts',(2.0517983672999,5.55206469246588,34.7755338201266));
#19615=CARTESIAN_POINT('Ctrl Pts',(1.8950797764015,5.60505157902887,34.7833204024596));
#19616=CARTESIAN_POINT('Ctrl Pts',(1.73835520985823,5.65804048597001,34.7911072816934));
#19617=CARTESIAN_POINT('Ctrl Pts',(1.57939773868323,5.70445500268399,34.7988941609271));
#19618=CARTESIAN_POINT('Ctrl Pts',(1.41877526322053,5.74412807264719,34.8066810401608));
#19619=CARTESIAN_POINT('Ctrl Pts',(1.25816338874814,5.78379852421076,34.814467405465));
#19620=CARTESIAN_POINT('Ctrl Pts',(1.09588704015207,5.81672834288891,34.8222537707692));
#19621=CARTESIAN_POINT('Ctrl Pts',(0.932526495142294,5.84280111747419,34.8300401360734));
#19622=CARTESIAN_POINT('Ctrl Pts',(0.769123054970881,5.86888073824059,34.837828545919));
#19623=CARTESIAN_POINT('Ctrl Pts',(0.604635164956452,5.88809966478843,34.8456169557646));
#19624=CARTESIAN_POINT('Ctrl Pts',(0.439651355956734,5.90039297400651,34.8534053656102));
#19625=CARTESIAN_POINT('Ctrl Pts',(0.283337769293297,5.91204024574482,34.8607844792623));
#19626=CARTESIAN_POINT('Ctrl Pts',(0.126579305409158,5.91747106814903,34.8681635929145));
#19627=CARTESIAN_POINT('Ctrl Pts',(-0.0301209308773817,5.91667332983857,
34.8755427065666));
#19628=CARTESIAN_POINT('Ctrl Pts',(-0.195506497902827,5.91583137576155,
34.8833308179596));
#19629=CARTESIAN_POINT('Ctrl Pts',(-0.36088626684752,5.90805052799148,34.8911189293525));
#19630=CARTESIAN_POINT('Ctrl Pts',(-0.525668977942791,5.89335241506297,
34.8989070407455));
#19631=CARTESIAN_POINT('Ctrl Pts',(-0.690419336825323,5.87865718785271,
34.9066936230786));
#19632=CARTESIAN_POINT('Ctrl Pts',(-0.854572553682613,5.85704743363695,
34.9144802054116));
#19633=CARTESIAN_POINT('Ctrl Pts',(-1.01754152073414,5.8285967278653,34.9222667877447));
#19634=CARTESIAN_POINT('Ctrl Pts',(-1.18051670175601,5.80014493727459,34.9300536669784));
#19635=CARTESIAN_POINT('Ctrl Pts',(-1.3423072271822,5.76485172423875,34.9378405462121));
#19636=CARTESIAN_POINT('Ctrl Pts',(-1.50233448502554,5.72284209616193,34.9456274254458));
#19637=CARTESIAN_POINT('Ctrl Pts',(-1.66235118116235,5.68083524069628,34.95341379075));
#19638=CARTESIAN_POINT('Ctrl Pts',(-1.82060453354907,5.63211293851259,34.9612001560542));
#19639=CARTESIAN_POINT('Ctrl Pts',(-1.9765292918561,5.57685059159153,34.9689865213583));
#19640=CARTESIAN_POINT('Ctrl Pts',(-2.13249499283837,5.52157373390036,34.9767749312039));
#19641=CARTESIAN_POINT('Ctrl Pts',(-2.28613057593417,5.45975350496361,34.9845633410495));
#19642=CARTESIAN_POINT('Ctrl Pts',(-2.4368881772574,5.39161446823149,34.9923517508951));
#19643=CARTESIAN_POINT('Ctrl Pts',(-2.5797231713256,5.32705627135107,34.9997308645473));
#19644=CARTESIAN_POINT('Ctrl Pts',(-2.71997465365962,5.2568264234601,35.0071099781995));
#19645=CARTESIAN_POINT('Ctrl Pts',(-2.85719504192284,5.18115499236527,35.0144890918517));
#19646=CARTESIAN_POINT('Ctrl Pts',(-3.00202106297927,5.10128936589519,35.0222772032446));
#19647=CARTESIAN_POINT('Ctrl Pts',(-3.14352218117468,5.015333312489,35.0300653146375));
#19648=CARTESIAN_POINT('Ctrl Pts',(-3.28118954566347,4.92358870417998,35.0378534260304));
#19649=CARTESIAN_POINT('Ctrl Pts',(-3.41882988156519,4.83186210832544,35.0456400083634));
#19650=CARTESIAN_POINT('Ctrl Pts',(-3.55263769987251,4.73434940227533,35.0534265906964));
#19651=CARTESIAN_POINT('Ctrl Pts',(-3.68213264893139,4.63139608737728,35.0612131730294));
#19652=CARTESIAN_POINT('Ctrl Pts',(-3.81163253560394,4.52843884689216,35.069000052263));
#19653=CARTESIAN_POINT('Ctrl Pts',(-3.93681897140464,4.42004077820467,35.0767869314966));
#19654=CARTESIAN_POINT('Ctrl Pts',(-4.05724367189022,4.30658848154856,35.0845738107303));
#19655=CARTESIAN_POINT('Ctrl Pts',(-4.17766042441529,4.19314367267836,35.0923601760344));
#19656=CARTESIAN_POINT('Ctrl Pts',(-4.29331583802088,4.07464552258709,35.1001465413386));
#19657=CARTESIAN_POINT('Ctrl Pts',(-4.40379747198279,3.95151849144832,35.1079329066427));
#19658=CARTESIAN_POINT('Ctrl Pts',(-4.51430811617819,3.82835912965155,35.1157213164882));
#19659=CARTESIAN_POINT('Ctrl Pts',(-4.61964205112156,3.70056869476739,35.1235097263338));
#19660=CARTESIAN_POINT('Ctrl Pts',(-4.71942562410225,3.56860649849029,35.1312981361793));
#19661=CARTESIAN_POINT('Ctrl Pts',(-4.8139653748704,3.44357917411025,35.1386772498318));
#19662=CARTESIAN_POINT('Ctrl Pts',(-4.90352296716482,3.31480748663149,35.1460563634843));
#19663=CARTESIAN_POINT('Ctrl Pts',(-4.9878154412707,3.18270760302003,35.1534354771368));
#19664=CARTESIAN_POINT('Ctrl Pts',(-5.07677994417001,3.04328589778231,35.1612235885298));
#19665=CARTESIAN_POINT('Ctrl Pts',(-5.15991089895353,2.90010680040592,35.1690116999229));
#19666=CARTESIAN_POINT('Ctrl Pts',(-5.2369058983043,2.75367884380253,35.1767998113159));
#19667=CARTESIAN_POINT('Ctrl Pts',(-5.3138857810293,2.60727963577555,35.1845863936491));
#19668=CARTESIAN_POINT('Ctrl Pts',(-5.38473196341406,2.45763312387514,35.1923729759822));
#19669=CARTESIAN_POINT('Ctrl Pts',(-5.44918793773478,2.3052725178915,35.2001595583154));
#19670=CARTESIAN_POINT('Ctrl Pts',(-5.51364636974735,2.15290610243209,35.2079464375492));
#19671=CARTESIAN_POINT('Ctrl Pts',(-5.57171397801221,1.99782567853851,35.2157333167829));
#19672=CARTESIAN_POINT('Ctrl Pts',(-5.62318207691178,1.8405852037866,35.2235201960167));
#19673=CARTESIAN_POINT('Ctrl Pts',(-5.67464677894655,1.68335510681517,35.231306561321));
#19674=CARTESIAN_POINT('Ctrl Pts',(-5.7195127439514,1.52396554800902,35.2390929266252));
#19675=CARTESIAN_POINT('Ctrl Pts',(-5.75762087502688,1.36298658172217,35.2468792919295));
#19676=CARTESIAN_POINT('Ctrl Pts',(-5.79573901252374,1.20196534562771,35.2546677017752));
#19677=CARTESIAN_POINT('Ctrl Pts',(-5.82709569478609,1.03935417880022,35.2624561116208));
#19678=CARTESIAN_POINT('Ctrl Pts',(-5.85158255975117,0.875735181956287,
35.2702445214665));
#19679=CARTESIAN_POINT('Ctrl Pts',(-5.87478259199587,0.720714683904022,
35.2776236351184));
#19680=CARTESIAN_POINT('Ctrl Pts',(-5.89181624181401,0.564789815447571,
35.2850027487702));
#19681=CARTESIAN_POINT('Ctrl Pts',(-5.90263414477321,0.408461400205068,
35.292381862422));
#19682=CARTESIAN_POINT('Ctrl Pts',(-5.9120376370948,0.272572489209566,35.2987961775464));
#19683=CARTESIAN_POINT('Ctrl Pts',(-5.91674717417702,0.1363570960496,35.3052104926708));
#19684=CARTESIAN_POINT('Ctrl Pts',(-5.91674999872832,0.00012267210750124,
35.3116248077951));
#19685=CARTESIAN_POINT('Origin',(0.,0.,0.));
#19686=CARTESIAN_POINT('',(-5.91674999982786,-4.51337720214345E-5,37.3133751922485));
#19687=CARTESIAN_POINT('',(-5.91674999805201,-0.000151827279522968,37.0616248082411));
#19688=CARTESIAN_POINT('',(-5.91675,-7.2459289488551E-16,0.));
#19689=CARTESIAN_POINT('Ctrl Pts',(-5.91674999982786,-4.51328457496523E-5,
37.3133751922049));
#19690=CARTESIAN_POINT('Ctrl Pts',(-5.9167512716958,0.166692072992805,37.3055286593146));
#19691=CARTESIAN_POINT('Ctrl Pts',(-5.90970008426505,0.333421001495371,
37.2976821264244));
#19692=CARTESIAN_POINT('Ctrl Pts',(-5.89562456490874,0.499541341777265,
37.2898355935341));
#19693=CARTESIAN_POINT('Ctrl Pts',(-5.88154835837704,0.665669792154845,
37.2819886775713));
#19694=CARTESIAN_POINT('Ctrl Pts',(-5.86044716515415,0.831189287417103,
37.2741417616085));
#19695=CARTESIAN_POINT('Ctrl Pts',(-5.83240101010933,0.995504404699285,
37.2662948456457));
#19696=CARTESIAN_POINT('Ctrl Pts',(-5.80434815606936,1.1598587696492,37.2584460553992));
#19697=CARTESIAN_POINT('Ctrl Pts',(-5.76934707958976,1.32300787753653,37.2505972651527));
#19698=CARTESIAN_POINT('Ctrl Pts',(-5.72752911738174,1.48436544423679,37.2427484749062));
#19699=CARTESIAN_POINT('Ctrl Pts',(-5.71723917772028,1.52406990465518,37.2408171618104));
#19700=CARTESIAN_POINT('Ctrl Pts',(-5.70653672951455,1.56366594835795,37.2388858487146));
#19701=CARTESIAN_POINT('Ctrl Pts',(-5.69542419792215,1.60314496169961,37.2369545356188));
#19702=CARTESIAN_POINT('Ctrl Pts',(-5.65061315765045,1.76234321837312,37.2291665578575));
#19703=CARTESIAN_POINT('Ctrl Pts',(-5.59911506889175,1.91968993099315,37.2213785800963));
#19704=CARTESIAN_POINT('Ctrl Pts',(-5.5411080665506,2.07462091894106,37.213590602335));
#19705=CARTESIAN_POINT('Ctrl Pts',(-5.48311246888355,2.22952144612814,37.2058041557569));
#19706=CARTESIAN_POINT('Ctrl Pts',(-5.41861062300551,2.38200689723374,37.1980177091788));
#19707=CARTESIAN_POINT('Ctrl Pts',(-5.34782963433365,2.53153091323074,37.1902312626008));
#19708=CARTESIAN_POINT('Ctrl Pts',(-5.2770459455265,2.68106063323216,37.1824445189873));
#19709=CARTESIAN_POINT('Ctrl Pts',(-5.19998276775482,2.82762840156007,37.1746577753738));
#19710=CARTESIAN_POINT('Ctrl Pts',(-5.11691452508468,2.97070973093593,37.1668710317604));
#19711=CARTESIAN_POINT('Ctrl Pts',(-5.03385177675738,3.1137815965522,37.1590848031817));
#19712=CARTESIAN_POINT('Ctrl Pts',(-4.94478491892114,3.25336720836627,37.1512985746031));
#19713=CARTESIAN_POINT('Ctrl Pts',(-4.85003339957065,3.38896836597056,37.1435123460245));
#19714=CARTESIAN_POINT('Ctrl Pts',(-4.75525693722305,3.52460522009249,37.1357240677492));
#19715=CARTESIAN_POINT('Ctrl Pts',(-4.65479300465449,3.65625526086087,37.1279357894738));
#19716=CARTESIAN_POINT('Ctrl Pts',(-4.54900381506683,3.78345012561384,37.1201475111985));
#19717=CARTESIAN_POINT('Ctrl Pts',(-4.44842993009576,3.90437440669057,37.1127431875012));
#19718=CARTESIAN_POINT('Ctrl Pts',(-4.3430433686534,4.02127199945382,37.1053388638038));
#19719=CARTESIAN_POINT('Ctrl Pts',(-4.23318854821258,4.13376889506197,37.0979345401065));
#19720=CARTESIAN_POINT('Ctrl Pts',(-4.11764161461318,4.25209480260808,37.0901465623448));
#19721=CARTESIAN_POINT('Ctrl Pts',(-3.99710975048733,4.36559418961599,37.0823585845831));
#19722=CARTESIAN_POINT('Ctrl Pts',(-3.8720194124591,4.47385697491995,37.0745706068215));
#19723=CARTESIAN_POINT('Ctrl Pts',(-3.7469536682634,4.58209847483247,37.066784160243));
#19724=CARTESIAN_POINT('Ctrl Pts',(-3.61733147989254,4.68510521832739,37.0589977136645));
#19725=CARTESIAN_POINT('Ctrl Pts',(-3.48361376928839,4.7825062121156,37.051211267086));
#19726=CARTESIAN_POINT('Ctrl Pts',(-3.34989095765504,4.87991092153214,37.0434245234721));
#19727=CARTESIAN_POINT('Ctrl Pts',(-3.21207256711454,4.97170926199926,37.0356377798582));
#19728=CARTESIAN_POINT('Ctrl Pts',(-3.07065059591841,5.05757209343435,37.0278510362443));
#19729=CARTESIAN_POINT('Ctrl Pts',(-2.92923797872759,5.14342924568554,37.0200648076653));
#19730=CARTESIAN_POINT('Ctrl Pts',(-2.78422253108445,5.22335150877934,37.0122785790863));
#19731=CARTESIAN_POINT('Ctrl Pts',(-2.63612319941929,5.29705437389342,37.0044923505072));
#19732=CARTESIAN_POINT('Ctrl Pts',(-2.48798488113741,5.37077664102182,36.9967040722315));
#19733=CARTESIAN_POINT('Ctrl Pts',(-2.33676134204432,5.43827609441476,36.9889157939557));
#19734=CARTESIAN_POINT('Ctrl Pts',(-2.18299479391218,5.49931489298915,36.98112751568));
#19735=CARTESIAN_POINT('Ctrl Pts',(-2.03680878776444,5.55734453787641,36.9737231919846));
#19736=CARTESIAN_POINT('Ctrl Pts',(-1.88832471336697,5.60953509414731,36.9663188682892));
#19737=CARTESIAN_POINT('Ctrl Pts',(-1.73802399381556,5.65572304479466,36.9589145445938));
#19738=CARTESIAN_POINT('Ctrl Pts',(-1.57993546209493,5.70430421807726,36.9511265668323));
#19739=CARTESIAN_POINT('Ctrl Pts',(-1.41978047724363,5.74626160057876,36.9433385890709));
#19740=CARTESIAN_POINT('Ctrl Pts',(-1.25812975907609,5.78143927338402,36.9355506113095));
#19741=CARTESIAN_POINT('Ctrl Pts',(-1.09651082282591,5.81661002995716,36.9277641647313));
#19742=CARTESIAN_POINT('Ctrl Pts',(-0.933397052074306,5.84500366855293,
36.9199777181531));
#19743=CARTESIAN_POINT('Ctrl Pts',(-0.769370716969568,5.86651508669071,
36.9121912715749));
#19744=CARTESIAN_POINT('Ctrl Pts',(-0.605338124629431,5.88802732544067,
36.9044045279612));
#19745=CARTESIAN_POINT('Ctrl Pts',(-0.44039321458797,5.90265677291185,36.8966177843476));
#19746=CARTESIAN_POINT('Ctrl Pts',(-0.275125508117482,5.91034994880025,
36.888831040734));
#19747=CARTESIAN_POINT('Ctrl Pts',(-0.109868732869458,5.91804261584261,
36.8810448121553));
#19748=CARTESIAN_POINT('Ctrl Pts',(0.0557104768455538,5.91879991464769,
36.8732585835765));
#19749=CARTESIAN_POINT('Ctrl Pts',(0.221020302878597,5.9126204502078,36.8654723549977));
#19750=CARTESIAN_POINT('Ctrl Pts',(0.386373646129538,5.90643935904609,36.8576840767222));
#19751=CARTESIAN_POINT('Ctrl Pts',(0.551457144383887,5.893317865741,36.8498957984468));
#19752=CARTESIAN_POINT('Ctrl Pts',(0.715680890929399,5.87330668574854,36.8421075201713));
#19753=CARTESIAN_POINT('Ctrl Pts',(0.871808565761582,5.85428203755611,36.8347031964746));
#19754=CARTESIAN_POINT('Ctrl Pts',(1.02715895519726,5.82903068068344,36.827298872778));
#19755=CARTESIAN_POINT('Ctrl Pts',(1.18123110126656,5.79763948930085,36.8198945490814));
#19756=CARTESIAN_POINT('Ctrl Pts',(1.34328647545535,5.76462176743793,36.8121065713198));
#19757=CARTESIAN_POINT('Ctrl Pts',(1.50398559573187,5.72479923784935,36.8043185935582));
#19758=CARTESIAN_POINT('Ctrl Pts',(1.66275273889179,5.67830818922396,36.7965306157965));
#19759=CARTESIAN_POINT('Ctrl Pts',(1.82148866706992,5.63182628113739,36.7887441692181));
#19760=CARTESIAN_POINT('Ctrl Pts',(1.97829306954646,5.578678559767,36.7809577226397));
#19761=CARTESIAN_POINT('Ctrl Pts',(2.13260440613291,5.51905145921312,36.7731712760613));
#19762=CARTESIAN_POINT('Ctrl Pts',(2.28692162934912,5.45942208401973,36.7653845324475));
#19763=CARTESIAN_POINT('Ctrl Pts',(2.43874529688261,5.39331294652846,36.7575977888337));
#19764=CARTESIAN_POINT('Ctrl Pts',(2.5875322119337,5.32095927579845,36.7498110452199));
#19765=CARTESIAN_POINT('Ctrl Pts',(2.73630928584353,5.24861039072242,36.742024816641));
#19766=CARTESIAN_POINT('Ctrl Pts',(2.88204972187158,5.1700179388011,36.734238588062));
#19767=CARTESIAN_POINT('Ctrl Pts',(3.02423323809834,5.08546397923348,36.7264523594831));
#19768=CARTESIAN_POINT('Ctrl Pts',(3.16645418362486,5.00088776113982,36.7186640812074));
#19769=CARTESIAN_POINT('Ctrl Pts',(3.30511606249578,4.91034706127661,36.7108758029317));
#19770=CARTESIAN_POINT('Ctrl Pts',(3.43972521460233,4.81416877669748,36.7030875246561));
#19771=CARTESIAN_POINT('Ctrl Pts',(3.56769826581228,4.72273198844711,36.6956832009603));
#19772=CARTESIAN_POINT('Ctrl Pts',(3.69200834128986,4.62620023382378,36.6882788772645));
#19773=CARTESIAN_POINT('Ctrl Pts',(3.81225718559272,4.52488958024355,36.6808745535688));
#19774=CARTESIAN_POINT('Ctrl Pts',(3.93873670806515,4.41832952837376,36.6730865758073));
#19775=CARTESIAN_POINT('Ctrl Pts',(4.06076820543666,4.30644407458904,36.6652985980459));
#19776=CARTESIAN_POINT('Ctrl Pts',(4.17791143177724,4.18962845974736,36.6575106202844));
#19777=CARTESIAN_POINT('Ctrl Pts',(4.29503162675513,4.07283581185714,36.6497241737062));
#19778=CARTESIAN_POINT('Ctrl Pts',(4.40726524219837,3.95111516247358,36.6419377271279));
#19779=CARTESIAN_POINT('Ctrl Pts',(4.51420848778309,3.82489899099664,36.6341512805497));
#19780=CARTESIAN_POINT('Ctrl Pts',(4.62115581301153,3.69867800465731,36.626364536936));
#19781=CARTESIAN_POINT('Ctrl Pts',(4.72281215496097,3.56796139429931,36.6185777933224));
#19782=CARTESIAN_POINT('Ctrl Pts',(4.81881318528843,3.43321570073748,36.6107910497088));
#19783=CARTESIAN_POINT('Ctrl Pts',(4.91480786586589,3.29847891959528,36.60300482113));
#19784=CARTESIAN_POINT('Ctrl Pts',(5.00514779802127,3.15971384888359,36.5952185925512));
#19785=CARTESIAN_POINT('Ctrl Pts',(5.08951118865056,3.01741717750475,36.5874323639724));
#19786=CARTESIAN_POINT('Ctrl Pts',(5.17389678763945,2.87508304703822,36.5796440856969));
#19787=CARTESIAN_POINT('Ctrl Pts',(5.25230253655634,2.72921573226415,36.5718558074214));
#19788=CARTESIAN_POINT('Ctrl Pts',(5.32445147856587,2.58033854656665,36.5640675291459));
#19789=CARTESIAN_POINT('Ctrl Pts',(5.39304354758304,2.43880086199333,36.5566632054494));
#19790=CARTESIAN_POINT('Ctrl Pts',(5.4559807433462,2.29454316233653,36.5492588817529));
#19791=CARTESIAN_POINT('Ctrl Pts',(5.51306469017522,2.14803358550169,36.5418545580564));
#19792=CARTESIAN_POINT('Ctrl Pts',(5.57310643425227,1.99393263408177,36.5340665802948));
#19793=CARTESIAN_POINT('Ctrl Pts',(5.62669373263113,1.83728512349577,36.5262786025332));
#19794=CARTESIAN_POINT('Ctrl Pts',(5.67362923987644,1.67864880511651,36.5184906247716));
#19795=CARTESIAN_POINT('Ctrl Pts',(5.72055551919885,1.52004367599674,36.5107041781931));
#19796=CARTESIAN_POINT('Ctrl Pts',(5.76083252622775,1.35945082550867,36.5029177316147));
#19797=CARTESIAN_POINT('Ctrl Pts',(5.79431274829024,1.19744325022155,36.4951312850362));
#19798=CARTESIAN_POINT('Ctrl Pts',(5.82779424754762,1.03542949471123,36.4873445414224));
#19799=CARTESIAN_POINT('Ctrl Pts',(5.8544783744694,0.872001218536192,36.4795577978086));
#19800=CARTESIAN_POINT('Ctrl Pts',(5.87426856794425,0.70774243490282,36.4717710541949));
#19801=CARTESIAN_POINT('Ctrl Pts',(5.89405745244584,0.543494515759324,36.4639848256159));
#19802=CARTESIAN_POINT('Ctrl Pts',(5.90695327787479,0.378416516380153,36.456198597037));
#19803=CARTESIAN_POINT('Ctrl Pts',(5.9129112598088,0.213098559653396,36.448412368458));
#19804=CARTESIAN_POINT('Ctrl Pts',(5.91887081016015,0.0477370835681996,
36.4406240901824));
#19805=CARTESIAN_POINT('Ctrl Pts',(5.91788885408841,-0.117864156602236,
36.4328358119067));
#19806=CARTESIAN_POINT('Ctrl Pts',(5.90997271752099,-0.283113123428823,
36.425047533631));
#19807=CARTESIAN_POINT('Ctrl Pts',(5.90244683882346,-0.440215476153025,
36.4176432099352));
#19808=CARTESIAN_POINT('Ctrl Pts',(5.88865401970231,-0.596999189135951,
36.4102388862395));
#19809=CARTESIAN_POINT('Ctrl Pts',(5.86864416935359,-0.75295828304897,36.4028345625437));
#19810=CARTESIAN_POINT('Ctrl Pts',(5.84759751122135,-0.916998377052583,
36.3950465847823));
#19811=CARTESIAN_POINT('Ctrl Pts',(5.81966491865678,-1.08018480844891,36.3872586070208));
#19812=CARTESIAN_POINT('Ctrl Pts',(5.78494010044588,-1.24193341075646,36.3794706292594));
#19813=CARTESIAN_POINT('Ctrl Pts',(5.75022210943202,-1.40365021190179,36.3716841826812));
#19814=CARTESIAN_POINT('Ctrl Pts',(5.7087146243404,-1.56392943576761,36.3638977361029));
#19815=CARTESIAN_POINT('Ctrl Pts',(5.66056240431804,-1.72219738396072,36.3561112895247));
#19816=CARTESIAN_POINT('Ctrl Pts',(5.61240834739688,-1.88047136971978,36.3483245459111));
#19817=CARTESIAN_POINT('Ctrl Pts',(5.55760913754932,-2.03673361942248,36.3405378022974));
#19818=CARTESIAN_POINT('Ctrl Pts',(5.49635954251166,-2.1904251509561,36.3327510586838));
#19819=CARTESIAN_POINT('Ctrl Pts',(5.43511399867645,-2.3441065169448,36.324964830105));
#19820=CARTESIAN_POINT('Ctrl Pts',(5.36741904184612,-2.49521720819887,36.3171786015262));
#19821=CARTESIAN_POINT('Ctrl Pts',(5.29351782400595,-2.64321766213668,36.3093923729474));
#19822=CARTESIAN_POINT('Ctrl Pts',(5.21959715193585,-2.79125707666196,36.3016040946719));
#19823=CARTESIAN_POINT('Ctrl Pts',(5.13946709532679,-2.93618433086334,36.2938158163964));
#19824=CARTESIAN_POINT('Ctrl Pts',(5.0534174752892,-3.07748312472087,36.2860275381209));
#19825=CARTESIAN_POINT('Ctrl Pts',(4.9716100182128,-3.21181602483592,36.2786232144244));
#19826=CARTESIAN_POINT('Ctrl Pts',(4.88445273274803,-3.34286938080751,36.2712188907279));
#19827=CARTESIAN_POINT('Ctrl Pts',(4.79223163475909,-3.47022283453299,36.2638145670314));
#19828=CARTESIAN_POINT('Ctrl Pts',(4.69523211262594,-3.60417509082536,36.2560265892698));
#19829=CARTESIAN_POINT('Ctrl Pts',(4.5925953855893,-3.73408176264429,36.2482386115083));
#19830=CARTESIAN_POINT('Ctrl Pts',(4.48468335102875,-3.85947480928501,36.2404506337468));
#19831=CARTESIAN_POINT('Ctrl Pts',(4.37679253289999,-3.98484320257699,36.2326641871685));
#19832=CARTESIAN_POINT('Ctrl Pts',(4.26362868502172,-4.10569949929104,36.2248777405902));
#19833=CARTESIAN_POINT('Ctrl Pts',(4.14559351607236,-4.22160928580545,36.2170912940119));
#19834=CARTESIAN_POINT('Ctrl Pts',(4.02755384434665,-4.33752349401765,36.2093045503982));
#19835=CARTESIAN_POINT('Ctrl Pts',(3.90464270492175,-4.44849058773415,36.2015178067844));
#19836=CARTESIAN_POINT('Ctrl Pts',(3.77729866963234,-4.55411301165153,36.1937310631707));
#19837=CARTESIAN_POINT('Ctrl Pts',(3.64996305719867,-4.65972844943534,36.1859448345919));
#19838=CARTESIAN_POINT('Ctrl Pts',(3.51819538169348,-4.75999972091334,36.178158606013));
#19839=CARTESIAN_POINT('Ctrl Pts',(3.38246740065049,-4.85456948101855,36.1703723774342));
#19840=CARTESIAN_POINT('Ctrl Pts',(3.24670368970339,-4.94916413627386,36.1625840991586));
#19841=CARTESIAN_POINT('Ctrl Pts',(3.10697785125219,-5.03805409663128,36.154795820883));
#19842=CARTESIAN_POINT('Ctrl Pts',(2.9637914831239,-5.12092478045345,36.1470075426074));
#19843=CARTESIAN_POINT('Ctrl Pts',(2.82766406432971,-5.19971001978793,36.1396032189111));
#19844=CARTESIAN_POINT('Ctrl Pts',(2.68840932636022,-5.27305504328633,36.1321988952149));
#19845=CARTESIAN_POINT('Ctrl Pts',(2.54647960178911,-5.34072768451753,36.1247945715187));
#19846=CARTESIAN_POINT('Ctrl Pts',(2.397195807073,-5.41190677481721,36.1170065937571));
#19847=CARTESIAN_POINT('Ctrl Pts',(2.24489905612588,-5.47683551091822,36.1092186159954));
#19848=CARTESIAN_POINT('Ctrl Pts',(2.09013112931874,-5.53527618324079,36.1014306382338));
#19849=CARTESIAN_POINT('Ctrl Pts',(1.93539363121317,-5.59370536562605,36.0936441916553));
#19850=CARTESIAN_POINT('Ctrl Pts',(1.77818622543415,-5.64564891663448,36.0858577450769));
#19851=CARTESIAN_POINT('Ctrl Pts',(1.61906955034184,-5.69091770751044,36.0780712984984));
#19852=CARTESIAN_POINT('Ctrl Pts',(1.45994680530705,-5.73618822528873,36.0702845548846));
#19853=CARTESIAN_POINT('Ctrl Pts',(1.29891495147683,-5.77478338217882,36.0624978112708));
#19854=CARTESIAN_POINT('Ctrl Pts',(1.13654935005534,-5.80656405608246,36.054711067657));
#19855=CARTESIAN_POINT('Ctrl Pts',(0.974194487903553,-5.8383426279323,36.046924839078));
#19856=CARTESIAN_POINT('Ctrl Pts',(0.810506368343906,-5.86330755749171,
36.039138610499));
#19857=CARTESIAN_POINT('Ctrl Pts',(0.646070242176841,-5.88137091201308,
36.03135238192));
#19858=CARTESIAN_POINT('Ctrl Pts',(0.481590828790343,-5.89943902164763,
36.0235641036443));
#19859=CARTESIAN_POINT('Ctrl Pts',(0.316363332966109,-5.91060188900507,
36.0157758253686));
#19860=CARTESIAN_POINT('Ctrl Pts',(0.150978735716734,-5.9148234110463,36.0079875470929));
#19861=CARTESIAN_POINT('Ctrl Pts',(-0.00625256097642329,-5.91883681613723,
36.0005832233973));
#19862=CARTESIAN_POINT('Ctrl Pts',(-0.16362557892651,-5.91657678607358,
35.9931788997018));
#19863=CARTESIAN_POINT('Ctrl Pts',(-0.320632041300111,-5.90805599639947,
35.9857745760062));
#19864=CARTESIAN_POINT('Ctrl Pts',(-0.485773773027661,-5.89909370312061,
35.9779865982448));
#19865=CARTESIAN_POINT('Ctrl Pts',(-0.650569029001088,-5.88320141796559,
35.9701986204834));
#19866=CARTESIAN_POINT('Ctrl Pts',(-0.814428344223128,-5.86042976535219,
35.9624106427221));
#19867=CARTESIAN_POINT('Ctrl Pts',(-0.978255443297349,-5.83766258984115,
35.954624196144));
#19868=CARTESIAN_POINT('Ctrl Pts',(-1.14114665246819,-5.80801878955106,
35.9468377495659));
#19869=CARTESIAN_POINT('Ctrl Pts',(-1.30251920354592,-5.77160066938922,
35.9390513029878));
#19870=CARTESIAN_POINT('Ctrl Pts',(-1.4638979106241,-5.73518115995788,35.9312645593742));
#19871=CARTESIAN_POINT('Ctrl Pts',(-1.62375753111289,-5.69198688002801,
35.9234778157606));
#19872=CARTESIAN_POINT('Ctrl Pts',(-1.78152630677224,-5.64217108751396,
35.9156910721471));
#19873=CARTESIAN_POINT('Ctrl Pts',(-1.93928464720688,-5.59235858994206,
35.9079048435684));
#19874=CARTESIAN_POINT('Ctrl Pts',(-2.09495211484654,-5.53592555254885,
35.9001186149897));
#19875=CARTESIAN_POINT('Ctrl Pts',(-2.24797277109128,-5.47307491113836,
35.892332386411));
#19876=CARTESIAN_POINT('Ctrl Pts',(-2.40103370947464,-5.41020772452207,
35.8845441081356));
#19877=CARTESIAN_POINT('Ctrl Pts',(-2.55144614765425,-5.34091967776843,
35.8767558298601));
#19878=CARTESIAN_POINT('Ctrl Pts',(-2.69867392511282,-5.26546195584169,
35.8689675515847));
#19879=CARTESIAN_POINT('Ctrl Pts',(-2.83864351568707,-5.19372422654856,
35.8615632278877));
#19880=CARTESIAN_POINT('Ctrl Pts',(-2.97573464857824,-5.11641060674806,
35.8541589041908));
#19881=CARTESIAN_POINT('Ctrl Pts',(-3.10950712595014,-5.03377552103441,
35.8467545804938));
#19882=CARTESIAN_POINT('Ctrl Pts',(-3.25021100675418,-4.9468587091542,35.8389666027321));
#19883=CARTESIAN_POINT('Ctrl Pts',(-3.38729352243181,-4.85402323632069,
35.8311786249705));
#19884=CARTESIAN_POINT('Ctrl Pts',(-3.52026135712141,-4.75559570822181,
35.8233906472088));
#19885=CARTESIAN_POINT('Ctrl Pts',(-3.65320304919531,-4.65718753181839,
35.8156042006303));
#19886=CARTESIAN_POINT('Ctrl Pts',(-3.78203141775639,-4.55318968387259,
35.8078177540518));
#19887=CARTESIAN_POINT('Ctrl Pts',(-3.9062837644773,-4.4439709398106,35.8000313074734));
#19888=CARTESIAN_POINT('Ctrl Pts',(-4.0305408511444,-4.33474802930037,35.7922445638595));
#19889=CARTESIAN_POINT('Ctrl Pts',(-4.15022132405298,-4.2203040321326,35.7844578202457));
#19890=CARTESIAN_POINT('Ctrl Pts',(-4.26489654111093,-4.10104719018448,
35.7766710766319));
#19891=CARTESIAN_POINT('Ctrl Pts',(-4.37956417326116,-3.9817982361843,35.7688848480529));
#19892=CARTESIAN_POINT('Ctrl Pts',(-4.4892269906369,-3.85773730487219,35.7610986194739));
#19893=CARTESIAN_POINT('Ctrl Pts',(-4.59349401991493,-3.72930868278637,
35.7533123908949));
#19894=CARTESIAN_POINT('Ctrl Pts',(-4.69778849711381,-3.60084625232721,
35.7455241126192));
#19895=CARTESIAN_POINT('Ctrl Pts',(-4.79668414484876,-3.46801408061042,
35.7377358343436));
#19896=CARTESIAN_POINT('Ctrl Pts',(-4.88983045017742,-3.33128934963892,
35.7299475560679));
#19897=CARTESIAN_POINT('Ctrl Pts',(-4.97838473281677,-3.20130501555805,
35.7225432323723));
#19898=CARTESIAN_POINT('Ctrl Pts',(-5.06174274352001,-3.06780289360419,
35.7151389086767));
#19899=CARTESIAN_POINT('Ctrl Pts',(-5.13963977493379,-2.93121707596326,
35.7077345849812));
#19900=CARTESIAN_POINT('Ctrl Pts',(-5.22157303086326,-2.78755408200825,
35.6999466072197));
#19901=CARTESIAN_POINT('Ctrl Pts',(-5.2974936718184,-2.64042795449758,35.6921586294583));
#19902=CARTESIAN_POINT('Ctrl Pts',(-5.36712490374431,-2.49036158621748,
35.6843706516968));
#19903=CARTESIAN_POINT('Ctrl Pts',(-5.43674244557314,-2.34032472227175,
35.6765842051186));
#19904=CARTESIAN_POINT('Ctrl Pts',(-5.50007291124137,-2.18734906067767,
35.6687977585403));
#19905=CARTESIAN_POINT('Ctrl Pts',(-5.5568865740533,-2.03197986348443,35.661011311962));
#19906=CARTESIAN_POINT('Ctrl Pts',(-5.61370240417827,-1.8766047393069,35.6532245683484));
#19907=CARTESIAN_POINT('Ctrl Pts',(-5.6640008205388,-1.71883619556755,35.6454378247348));
#19908=CARTESIAN_POINT('Ctrl Pts',(-5.70760088899002,-1.55923784410856,
35.6376510811211));
#19909=CARTESIAN_POINT('Ctrl Pts',(-5.75119807362305,-1.39965004888596,
35.6298648525423));
#19910=CARTESIAN_POINT('Ctrl Pts',(-5.78809771283873,-1.23823299644907,
35.6220786239635));
#19911=CARTESIAN_POINT('Ctrl Pts',(-5.81816919893528,-1.07556391491199,
35.6142923953847));
#19912=CARTESIAN_POINT('Ctrl Pts',(-5.84824860124243,-0.912852011324053,
35.6065041171092));
#19913=CARTESIAN_POINT('Ctrl Pts',(-5.87149619862239,-0.748887734121178,
35.5987158388337));
#19914=CARTESIAN_POINT('Ctrl Pts',(-5.8878326534242,-0.584257826453108,
35.5909275605582));
#19915=CARTESIAN_POINT('Ctrl Pts',(-5.90336373681984,-0.427744013852536,
35.5835232368617));
#19916=CARTESIAN_POINT('Ctrl Pts',(-5.91264866230486,-0.27062888192908,
35.5761189131652));
#19917=CARTESIAN_POINT('Ctrl Pts',(-5.91566280353483,-0.113420268798857,
35.5687145894688));
#19918=CARTESIAN_POINT('Ctrl Pts',(-5.91638732153701,-0.0756315715813799,
35.5669347903808));
#19919=CARTESIAN_POINT('Ctrl Pts',(-5.9167497460477,-0.0378359212400649,
35.5651549912929));
#19920=CARTESIAN_POINT('Ctrl Pts',(-5.91674999986659,-3.97337130474773E-5,
35.5633751922049));
#19921=CARTESIAN_POINT('Ctrl Pts',(-5.91702973121491,0.000122477731109751,
35.3116248172195));
#19922=CARTESIAN_POINT('Ctrl Pts',(-5.91624721053643,-0.84738287545781,
35.3515259607155));
#19923=CARTESIAN_POINT('Ctrl Pts',(-5.51859916564424,-2.67934504448225,
35.437742565973));
#19924=CARTESIAN_POINT('Ctrl Pts',(-3.69398986882353,-4.93928937015303,
35.5702746329922));
#19925=CARTESIAN_POINT('Ctrl Pts',(-0.880646612225805,-6.10463775972444,
35.7092210182773));
#19926=CARTESIAN_POINT('Ctrl Pts',(2.14735808427326,-5.78195415849901,35.8481674035626));
#19927=CARTESIAN_POINT('Ctrl Pts',(4.65193491316365,-4.04989409698157,35.9871137888476));
#19928=CARTESIAN_POINT('Ctrl Pts',(6.02258238500697,-1.3306547444329,36.1260601741327));
#19929=CARTESIAN_POINT('Ctrl Pts',(5.92519922033558,1.71293748643058,36.265006559418));
#19930=CARTESIAN_POINT('Ctrl Pts',(4.38352298886376,4.33899375883021,36.4039529447029));
#19931=CARTESIAN_POINT('Ctrl Pts',(1.77334397367895,5.90740144091314,36.5428993299881));
#19932=CARTESIAN_POINT('Ctrl Pts',(-1.26909534381814,6.03585434229275,36.6818457152732));
#19933=CARTESIAN_POINT('Ctrl Pts',(-4.0021871545,4.69304150987745,36.8207921005585));
#19934=CARTESIAN_POINT('Ctrl Pts',(-5.60347011563501,2.42737082897272,36.947385131399));
#19935=CARTESIAN_POINT('Ctrl Pts',(-5.91593150251293,0.721344592538736,
37.0276627004779));
#19936=CARTESIAN_POINT('Ctrl Pts',(-5.91663997003447,-0.000151814981789717,
37.0616248077951));
#19937=CARTESIAN_POINT('Origin',(0.,0.,0.));
#19938=CARTESIAN_POINT('',(-5.91674999872984,0.000122598544046725,39.0633751922447));
#19939=CARTESIAN_POINT('',(-5.91674999852514,0.000132108695946752,38.8116248077543));
#19940=CARTESIAN_POINT('',(-5.91675,-7.2459289488551E-16,0.));
#19941=CARTESIAN_POINT('Ctrl Pts',(-5.91674999872983,0.000122599388472625,
39.0633751922049));
#19942=CARTESIAN_POINT('Ctrl Pts',(-5.9167471879205,0.135774630831213,39.0569882872305));
#19943=CARTESIAN_POINT('Ctrl Pts',(-5.91207783419387,0.271407816372676,
39.050601382256));
#19944=CARTESIAN_POINT('Ctrl Pts',(-5.90275448146221,0.406718691576558,
39.0442144772815));
#19945=CARTESIAN_POINT('Ctrl Pts',(-5.89138589776885,0.571712235600173,
39.0364264995193));
#19946=CARTESIAN_POINT('Ctrl Pts',(-5.87309310901039,0.736258323381238,
39.028638521757));
#19947=CARTESIAN_POINT('Ctrl Pts',(-5.8479353267559,0.899768290495045,39.0208505439948));
#19948=CARTESIAN_POINT('Ctrl Pts',(-5.82278249073704,1.06324611014776,39.0130640974158));
#19949=CARTESIAN_POINT('Ctrl Pts',(-5.79076740286871,1.22568789995535,39.0052776508368));
#19950=CARTESIAN_POINT('Ctrl Pts',(-5.75200085210035,1.38651244492677,38.9974912042578));
#19951=CARTESIAN_POINT('Ctrl Pts',(-5.71323282247546,1.54734312499211,38.9897044606434));
#19952=CARTESIAN_POINT('Ctrl Pts',(-5.66771288561786,1.70655612520183,38.981917717029));
#19953=CARTESIAN_POINT('Ctrl Pts',(-5.61560261758027,1.86358198207797,38.9741309734147));
#19954=CARTESIAN_POINT('Ctrl Pts',(-5.5634957962471,2.02059745286828,38.9663447448352));
#19955=CARTESIAN_POINT('Ctrl Pts',(-5.50479961680108,2.17542576654225,38.9585585162557));
#19956=CARTESIAN_POINT('Ctrl Pts',(-5.43972509730625,2.32751400172728,38.9507722876762));
#19957=CARTESIAN_POINT('Ctrl Pts',(-5.37463344717792,2.47964227359391,38.9429840094));
#19958=CARTESIAN_POINT('Ctrl Pts',(-5.30316022584418,2.62902873087834,38.9351957311238));
#19959=CARTESIAN_POINT('Ctrl Pts',(-5.22556440710126,2.77514093150896,38.9274074528476));
#19960=CARTESIAN_POINT('Ctrl Pts',(-5.15179398714427,2.91404994201986,38.9200031291548));
#19961=CARTESIAN_POINT('Ctrl Pts',(-5.07249022789409,3.04999952188263,38.912598805462));
#19962=CARTESIAN_POINT('Ctrl Pts',(-4.98791394360065,3.18255322873542,38.9051944817693));
#19963=CARTESIAN_POINT('Ctrl Pts',(-4.89895535014512,3.3219751886554,38.8974065040081));
#19964=CARTESIAN_POINT('Ctrl Pts',(-4.80413151259739,3.45768989290758,38.8896185262469));
#19965=CARTESIAN_POINT('Ctrl Pts',(-4.70377619292479,3.58920883891896,38.8818305484857));
#19966=CARTESIAN_POINT('Ctrl Pts',(-4.6034406039686,3.72070192717776,38.8740441019077));
#19967=CARTESIAN_POINT('Ctrl Pts',(-4.49757589656964,3.84800064927392,38.8662576553297));
#19968=CARTESIAN_POINT('Ctrl Pts',(-4.3865575516465,3.97064773161672,38.8584712087517));
#19969=CARTESIAN_POINT('Ctrl Pts',(-4.27553497162364,4.09329949266939,38.8506844651383));
#19970=CARTESIAN_POINT('Ctrl Pts',(-4.15935857218371,4.21129901933567,38.8428977215249));
#19971=CARTESIAN_POINT('Ctrl Pts',(-4.03844280007124,4.32422366593737,38.8351109779115));
#19972=CARTESIAN_POINT('Ctrl Pts',(-3.91753502563239,4.43714084341859,38.8273247493329));
#19973=CARTESIAN_POINT('Ctrl Pts',(-3.79188873946776,4.54498359450944,38.8195385207543));
#19974=CARTESIAN_POINT('Ctrl Pts',(-3.66195388006204,4.64736746371519,38.8117522921757));
#19975=CARTESIAN_POINT('Ctrl Pts',(-3.53198481577141,4.74977828510667,38.8039640139004));
#19976=CARTESIAN_POINT('Ctrl Pts',(-3.39772517230712,4.84672715368042,38.7961757356252));
#19977=CARTESIAN_POINT('Ctrl Pts',(-3.25965719033948,4.93787054953531,38.7883874573499));
#19978=CARTESIAN_POINT('Ctrl Pts',(-3.12839582619023,5.02452066422961,38.7809831336521));
#19979=CARTESIAN_POINT('Ctrl Pts',(-2.99369279308517,5.10592378088708,38.7735788099543));
#19980=CARTESIAN_POINT('Ctrl Pts',(-2.85598599568298,5.1818215479658,38.7661744862566));
#19981=CARTESIAN_POINT('Ctrl Pts',(-2.71114393858502,5.26165194791852,38.7583865084949));
#19982=CARTESIAN_POINT('Ctrl Pts',(-2.56292676073579,5.33541989021992,38.7505985307332));
#19983=CARTESIAN_POINT('Ctrl Pts',(-2.41186133414479,5.40285623234205,38.7428105529715));
#19984=CARTESIAN_POINT('Ctrl Pts',(-2.2608256083118,5.47027931590116,38.735024106393));
#19985=CARTESIAN_POINT('Ctrl Pts',(-2.10694304269897,5.53137315293793,38.7272376598145));
#19986=CARTESIAN_POINT('Ctrl Pts',(-1.95076219010932,5.58591598935572,38.719451213236));
#19987=CARTESIAN_POINT('Ctrl Pts',(-1.79457537957215,5.64046090645979,38.7116644696221));
#19988=CARTESIAN_POINT('Ctrl Pts',(-1.63609040698825,5.68845421379307,38.7038777260083));
#19989=CARTESIAN_POINT('Ctrl Pts',(-1.47587346176335,5.72972321210743,38.6960909823944));
#19990=CARTESIAN_POINT('Ctrl Pts',(-1.31566711369084,5.77098948078627,38.6883047538154));
#19991=CARTESIAN_POINT('Ctrl Pts',(-1.15372933172641,5.80553225087759,38.6805185252363));
#19992=CARTESIAN_POINT('Ctrl Pts',(-0.990639186501122,5.83322934271133,
38.6727322966573));
#19993=CARTESIAN_POINT('Ctrl Pts',(-0.827506108380989,5.86093372570499,
38.6649440183816));
#19994=CARTESIAN_POINT('Ctrl Pts',(-0.663220375753615,5.88178877399905,
38.6571557401059));
#19995=CARTESIAN_POINT('Ctrl Pts',(-0.498369825920027,5.895723711226,38.6493674618301));
#19996=CARTESIAN_POINT('Ctrl Pts',(-0.341646248626712,5.90897166953594,
38.6419631381348));
#19997=CARTESIAN_POINT('Ctrl Pts',(-0.184412465069586,5.91596536824798,
38.6345588144394));
#19998=CARTESIAN_POINT('Ctrl Pts',(-0.027176618381928,5.91668758630311,
38.627154490744));
#19999=CARTESIAN_POINT('Ctrl Pts',(0.138206383183557,5.91744722599252,38.6193665129826));
#20000=CARTESIAN_POINT('Ctrl Pts',(0.303650828059728,5.91126848996617,38.6115785352211));
#20001=CARTESIAN_POINT('Ctrl Pts',(0.468565294811073,5.89816726848253,38.6037905574597));
#20002=CARTESIAN_POINT('Ctrl Pts',(0.633447337964542,5.88506862281134,38.5960041108814));
#20003=CARTESIAN_POINT('Ctrl Pts',(0.797799292548417,5.86505023260907,38.5882176643032));
#20004=CARTESIAN_POINT('Ctrl Pts',(0.961033384763278,5.83817997289142,38.5804312177249));
#20005=CARTESIAN_POINT('Ctrl Pts',(1.12427370399059,5.81130868813396,38.5726444741113));
#20006=CARTESIAN_POINT('Ctrl Pts',(1.28639575957966,5.77758505882802,38.5648577304977));
#20007=CARTESIAN_POINT('Ctrl Pts',(1.4468197738114,5.7371284720327,38.557070986884));
#20008=CARTESIAN_POINT('Ctrl Pts',(1.6072331771948,5.69667456113793,38.5492847583052));
#20009=CARTESIAN_POINT('Ctrl Pts',(1.76594845412817,5.64948866219114,38.5414985297264));
#20010=CARTESIAN_POINT('Ctrl Pts',(1.92239869929495,5.5957406840783,38.5337123011476));
#20011=CARTESIAN_POINT('Ctrl Pts',(2.07889012942669,5.54197855700332,38.5259240228721));
#20012=CARTESIAN_POINT('Ctrl Pts',(2.23311503328575,5.4816510010094,38.5181357445966));
#20013=CARTESIAN_POINT('Ctrl Pts',(2.38452341353271,5.41497725321301,38.5103474663211));
#20014=CARTESIAN_POINT('Ctrl Pts',(2.52846750721535,5.35159045663462,38.5029431426246));
#20015=CARTESIAN_POINT('Ctrl Pts',(2.66986585041888,5.28246822388523,38.4955388189281));
#20016=CARTESIAN_POINT('Ctrl Pts',(2.8082640521683,5.20783866645265,38.4881344952316));
#20017=CARTESIAN_POINT('Ctrl Pts',(2.95383333866183,5.12934218825087,38.48034651747));
#20018=CARTESIAN_POINT('Ctrl Pts',(3.09613539840919,5.04472443058755,38.4725585397084));
#20019=CARTESIAN_POINT('Ctrl Pts',(3.234658571696,4.95428243916852,38.4647705619468));
#20020=CARTESIAN_POINT('Ctrl Pts',(3.37315451013931,4.86385822942041,38.4569841153684));
#20021=CARTESIAN_POINT('Ctrl Pts',(3.50787277714379,4.76761224530614,38.44919766879));
#20022=CARTESIAN_POINT('Ctrl Pts',(3.63832979901089,4.66588542895444,38.4414112222116));
#20023=CARTESIAN_POINT('Ctrl Pts',(3.76879179751932,4.564154731954,38.4336244785978));
#20024=CARTESIAN_POINT('Ctrl Pts',(3.89499197119463,4.45694297771329,38.4258377349841));
#20025=CARTESIAN_POINT('Ctrl Pts',(4.01647842399972,4.34463250828476,38.4180509913703));
#20026=CARTESIAN_POINT('Ctrl Pts',(4.13795684138479,4.23232946735359,38.4102647627913));
#20027=CARTESIAN_POINT('Ctrl Pts',(4.25472192722656,4.11492860312819,38.4024785342124));
#20028=CARTESIAN_POINT('Ctrl Pts',(4.36635727055808,3.99285045404215,38.3946923056335));
#20029=CARTESIAN_POINT('Ctrl Pts',(4.47802200149266,3.87074016832195,38.3869040273578));
#20030=CARTESIAN_POINT('Ctrl Pts',(4.58455407432886,3.74395037204153,38.3791157490822));
#20031=CARTESIAN_POINT('Ctrl Pts',(4.68557553505414,3.61293682034465,38.3713274708065));
#20032=CARTESIAN_POINT('Ctrl Pts',(4.78161673555627,3.48838210992292,38.3639231471107));
#20033=CARTESIAN_POINT('Ctrl Pts',(4.87267741053592,3.36001027504955,38.3565188234148));
#20034=CARTESIAN_POINT('Ctrl Pts',(4.95846779589131,3.22823909889103,38.349114499719));
#20035=CARTESIAN_POINT('Ctrl Pts',(5.04870339886322,3.08964021644371,38.3413265219575));
#20036=CARTESIAN_POINT('Ctrl Pts',(5.13314033220658,2.94723078765855,38.3335385441961));
#20037=CARTESIAN_POINT('Ctrl Pts',(5.21147154663315,2.80151653236834,38.3257505664346));
#20038=CARTESIAN_POINT('Ctrl Pts',(5.28978736047149,2.65583092574979,38.3179641198564));
#20039=CARTESIAN_POINT('Ctrl Pts',(5.36199969940708,2.50684207037001,38.3101776732781));
#20040=CARTESIAN_POINT('Ctrl Pts',(5.42784718535444,2.35508078310276,38.3023912266998));
#20041=CARTESIAN_POINT('Ctrl Pts',(5.49369718323489,2.20331370648465,38.2946044830862));
#20042=CARTESIAN_POINT('Ctrl Pts',(5.55318171145486,2.0487742779088,38.2868177394725));
#20043=CARTESIAN_POINT('Ctrl Pts',(5.60608702159078,1.89201450016945,38.2790309958589));
#20044=CARTESIAN_POINT('Ctrl Pts',(5.65898883243623,1.73526509091662,38.2712447672801));
#20045=CARTESIAN_POINT('Ctrl Pts',(5.70531219394555,1.57629592922152,38.2634585387013));
#20046=CARTESIAN_POINT('Ctrl Pts',(5.74489279681686,1.41567556861795,38.2556723101225));
#20047=CARTESIAN_POINT('Ctrl Pts',(5.78448381913969,1.25501292528147,38.2478840318469));
#20048=CARTESIAN_POINT('Ctrl Pts',(5.81732845757911,1.09269852447719,38.2400957535714));
#20049=CARTESIAN_POINT('Ctrl Pts',(5.84331302498732,0.929313431794404,38.2323074752959));
#20050=CARTESIAN_POINT('Ctrl Pts',(5.86801657837826,0.773983066006007,38.2249031515995));
#20051=CARTESIAN_POINT('Ctrl Pts',(5.88652011578327,0.617685293712312,38.217498827903));
#20052=CARTESIAN_POINT('Ctrl Pts',(5.89876920452956,0.460925627616558,38.2100945042066));
#20053=CARTESIAN_POINT('Ctrl Pts',(5.91165297820922,0.296043479898478,38.202306526445));
#20054=CARTESIAN_POINT('Ctrl Pts',(5.91762155709263,0.130591320086449,38.1945185486834));
#20055=CARTESIAN_POINT('Ctrl Pts',(5.91664742458522,-0.0348398571903262,
38.1867305709218));
#20056=CARTESIAN_POINT('Ctrl Pts',(5.91567348360062,-0.200238509279394,
38.1789441243434));
#20057=CARTESIAN_POINT('Ctrl Pts',(5.90775955667576,-0.36561586771609,38.171157677765));
#20058=CARTESIAN_POINT('Ctrl Pts',(5.89293023949894,-0.530380764073326,
38.1633712311866));
#20059=CARTESIAN_POINT('Ctrl Pts',(5.8781003566171,-0.695151945839907,38.1555844875728));
#20060=CARTESIAN_POINT('Ctrl Pts',(5.85635458030705,-0.859310300168159,
38.147797743959));
#20061=CARTESIAN_POINT('Ctrl Pts',(5.82776946593429,-1.02226885623303,38.1400110003452));
#20062=CARTESIAN_POINT('Ctrl Pts',(5.79918624225299,-1.18521663380852,38.1322247717663));
#20063=CARTESIAN_POINT('Ctrl Pts',(5.76376464109781,-1.34696445717608,38.1244385431873));
#20064=CARTESIAN_POINT('Ctrl Pts',(5.72163254750092,-1.5069344889139,38.1166523146084));
#20065=CARTESIAN_POINT('Ctrl Pts',(5.67948936278175,-1.66694663218784,38.1088640363327));
#20066=CARTESIAN_POINT('Ctrl Pts',(5.63063223530453,-1.82517973895856,38.1010757580571));
#20067=CARTESIAN_POINT('Ctrl Pts',(5.5752394852801,-1.98106921743631,38.0932874797814));
#20068=CARTESIAN_POINT('Ctrl Pts',(5.52257754421092,-2.12927349552827,38.0858831560856));
#20069=CARTESIAN_POINT('Ctrl Pts',(5.46400894584996,-2.27535940793032,38.0784788323898));
#20070=CARTESIAN_POINT('Ctrl Pts',(5.39972787092285,-2.41885706119212,38.071074508694));
#20071=CARTESIAN_POINT('Ctrl Pts',(5.33211608049055,-2.56979002662347,38.0632865309325));
#20072=CARTESIAN_POINT('Ctrl Pts',(5.25815992810046,-2.7179133827933,38.055498553171));
#20073=CARTESIAN_POINT('Ctrl Pts',(5.17811814410162,-2.86269506727936,38.0477105754096));
#20074=CARTESIAN_POINT('Ctrl Pts',(5.09809209700367,-3.00744828644511,38.0399241288313));
#20075=CARTESIAN_POINT('Ctrl Pts',(5.01198296015422,-3.14886086535153,38.032137682253));
#20076=CARTESIAN_POINT('Ctrl Pts',(4.92009530148782,-3.28642553342951,38.0243512356748));
#20077=CARTESIAN_POINT('Ctrl Pts',(4.82820413751447,-3.42399544928935,38.0165644920611));
#20078=CARTESIAN_POINT('Ctrl Pts',(4.73053418482264,-3.55771689268298,38.0087777484475));
#20079=CARTESIAN_POINT('Ctrl Pts',(4.62743362249892,-3.68711114992029,38.0009910048338));
#20080=CARTESIAN_POINT('Ctrl Pts',(4.52433987950609,-3.81649684869549,37.993204776255));
#20081=CARTESIAN_POINT('Ctrl Pts',(4.41581644492041,-3.94155568419812,37.9854185476762));
#20082=CARTESIAN_POINT('Ctrl Pts',(4.30225219322678,-4.06184153166706,37.9776323190974));
#20083=CARTESIAN_POINT('Ctrl Pts',(4.18865804615181,-4.18215904395327,37.9698440408218));
#20084=CARTESIAN_POINT('Ctrl Pts',(4.07002064848399,-4.29770082365773,37.9620557625463));
#20085=CARTESIAN_POINT('Ctrl Pts',(3.94676681635972,-4.40805651730802,37.9542674842708));
#20086=CARTESIAN_POINT('Ctrl Pts',(3.82958927883582,-4.51297178209789,37.9468631605744));
#20087=CARTESIAN_POINT('Ctrl Pts',(3.70823971020562,-4.61319980569276,37.9394588368779));
#20088=CARTESIAN_POINT('Ctrl Pts',(3.58311352307887,-4.70842097132673,37.9320545131815));
#20089=CARTESIAN_POINT('Ctrl Pts',(3.45150393891052,-4.80857600921993,37.9242665354199));
#20090=CARTESIAN_POINT('Ctrl Pts',(3.31566889624897,-4.90322738166368,37.9164785576583));
#20091=CARTESIAN_POINT('Ctrl Pts',(3.17609024029319,-4.9920317855573,37.9086905798967));
#20092=CARTESIAN_POINT('Ctrl Pts',(3.03653902669779,-5.08081872974378,37.9009041333183));
#20093=CARTESIAN_POINT('Ctrl Pts',(2.89324593784037,-5.16376082767102,37.8931176867399));
#20094=CARTESIAN_POINT('Ctrl Pts',(2.74672119710268,-5.24055848434943,37.8853312401615));
#20095=CARTESIAN_POINT('Ctrl Pts',(2.60019086677646,-5.31735907068531,37.8775444965477));
#20096=CARTESIAN_POINT('Ctrl Pts',(2.45042891906903,-5.38801459489937,37.8697577529339));
#20097=CARTESIAN_POINT('Ctrl Pts',(2.29797019854953,-5.45227141007106,37.8619710093201));
#20098=CARTESIAN_POINT('Ctrl Pts',(2.14552156203383,-5.51652397513513,37.8541847807412));
#20099=CARTESIAN_POINT('Ctrl Pts',(1.9903768041871,-5.57437855408287,37.8463985521622));
#20100=CARTESIAN_POINT('Ctrl Pts',(1.83309090073417,-5.6256295925119,37.8386123235833));
#20101=CARTESIAN_POINT('Ctrl Pts',(1.6757635923322,-5.67689412259268,37.8308240453077));
#20102=CARTESIAN_POINT('Ctrl Pts',(1.51629431545865,-5.72155153762187,37.823035767032));
#20103=CARTESIAN_POINT('Ctrl Pts',(1.35525423592285,-5.75944585168688,37.8152474887563));
#20104=CARTESIAN_POINT('Ctrl Pts',(1.20215327641925,-5.79547201275068,37.8078431650605));
#20105=CARTESIAN_POINT('Ctrl Pts',(1.04763291803855,-5.82538577818048,37.8004388413647));
#20106=CARTESIAN_POINT('Ctrl Pts',(0.892193321711462,-5.84909579671879,
37.7930345176689));
#20107=CARTESIAN_POINT('Ctrl Pts',(0.728699642994194,-5.87403434677219,
37.7852465399075));
#20108=CARTESIAN_POINT('Ctrl Pts',(0.56413045196339,-5.89211810973065,37.777458562146));
#20109=CARTESIAN_POINT('Ctrl Pts',(0.399073134922297,-5.90327631027748,
37.7696705843846));
#20110=CARTESIAN_POINT('Ctrl Pts',(0.23404826956456,-5.91443231702644,37.7618841378063));
#20111=CARTESIAN_POINT('Ctrl Pts',(0.0685357883111578,-5.91866545666666,
37.754097691228));
#20112=CARTESIAN_POINT('Ctrl Pts',(-0.0968729282384096,-5.9159569131523,
37.7463112446498));
#20113=CARTESIAN_POINT('Ctrl Pts',(-0.262287954757499,-5.91324826631312,
37.7385245010362));
#20114=CARTESIAN_POINT('Ctrl Pts',(-0.427598889091094,-5.90359740770875,
37.7307377574225));
#20115=CARTESIAN_POINT('Ctrl Pts',(-0.59221472716635,-5.88703764888822,
37.7229510138089));
#20116=CARTESIAN_POINT('Ctrl Pts',(-0.75681967713536,-5.87047898537185,
37.7151647852301));
#20117=CARTESIAN_POINT('Ctrl Pts',(-0.920729304889136,-5.84701236820843,
37.7073785566513));
#20118=CARTESIAN_POINT('Ctrl Pts',(-1.08335795159065,-5.81672297012891,
37.6995923280725));
#20119=CARTESIAN_POINT('Ctrl Pts',(-1.2460294096993,-5.78642559847414,37.691804049797));
#20120=CARTESIAN_POINT('Ctrl Pts',(-1.40741889821639,-5.74930191359766,
37.6840157715215));
#20121=CARTESIAN_POINT('Ctrl Pts',(-1.56695027028627,-5.70548835884798,
37.676227493246));
#20122=CARTESIAN_POINT('Ctrl Pts',(-1.71861690015822,-5.66383476993079,
37.6688231695495));
#20123=CARTESIAN_POINT('Ctrl Pts',(-1.86860395299201,-5.61613510008907,
37.661418845853));
#20124=CARTESIAN_POINT('Ctrl Pts',(-2.01642856245358,-5.56254855394732,
37.6540145221565));
#20125=CARTESIAN_POINT('Ctrl Pts',(-2.17191268474426,-5.50618542791717,
37.6462265443949));
#20126=CARTESIAN_POINT('Ctrl Pts',(-2.32505994031396,-5.44328901123178,
37.6384385666333));
#20127=CARTESIAN_POINT('Ctrl Pts',(-2.47532072830056,-5.37407832605235,
37.6306505888717));
#20128=CARTESIAN_POINT('Ctrl Pts',(-2.6255519737283,-5.30488124828685,37.6228641422933));
#20129=CARTESIAN_POINT('Ctrl Pts',(-2.77289759384758,-5.22937251266861,
37.6150776957148));
#20130=CARTESIAN_POINT('Ctrl Pts',(-2.916829352024,-5.14781867334809,37.6072912491364));
#20131=CARTESIAN_POINT('Ctrl Pts',(-3.06076660087231,-5.06626172293257,
37.5995045055226));
#20132=CARTESIAN_POINT('Ctrl Pts',(-3.20128944722143,-4.97865936145136,
37.5917177619088));
#20133=CARTESIAN_POINT('Ctrl Pts',(-3.33789493680239,-4.88532373066197,
37.583931018295));
#20134=CARTESIAN_POINT('Ctrl Pts',(-3.47449139095203,-4.7919942733264,37.5761447897161));
#20135=CARTESIAN_POINT('Ctrl Pts',(-3.6071707430359,-4.69293248592507,37.5683585611371));
#20136=CARTESIAN_POINT('Ctrl Pts',(-3.73545955613584,-4.58849348555421,
37.5605723325582));
#20137=CARTESIAN_POINT('Ctrl Pts',(-3.86378214080505,-4.48402699199162,
37.5527840542825));
#20138=CARTESIAN_POINT('Ctrl Pts',(-3.98771162775715,-4.37418065728952,
37.5449957760069));
#20139=CARTESIAN_POINT('Ctrl Pts',(-4.10680747312832,-4.25935006088457,
37.5372074977312));
#20140=CARTESIAN_POINT('Ctrl Pts',(-4.22003200860839,-4.15018050172547,
37.5298031740354));
#20141=CARTESIAN_POINT('Ctrl Pts',(-4.32888782019247,-4.03650646423048,
37.5223988503397));
#20142=CARTESIAN_POINT('Ctrl Pts',(-4.43302715905347,-3.91869886181553,
37.5149945266439));
#20143=CARTESIAN_POINT('Ctrl Pts',(-4.54256246416287,-3.79478707386043,
37.5072065488824));
#20144=CARTESIAN_POINT('Ctrl Pts',(-4.64691873605409,-3.66625766229791,
37.4994185711209));
#20145=CARTESIAN_POINT('Ctrl Pts',(-4.74571826592819,-3.53356600376101,
37.4916305933594));
#20146=CARTESIAN_POINT('Ctrl Pts',(-4.84449837096764,-3.40090043354185,
37.4838441467811));
#20147=CARTESIAN_POINT('Ctrl Pts',(-4.93772372313274,-3.26407450531249,
37.4760577002028));
#20148=CARTESIAN_POINT('Ctrl Pts',(-5.02505812334871,-3.12357510226137,
37.4682712536245));
#20149=CARTESIAN_POINT('Ctrl Pts',(-5.11239585517522,-2.98307033947468,
37.4604845100108));
#20150=CARTESIAN_POINT('Ctrl Pts',(-5.19384201332127,-2.8388920907489,37.4526977663971));
#20151=CARTESIAN_POINT('Ctrl Pts',(-5.2691044178346,-2.69155516318278,37.4449110227835));
#20152=CARTESIAN_POINT('Ctrl Pts',(-5.34436184430279,-2.54422798085243,
37.4371247942046));
#20153=CARTESIAN_POINT('Ctrl Pts',(-5.4134361903507,-2.39374282241546,37.4293385656258));
#20154=CARTESIAN_POINT('Ctrl Pts',(-5.47608176304281,-2.2406380981698,37.421552337047));
#20155=CARTESIAN_POINT('Ctrl Pts',(-5.53874382695698,-2.08749306965524,
37.4137640587714));
#20156=CARTESIAN_POINT('Ctrl Pts',(-5.59497361293785,-1.93172739259032,
37.4059757804958));
#20157=CARTESIAN_POINT('Ctrl Pts',(-5.64457367603185,-1.77389925822983,
37.3981875022203));
#20158=CARTESIAN_POINT('Ctrl Pts',(-5.69172850403234,-1.62385189810238,
37.390783178524));
#20159=CARTESIAN_POINT('Ctrl Pts',(-5.73289146179677,-1.47194078781932,
37.3833788548277));
#20160=CARTESIAN_POINT('Ctrl Pts',(-5.76793477125694,-1.31865804400732,
37.3759745311315));
#20161=CARTESIAN_POINT('Ctrl Pts',(-5.80546095191119,-1.15451498719907,
37.3680455999623));
#20162=CARTESIAN_POINT('Ctrl Pts',(-5.83598056412886,-0.988749824618148,
37.3601166687931));
#20163=CARTESIAN_POINT('Ctrl Pts',(-5.8593775349695,-0.821964394116137,
37.352187737624));
#20164=CARTESIAN_POINT('Ctrl Pts',(-5.88276867425801,-0.655220533864368,
37.3442607826925));
#20165=CARTESIAN_POINT('Ctrl Pts',(-5.89904067508326,-0.487457204634034,
37.3363338277611));
#20166=CARTESIAN_POINT('Ctrl Pts',(-5.90812900489858,-0.319283923767114,
37.3284068728296));
#20167=CARTESIAN_POINT('Ctrl Pts',(-5.91387366019098,-0.212983035968757,
37.3233963126359));
#20168=CARTESIAN_POINT('Ctrl Pts',(-5.91674918763453,-0.106518504630412,
37.3183857524422));
#20169=CARTESIAN_POINT('Ctrl Pts',(-5.91674999982786,-4.51337719426076E-5,
37.3133751922485));
#20170=CARTESIAN_POINT('Ctrl Pts',(-5.91674999805201,-0.000151827279522968,
37.0616248082411));
#20171=CARTESIAN_POINT('Ctrl Pts',(-5.91674555035387,-0.17347982250265,
37.0697835109022));
#20172=CARTESIAN_POINT('Ctrl Pts',(-5.9091204396543,-0.346769807533754,
37.0779422135633));
#20173=CARTESIAN_POINT('Ctrl Pts',(-5.89391063127059,-0.519372730411945,
37.0861009162245));
#20174=CARTESIAN_POINT('Ctrl Pts',(-5.88609077923648,-0.608113448474336,
37.0902955678592));
#20175=CARTESIAN_POINT('Ctrl Pts',(-5.87626689374088,-0.696672605295589,
37.0944902194939));
#20176=CARTESIAN_POINT('Ctrl Pts',(-5.86444920173335,-0.784962497695989,
37.0986848711286));
#20177=CARTESIAN_POINT('Ctrl Pts',(-5.84250756991799,-0.948888271936102,
37.1064729825216));
#20178=CARTESIAN_POINT('Ctrl Pts',(-5.81368452304766,-1.11192275153252,
37.1142610939145));
#20179=CARTESIAN_POINT('Ctrl Pts',(-5.77807696957521,-1.27348227163338,
37.1220492053075));
#20180=CARTESIAN_POINT('Ctrl Pts',(-5.7424764070251,-1.43501007233914,37.1298357876406));
#20181=CARTESIAN_POINT('Ctrl Pts',(-5.70009406437873,-1.59506317950582,
37.1376223699736));
#20182=CARTESIAN_POINT('Ctrl Pts',(-5.65107784236079,-1.75306867580222,
37.1454089523067));
#20183=CARTESIAN_POINT('Ctrl Pts',(-5.60205975136534,-1.91108019681262,
37.1531958315404));
#20184=CARTESIAN_POINT('Ctrl Pts',(-5.54640736574657,-2.0670436443859,37.1609827107741));
#20185=CARTESIAN_POINT('Ctrl Pts',(-5.48431851339339,-2.22040109127846,
37.1687695900078));
#20186=CARTESIAN_POINT('Ctrl Pts',(-5.42223375886856,-2.37374841666818,
37.176555955312));
#20187=CARTESIAN_POINT('Ctrl Pts',(-5.35371350773485,-2.52448978941045,
37.1843423206161));
#20188=CARTESIAN_POINT('Ctrl Pts',(-5.27900386516668,-2.67208696603522,
37.1921286859203));
#20189=CARTESIAN_POINT('Ctrl Pts',(-5.20427460536344,-2.8197228986814,37.1999170957659));
#20190=CARTESIAN_POINT('Ctrl Pts',(-5.12335284928681,-2.9642126993332,37.2077055056115));
#20191=CARTESIAN_POINT('Ctrl Pts',(-5.03653124272813,-3.1050416428002,37.215493915457));
#20192=CARTESIAN_POINT('Ctrl Pts',(-4.95427228166071,-3.23846974943158,
37.2228730291093));
#20193=CARTESIAN_POINT('Ctrl Pts',(-4.86671775478904,-3.36861165143155,
37.2302521427615));
#20194=CARTESIAN_POINT('Ctrl Pts',(-4.77415296928689,-3.49505278763414,
37.2376312564137));
#20195=CARTESIAN_POINT('Ctrl Pts',(-4.67645765050916,-3.62850210144088,
37.2454193678066));
#20196=CARTESIAN_POINT('Ctrl Pts',(-4.57314603088103,-3.75787643744925,
37.2532074791995));
#20197=CARTESIAN_POINT('Ctrl Pts',(-4.46458245377437,-3.882709630651,37.2609955905924));
#20198=CARTESIAN_POINT('Ctrl Pts',(-4.35604019123365,-4.0075183150313,37.2687821729254));
#20199=CARTESIAN_POINT('Ctrl Pts',(-4.24224823817848,-4.12778739460402,
37.2765687552584));
#20200=CARTESIAN_POINT('Ctrl Pts',(-4.12361057346573,-4.24308453850517,
37.2843553375914));
#20201=CARTESIAN_POINT('Ctrl Pts',(-4.00496838512514,-4.35838607866085,
37.2921422168251));
#20202=CARTESIAN_POINT('Ctrl Pts',(-3.88148034179317,-4.46871507828333,
37.2999290960587));
#20203=CARTESIAN_POINT('Ctrl Pts',(-3.75358709272272,-4.5736762565627,37.3077159752924));
#20204=CARTESIAN_POINT('Ctrl Pts',(-3.62570228453273,-4.67863050746502,
37.3155023405965));
#20205=CARTESIAN_POINT('Ctrl Pts',(-3.49341309951283,-4.77821744334559,
37.3232887059007));
#20206=CARTESIAN_POINT('Ctrl Pts',(-3.35719316289092,-4.87208216572119,
37.3310750712048));
#20207=CARTESIAN_POINT('Ctrl Pts',(-3.22093745767984,-4.96597153506679,
37.3388634810503));
#20208=CARTESIAN_POINT('Ctrl Pts',(-3.08074920062857,-5.05413550550532,
37.3466518908959));
#20209=CARTESIAN_POINT('Ctrl Pts',(-2.93713163336884,-5.13626209716405,
37.3544403007414));
#20210=CARTESIAN_POINT('Ctrl Pts',(-2.80106145058167,-5.21407277556443,
37.3618194143939));
#20211=CARTESIAN_POINT('Ctrl Pts',(-2.66191334676182,-5.28646417724288,
37.3691985280464));
#20212=CARTESIAN_POINT('Ctrl Pts',(-2.52013619733201,-5.35320876758949,
37.3765776416989));
#20213=CARTESIAN_POINT('Ctrl Pts',(-2.37050085022191,-5.42365277062102,
37.384365753092));
#20214=CARTESIAN_POINT('Ctrl Pts',(-2.21788331421212,-5.48783140625146,
37.3921538644851));
#20215=CARTESIAN_POINT('Ctrl Pts',(-2.06282655731286,-5.54550963906337,
37.3999419758781));
#20216=CARTESIAN_POINT('Ctrl Pts',(-1.90780024310472,-5.60317654775977,
37.4077285582113));
#20217=CARTESIAN_POINT('Ctrl Pts',(-1.75033596284705,-5.65434548878523,
37.4155151405445));
#20218=CARTESIAN_POINT('Ctrl Pts',(-1.59099530192642,-5.69883010027041,
37.4233017228777));
#20219=CARTESIAN_POINT('Ctrl Pts',(-1.43164856538189,-5.74331640794392,
37.4310886021115));
#20220=CARTESIAN_POINT('Ctrl Pts',(-1.27042561169685,-5.78111778635841,
37.4388754813454));
#20221=CARTESIAN_POINT('Ctrl Pts',(-1.10790250131735,-5.81209795255334,
37.4466623605792));
#20222=CARTESIAN_POINT('Ctrl Pts',(-0.945390117368948,-5.84307607407526,
37.4544487258835));
#20223=CARTESIAN_POINT('Ctrl Pts',(-0.781578062367603,-5.86723382456904,
37.4622350911878));
#20224=CARTESIAN_POINT('Ctrl Pts',(-0.617052033386599,-5.88448615858628,
37.4700214564921));
#20225=CARTESIAN_POINT('Ctrl Pts',(-0.452482803211596,-5.90174302271607,
37.4778098663378));
#20226=CARTESIAN_POINT('Ctrl Pts',(-0.287199542235393,-5.91209081189761,
37.4855982761836));
#20227=CARTESIAN_POINT('Ctrl Pts',(-0.121793420594745,-5.91549633802607,
37.4933866860293));
#20228=CARTESIAN_POINT('Ctrl Pts',(0.0349202853391011,-5.91872289708538,
37.5007657996809));
#20229=CARTESIAN_POINT('Ctrl Pts',(0.191744010902166,-5.91571807959255,
37.5081449133325));
#20230=CARTESIAN_POINT('Ctrl Pts',(0.348174727758624,-5.90649684004404,
37.515524026984));
#20231=CARTESIAN_POINT('Ctrl Pts',(0.513275836872115,-5.89676450033829,
37.523312138377));
#20232=CARTESIAN_POINT('Ctrl Pts',(0.677998101426518,-5.88010361416883,
37.5311002497699));
#20233=CARTESIAN_POINT('Ctrl Pts',(0.841752279586095,-5.85656756661371,
37.5388883611628));
#20234=CARTESIAN_POINT('Ctrl Pts',(1.00547430746745,-5.83303613995124,37.5466749434958));
#20235=CARTESIAN_POINT('Ctrl Pts',(1.16822831211086,-5.80263229062148,37.5544615258288));
#20236=CARTESIAN_POINT('Ctrl Pts',(1.32943199047928,-5.76546105226549,37.5622481081618));
#20237=CARTESIAN_POINT('Ctrl Pts',(1.49064181550798,-5.72828839657848,37.5700349873955));
#20238=CARTESIAN_POINT('Ctrl Pts',(1.65030088374228,-5.68434790347346,37.5778218666292));
#20239=CARTESIAN_POINT('Ctrl Pts',(1.80783814078094,-5.63379550740331,37.5856087458628));
#20240=CARTESIAN_POINT('Ctrl Pts',(1.96536500045176,-5.58324644776206,37.593395111167));
#20241=CARTESIAN_POINT('Ctrl Pts',(2.12077002492968,-5.5260864561731,37.6011814764711));
#20242=CARTESIAN_POINT('Ctrl Pts',(2.2734982115037,-5.46252107042064,37.6089678417752));
#20243=CARTESIAN_POINT('Ctrl Pts',(2.42626650139811,-5.39893899368868,37.6167562516208));
#20244=CARTESIAN_POINT('Ctrl Pts',(2.57635625294304,-5.32894828302026,37.6245446614664));
#20245=CARTESIAN_POINT('Ctrl Pts',(2.72323246778739,-5.25280263182319,37.6323330713119));
#20246=CARTESIAN_POINT('Ctrl Pts',(2.86239004984366,-5.18065858374901,37.6397121849643));
#20247=CARTESIAN_POINT('Ctrl Pts',(2.99866293236299,-5.10298998441233,37.6470912986167));
#20248=CARTESIAN_POINT('Ctrl Pts',(3.13161654943962,-5.02005063219246,37.6544704122691));
#20249=CARTESIAN_POINT('Ctrl Pts',(3.27193930751913,-4.93251424986062,37.662258523662));
#20250=CARTESIAN_POINT('Ctrl Pts',(3.40861453258895,-4.83907500532104,37.670046635055));
#20251=CARTESIAN_POINT('Ctrl Pts',(3.54115033924669,-4.74006169130245,37.6778347464479));
#20252=CARTESIAN_POINT('Ctrl Pts',(3.67366012480919,-4.64106781682205,37.6856213287809));
#20253=CARTESIAN_POINT('Ctrl Pts',(3.80203185771857,-4.53650224757727,37.693407911114));
#20254=CARTESIAN_POINT('Ctrl Pts',(3.9258044561838,-4.42673581031299,37.701194493447));
#20255=CARTESIAN_POINT('Ctrl Pts',(4.04958177407063,-4.31696518767893,37.7089813726807));
#20256=CARTESIAN_POINT('Ctrl Pts',(4.16875936493796,-4.20199350925795,37.7167682519144));
#20257=CARTESIAN_POINT('Ctrl Pts',(4.28291037742195,-4.08223091721565,37.724555131148));
#20258=CARTESIAN_POINT('Ctrl Pts',(4.39705385600517,-3.96247622943515,37.7323414964522));
#20259=CARTESIAN_POINT('Ctrl Pts',(4.50617119970149,-3.83793149218703,37.7401278617563));
#20260=CARTESIAN_POINT('Ctrl Pts',(4.60987338448563,-3.70904272575971,37.7479142270605));
#20261=CARTESIAN_POINT('Ctrl Pts',(4.7136027993576,-3.58012011575968,37.7557026369061));
#20262=CARTESIAN_POINT('Ctrl Pts',(4.81191401209567,-3.44685144521499,37.7634910467516));
#20263=CARTESIAN_POINT('Ctrl Pts',(4.90445860430809,-3.30971545017519,37.7712794565972));
#20264=CARTESIAN_POINT('Ctrl Pts',(4.99213979692452,-3.17978622029505,37.7786585702496));
#20265=CARTESIAN_POINT('Ctrl Pts',(5.07464472888979,-3.04638589782895,37.7860376839019));
#20266=CARTESIAN_POINT('Ctrl Pts',(5.15171322405697,-2.90994526058079,37.7934167975542));
#20267=CARTESIAN_POINT('Ctrl Pts',(5.23305334883766,-2.76594220933593,37.8012049089472));
#20268=CARTESIAN_POINT('Ctrl Pts',(5.30836635418492,-2.6185008284622,37.8089930203402));
#20269=CARTESIAN_POINT('Ctrl Pts',(5.37737761033478,-2.4681451736821,37.8167811317332));
#20270=CARTESIAN_POINT('Ctrl Pts',(5.44637531732751,-2.31781903861378,37.8245677140663));
#20271=CARTESIAN_POINT('Ctrl Pts',(5.50907361057417,-2.16458006150297,37.8323542963994));
#20272=CARTESIAN_POINT('Ctrl Pts',(5.56524502022065,-2.00897447156734,37.8401408787325));
#20273=CARTESIAN_POINT('Ctrl Pts',(5.62141857167049,-1.85336294842517,37.8479277579662));
#20274=CARTESIAN_POINT('Ctrl Pts',(5.67106462933165,-1.69538493108427,37.8557146371999));
#20275=CARTESIAN_POINT('Ctrl Pts',(5.71400459175321,-1.53560479548718,37.8635015164337));
#20276=CARTESIAN_POINT('Ctrl Pts',(5.7569417201621,-1.37583520528655,37.8712878817379));
#20277=CARTESIAN_POINT('Ctrl Pts',(5.79317355621734,-1.21426404347849,37.8790742470421));
#20278=CARTESIAN_POINT('Ctrl Pts',(5.82257188087655,-1.05146909347147,37.8868606123463));
#20279=CARTESIAN_POINT('Ctrl Pts',(5.85197792493881,-0.888631396816528,
37.894649022192));
#20280=CARTESIAN_POINT('Ctrl Pts',(5.87454681340574,-0.724569584158841,
37.9024374320376));
#20281=CARTESIAN_POINT('Ctrl Pts',(5.89020163634249,-0.559870740196556,
37.9102258418832));
#20282=CARTESIAN_POINT('Ctrl Pts',(5.90503376766878,-0.403827143101491,
37.9176049555353));
#20283=CARTESIAN_POINT('Ctrl Pts',(5.91365981326503,-0.247212006003625,
37.9249840691874));
#20284=CARTESIAN_POINT('Ctrl Pts',(5.91605740580995,-0.0905280821691331,
37.9323631828394));
#20285=CARTESIAN_POINT('Ctrl Pts',(5.91858788828999,0.0748402682650383,
37.9401512942324));
#20286=CARTESIAN_POINT('Ctrl Pts',(5.91418080147477,0.240344307955706,37.9479394056253));
#20287=CARTESIAN_POINT('Ctrl Pts',(5.90284571343753,0.405392459047019,37.9557275170183));
#20288=CARTESIAN_POINT('Ctrl Pts',(5.89151285084722,0.570408205811078,37.9635140993513));
#20289=CARTESIAN_POINT('Ctrl Pts',(5.87325472290218,0.734967923985702,37.9713006816844));
#20290=CARTESIAN_POINT('Ctrl Pts',(5.84813291845099,0.898483127626742,37.9790872640174));
#20291=CARTESIAN_POINT('Ctrl Pts',(5.82301015611099,1.06200456606606,37.9868741432511));
#20292=CARTESIAN_POINT('Ctrl Pts',(5.79102323819929,1.22448109386781,37.9946610224848));
#20293=CARTESIAN_POINT('Ctrl Pts',(5.7522853480579,1.38533167040185,38.0024479017185));
#20294=CARTESIAN_POINT('Ctrl Pts',(5.71355001459484,1.54617163089094,38.0102342670227));
#20295=CARTESIAN_POINT('Ctrl Pts',(5.6680646754706,1.7053855442165,38.0180206323268));
#20296=CARTESIAN_POINT('Ctrl Pts',(5.61599317057472,1.86240470106745,38.025806997631));
#20297=CARTESIAN_POINT('Ctrl Pts',(5.56390799275907,2.01946508796038,38.0335954074766));
#20298=CARTESIAN_POINT('Ctrl Pts',(5.50523329228426,2.17432926271722,38.0413838173222));
#20299=CARTESIAN_POINT('Ctrl Pts',(5.44018241480332,2.32644489643848,38.0491722271678));
#20300=CARTESIAN_POINT('Ctrl Pts',(5.37855008835583,2.4705665556432,38.05655134082));
#20301=CARTESIAN_POINT('Ctrl Pts',(5.31119461147333,2.61222088690754,38.0639304544722));
#20302=CARTESIAN_POINT('Ctrl Pts',(5.23833687779192,2.75095570979708,38.0713095681245));
#20303=CARTESIAN_POINT('Ctrl Pts',(5.16144090186704,2.89738010514689,38.0790976795175));
#20304=CARTESIAN_POINT('Ctrl Pts',(5.07838796945833,3.04060447453471,38.0868857909104));
#20305=CARTESIAN_POINT('Ctrl Pts',(4.98946951421679,3.18011391764529,38.0946739023034));
#20306=CARTESIAN_POINT('Ctrl Pts',(4.9005685165638,3.31959597050883,38.1024604846365));
#20307=CARTESIAN_POINT('Ctrl Pts',(4.80580446548167,3.45536428310203,38.1102470669695));
#20308=CARTESIAN_POINT('Ctrl Pts',(4.70551299597211,3.58693155876128,38.1180336493026));
#20309=CARTESIAN_POINT('Ctrl Pts',(4.60521770237119,3.71850385105139,38.1258205285363));
#20310=CARTESIAN_POINT('Ctrl Pts',(4.49939475917456,3.84587452937775,38.13360740777));
#20311=CARTESIAN_POINT('Ctrl Pts',(4.38842154558554,3.96858751960199,38.1413942870037));
#20312=CARTESIAN_POINT('Ctrl Pts',(4.27745565616441,4.09129241083986,38.1491806523079));
#20313=CARTESIAN_POINT('Ctrl Pts',(4.16134039099671,4.20933999220777,38.1569670176121));
#20314=CARTESIAN_POINT('Ctrl Pts',(4.04049171221856,4.32230925385876,38.1647533829163));
#20315=CARTESIAN_POINT('Ctrl Pts',(3.91961130103145,4.43530817894379,38.1725417927619));
#20316=CARTESIAN_POINT('Ctrl Pts',(3.79399522491412,4.54322590000898,38.1803302026075));
#20317=CARTESIAN_POINT('Ctrl Pts',(3.66409508117712,4.64567947652371,38.1881186124531));
#20318=CARTESIAN_POINT('Ctrl Pts',(3.54102144444373,4.74274891690509,38.1954977261053));
#20319=CARTESIAN_POINT('Ctrl Pts',(3.4141026353678,4.83491358331393,38.2028768397574));
#20320=CARTESIAN_POINT('Ctrl Pts',(3.28374896475881,4.92188208909411,38.2102559534096));
#20321=CARTESIAN_POINT('Ctrl Pts',(3.14617025882768,5.01367094648573,38.2180440648026));
#20322=CARTESIAN_POINT('Ctrl Pts',(3.00471599413142,5.09970408293563,38.2258321761955));
#20323=CARTESIAN_POINT('Ctrl Pts',(2.85988843167947,5.17966878485931,38.2336202875885));
#20324=CARTESIAN_POINT('Ctrl Pts',(2.7150893035948,5.2596177871077,38.2414068699215));
#20325=CARTESIAN_POINT('Ctrl Pts',(2.5669184787667,5.33350057773942,38.2491934522546));
#20326=CARTESIAN_POINT('Ctrl Pts',(2.41590382585929,5.40104983005142,38.2569800345876));
#20327=CARTESIAN_POINT('Ctrl Pts',(2.26488341479661,5.46860165800145,38.2647669138213));
#20328=CARTESIAN_POINT('Ctrl Pts',(2.11101924873187,5.52981933032966,38.272553793055));
#20329=CARTESIAN_POINT('Ctrl Pts',(1.95486091490845,5.58448290944321,38.2803406722888));
#20330=CARTESIAN_POINT('Ctrl Pts',(1.79871288744472,5.63914288079217,38.2881270375929));
#20331=CARTESIAN_POINT('Ctrl Pts',(1.6402712968716,5.68724951909089,38.2959134028971));
#20332=CARTESIAN_POINT('Ctrl Pts',(1.48010283499295,5.72863213693686,38.3036997682013));
#20333=CARTESIAN_POINT('Ctrl Pts',(1.31989231612876,5.77002562101793,38.3114881780469));
#20334=CARTESIAN_POINT('Ctrl Pts',(1.15795432897601,5.80469147476326,38.3192765878925));
#20335=CARTESIAN_POINT('Ctrl Pts',(0.994868643695197,5.83250948943009,38.3270649977381));
#20336=CARTESIAN_POINT('Ctrl Pts',(0.840353430629375,5.85886561293605,38.3344441113903));
#20337=CARTESIAN_POINT('Ctrl Pts',(0.684808300786823,5.87907507641403,38.3418232250425));
#20338=CARTESIAN_POINT('Ctrl Pts',(0.528732967106978,5.89307831375031,38.3492023386947));
#20339=CARTESIAN_POINT('Ctrl Pts',(0.364006938796237,5.90785770018834,38.3569904500876));
#20340=CARTESIAN_POINT('Ctrl Pts',(0.198631433735107,5.91572865270471,38.3647785614805));
#20341=CARTESIAN_POINT('Ctrl Pts',(0.0331971119871187,5.9166568697412,38.3725666728734));
#20342=CARTESIAN_POINT('Ctrl Pts',(-0.132204729615795,5.91758490453846,
38.3803532552064));
#20343=CARTESIAN_POINT('Ctrl Pts',(-0.297665045538489,5.91157292182418,
38.3881398375394));
#20344=CARTESIAN_POINT('Ctrl Pts',(-0.462592403735932,5.89863872690181,
38.3959264198724));
#20345=CARTESIAN_POINT('Ctrl Pts',(-0.627526050576847,5.88570403880147,
38.4037132991061));
#20346=CARTESIAN_POINT('Ctrl Pts',(-0.791926380182615,5.86584663138872,
38.4115001783397));
#20347=CARTESIAN_POINT('Ctrl Pts',(-0.955205561549463,5.83913631436063,
38.4192870575734));
#20348=CARTESIAN_POINT('Ctrl Pts',(-1.11847396658491,5.81242776019798,38.4270734228775));
#20349=CARTESIAN_POINT('Ctrl Pts',(-1.28062105611454,5.77886725322325,38.4348597881816));
#20350=CARTESIAN_POINT('Ctrl Pts',(-1.44106754225738,5.73857603427473,38.4426461534858));
#20351=CARTESIAN_POINT('Ctrl Pts',(-1.60155615838923,5.69827423567032,38.4504345633313));
#20352=CARTESIAN_POINT('Ctrl Pts',(-1.7603429682634,5.65123826955373,38.4582229731768));
#20353=CARTESIAN_POINT('Ctrl Pts',(-1.91686135036628,5.59763996037366,38.4660113830224));
#20354=CARTESIAN_POINT('Ctrl Pts',(-2.06515438490714,5.54685834732741,38.4733904966749));
#20355=CARTESIAN_POINT('Ctrl Pts',(-2.21141103396735,5.49018646329872,38.4807696103274));
#20356=CARTESIAN_POINT('Ctrl Pts',(-2.35516398967869,5.42781108221544,38.4881487239799));
#20357=CARTESIAN_POINT('Ctrl Pts',(-2.50688465490904,5.36197845800871,38.495936835373));
#20358=CARTESIAN_POINT('Ctrl Pts',(-2.65587040209376,5.28976864769933,38.5037249467661));
#20359=CARTESIAN_POINT('Ctrl Pts',(-2.80158614807328,5.21143412290935,38.5115130581591));
#20360=CARTESIAN_POINT('Ctrl Pts',(-2.94727328530633,5.13311497773771,38.5192996404923));
#20361=CARTESIAN_POINT('Ctrl Pts',(-3.08969142106573,5.04867366859599,38.5270862228255));
#20362=CARTESIAN_POINT('Ctrl Pts',(-3.22832972405745,4.95840879267403,38.5348728051587));
#20363=CARTESIAN_POINT('Ctrl Pts',(-3.36697331329682,4.86814047497244,38.5426596843925));
#20364=CARTESIAN_POINT('Ctrl Pts',(-3.50183651145808,4.77204831719295,38.5504465636264));
#20365=CARTESIAN_POINT('Ctrl Pts',(-3.63243653013948,4.67047485990539,38.5582334428602));
#20366=CARTESIAN_POINT('Ctrl Pts',(-3.76302792929524,4.56890810640722,38.5660198081645));
#20367=CARTESIAN_POINT('Ctrl Pts',(-3.8893564598587,4.46186097361815,38.5738061734689));
#20368=CARTESIAN_POINT('Ctrl Pts',(-4.01097144181087,4.34971707763592,38.5815925387732));
#20369=CARTESIAN_POINT('Ctrl Pts',(-4.13261835738758,4.237543734944,38.5893809486189));
#20370=CARTESIAN_POINT('Ctrl Pts',(-4.2495490148332,4.12027117016764,38.5971693584646));
#20371=CARTESIAN_POINT('Ctrl Pts',(-4.36134805773805,3.99832135799069,38.6049577683103));
#20372=CARTESIAN_POINT('Ctrl Pts',(-4.46727184193451,3.88278024733178,38.6123368819619));
#20373=CARTESIAN_POINT('Ctrl Pts',(-4.56858931620707,3.76304103389447,38.6197159956135));
#20374=CARTESIAN_POINT('Ctrl Pts',(-4.6649794860832,3.63949130469121,38.627095109265));
#20375=CARTESIAN_POINT('Ctrl Pts',(-4.76671221654703,3.50909365816702,38.634883220658));
#20376=CARTESIAN_POINT('Ctrl Pts',(-4.86299228233177,3.37440454019386,38.6426713320509));
#20377=CARTESIAN_POINT('Ctrl Pts',(-4.95347060602803,3.23590165451862,38.6504594434438));
#20378=CARTESIAN_POINT('Ctrl Pts',(-5.04393116588276,3.09742596147043,38.6582460257768));
#20379=CARTESIAN_POINT('Ctrl Pts',(-5.12859208179027,2.95513826207483,38.6660326081098));
#20380=CARTESIAN_POINT('Ctrl Pts',(-5.20714764055606,2.80954516104502,38.6738191904429));
#20381=CARTESIAN_POINT('Ctrl Pts',(-5.28570619462777,2.66394650858276,38.6816060696765));
#20382=CARTESIAN_POINT('Ctrl Pts',(-5.35815877053739,2.51504248161278,38.6893929489102));
#20383=CARTESIAN_POINT('Ctrl Pts',(-5.42424530425686,2.36336485582473,38.6971798281439));
#20384=CARTESIAN_POINT('Ctrl Pts',(-5.49032747630335,2.21169724067218,38.704966193448));
#20385=CARTESIAN_POINT('Ctrl Pts',(-5.55004431942148,2.05725668602571,38.7127525587522));
#20386=CARTESIAN_POINT('Ctrl Pts',(-5.60318361666804,1.90059567515106,38.7205389240563));
#20387=CARTESIAN_POINT('Ctrl Pts',(-5.65633686721495,1.74389352827628,38.7283273339019));
#20388=CARTESIAN_POINT('Ctrl Pts',(-5.70290901617878,1.58497006229457,38.7361157437475));
#20389=CARTESIAN_POINT('Ctrl Pts',(-5.74273721718423,1.42439454396143,38.743904153593));
#20390=CARTESIAN_POINT('Ctrl Pts',(-5.78047236821199,1.27225758364953,38.7512832672454));
#20391=CARTESIAN_POINT('Ctrl Pts',(-5.8121540929384,1.11863799456283,38.7586623808978));
#20392=CARTESIAN_POINT('Ctrl Pts',(-5.83768595408446,0.964029700779509,
38.7660414945501));
#20393=CARTESIAN_POINT('Ctrl Pts',(-5.86560263673436,0.79498011023452,38.7741098595194));
#20394=CARTESIAN_POINT('Ctrl Pts',(-5.88617396736588,0.624704945254722,
38.7821782244886));
#20395=CARTESIAN_POINT('Ctrl Pts',(-5.89931905236653,0.453833979430056,
38.7902465894579));
#20396=CARTESIAN_POINT('Ctrl Pts',(-5.9109289426702,0.302918776583512,38.7973726622233));
#20397=CARTESIAN_POINT('Ctrl Pts',(-5.9167466179235,0.151539059100074,38.8044987349888));
#20398=CARTESIAN_POINT('Ctrl Pts',(-5.91674999852514,0.000132108695950693,
38.8116248077543));
#20399=CARTESIAN_POINT('Origin',(0.,0.,0.));
#20400=CARTESIAN_POINT('',(-5.91674999807463,-0.000150943316464095,40.8133751922049));
#20401=CARTESIAN_POINT('',(-5.91674999950574,-7.64775397920275E-5,40.5616248077532));
#20402=CARTESIAN_POINT('',(-5.91675,-7.2459289488551E-16,0.));
#20403=CARTESIAN_POINT('Ctrl Pts',(-5.91674999807463,-0.000150943316464095,
40.8133751922049));
#20404=CARTESIAN_POINT('Ctrl Pts',(-5.91675420785041,0.16486590810397,40.8056078136878));
#20405=CARTESIAN_POINT('Ctrl Pts',(-5.90985064980782,0.329899361430627,
40.7978404351708));
#20406=CARTESIAN_POINT('Ctrl Pts',(-5.89606122030937,0.494360848838174,
40.7900730566537));
#20407=CARTESIAN_POINT('Ctrl Pts',(-5.88227108254778,0.658830783441378,
40.7823052791827));
#20408=CARTESIAN_POINT('Ctrl Pts',(-5.86159439040863,0.822728371697022,
40.7745375017117));
#20409=CARTESIAN_POINT('Ctrl Pts',(-5.83410500661337,0.985469093533016,
40.7667697242406));
#20410=CARTESIAN_POINT('Ctrl Pts',(-5.80661608301405,1.14820709094933,40.7590020768088));
#20411=CARTESIAN_POINT('Ctrl Pts',(-5.77231475214443,1.30978794303029,40.7512344293771));
#20412=CARTESIAN_POINT('Ctrl Pts',(-5.73132622610735,1.46963609524063,40.7434667819453));
#20413=CARTESIAN_POINT('Ctrl Pts',(-5.69032839687805,1.62952052828923,40.7356973714856));
#20414=CARTESIAN_POINT('Ctrl Pts',(-5.64264042152028,1.78767116355322,40.7279279610259));
#20415=CARTESIAN_POINT('Ctrl Pts',(-5.58843791706703,1.94352571621461,40.7201585505662));
#20416=CARTESIAN_POINT('Ctrl Pts',(-5.57052222974968,1.99504070543204,40.717590508188));
#20417=CARTESIAN_POINT('Ctrl Pts',(-5.55189522117018,2.04630497463979,40.7150224658099));
#20418=CARTESIAN_POINT('Ctrl Pts',(-5.53256441396586,2.09729863582148,40.7124544234318));
#20419=CARTESIAN_POINT('Ctrl Pts',(-5.47394081106185,2.25194464269218,40.7046664456704));
#20420=CARTESIAN_POINT('Ctrl Pts',(-5.40881867575399,2.4041587964738,40.6968784679091));
#20421=CARTESIAN_POINT('Ctrl Pts',(-5.33742501837016,2.55339474734643,40.6890904901478));
#20422=CARTESIAN_POINT('Ctrl Pts',(-5.26604539759129,2.702601357152,40.6813040435696));
#20423=CARTESIAN_POINT('Ctrl Pts',(-5.18839685282266,2.84883064428859,40.6735175969914));
#20424=CARTESIAN_POINT('Ctrl Pts',(-5.10475360990861,2.99155831375974,40.6657311504133));
#20425=CARTESIAN_POINT('Ctrl Pts',(-5.02110717619358,3.13429142796942,40.6579444067998));
#20426=CARTESIAN_POINT('Ctrl Pts',(-4.93146574488197,3.27352237953437,40.6501576631862));
#20427=CARTESIAN_POINT('Ctrl Pts',(-4.83614875604487,3.4087528176601,40.6423709195727));
#20428=CARTESIAN_POINT('Ctrl Pts',(-4.74083807171344,3.5439743113041,40.634584690994));
#20429=CARTESIAN_POINT('Ctrl Pts',(-4.63985276528638,3.67519555987536,40.6267984624153));
#20430=CARTESIAN_POINT('Ctrl Pts',(-4.53355481733812,3.80194835323815,40.6190122338366));
#20431=CARTESIAN_POINT('Ctrl Pts',(-4.42722888683693,3.92873451381845,40.6112239555612));
#20432=CARTESIAN_POINT('Ctrl Pts',(-4.31558772422202,4.05104962241858,40.6034356772858));
#20433=CARTESIAN_POINT('Ctrl Pts',(-4.19903328863283,4.16845894827493,40.5956473990104));
#20434=CARTESIAN_POINT('Ctrl Pts',(-4.08822487387036,4.2800801080421,40.5882430753134));
#20435=CARTESIAN_POINT('Ctrl Pts',(-3.97297614149774,4.38726734707188,40.5808387516164));
#20436=CARTESIAN_POINT('Ctrl Pts',(-3.85366303459733,4.4896783602256,40.5734344279194));
#20437=CARTESIAN_POINT('Ctrl Pts',(-3.72816773465678,4.59739578664105,40.5656464501577));
#20438=CARTESIAN_POINT('Ctrl Pts',(-3.59813079559704,4.69986741979239,40.557858472396));
#20439=CARTESIAN_POINT('Ctrl Pts',(-3.46401305146472,4.79672222895824,40.5500704946344));
#20440=CARTESIAN_POINT('Ctrl Pts',(-3.32992167603034,4.89355799563852,40.5422840480559));
#20441=CARTESIAN_POINT('Ctrl Pts',(-3.19175135529146,4.98477895479982,40.5344976014774));
#20442=CARTESIAN_POINT('Ctrl Pts',(-3.04999382142249,5.07005604030021,40.5267111548989));
#20443=CARTESIAN_POINT('Ctrl Pts',(-2.90823087982341,5.15533637892902,40.5189244112851));
#20444=CARTESIAN_POINT('Ctrl Pts',(-2.76288072304099,5.23467222206963,40.5111376676712));
#20445=CARTESIAN_POINT('Ctrl Pts',(-2.61446236253391,5.30777892506778,40.5033509240574));
#20446=CARTESIAN_POINT('Ctrl Pts',(-2.46605381879135,5.38088079260429,40.4955646954784));
#20447=CARTESIAN_POINT('Ctrl Pts',(-2.31457776416987,5.44775420338287,40.4877784668994));
#20448=CARTESIAN_POINT('Ctrl Pts',(-2.16057613318633,5.50816133888665,40.4799922383204));
#20449=CARTESIAN_POINT('Ctrl Pts',(-2.00653396182636,5.56858437635197,40.4722039600447));
#20450=CARTESIAN_POINT('Ctrl Pts',(-1.84996518256331,5.62253761855439,40.464415681769));
#20451=CARTESIAN_POINT('Ctrl Pts',(-1.69143080546665,5.66983177817636,40.4566274034933));
#20452=CARTESIAN_POINT('Ctrl Pts',(-1.54071201970464,5.71479438150819,40.4492230797978));
#20453=CARTESIAN_POINT('Ctrl Pts',(-1.38821702426881,5.75373858366138,40.4418187561022));
#20454=CARTESIAN_POINT('Ctrl Pts',(-1.23443974609842,5.78654379364336,40.4344144324067));
#20455=CARTESIAN_POINT('Ctrl Pts',(-1.07269451833015,5.82104880129892,40.4266264546453));
#20456=CARTESIAN_POINT('Ctrl Pts',(-0.909472737823357,5.8487740873626,40.4188384768839));
#20457=CARTESIAN_POINT('Ctrl Pts',(-0.745356615472228,5.86961447441583,
40.4110504991224));
#20458=CARTESIAN_POINT('Ctrl Pts',(-0.581272759757513,5.89045076407032,
40.4032640525442));
#20459=CARTESIAN_POINT('Ctrl Pts',(-0.416295229851423,5.90440481537482,
40.395477605966));
#20460=CARTESIAN_POINT('Ctrl Pts',(-0.251013278018535,5.91142308558256,
40.3876911593877));
#20461=CARTESIAN_POINT('Ctrl Pts',(-0.0857250210519691,5.91844162352147,
40.3799044157741));
#20462=CARTESIAN_POINT('Ctrl Pts',(0.079867361995723,5.91852383341869,40.3721176721605));
#20463=CARTESIAN_POINT('Ctrl Pts',(0.245171930862612,5.91166823213356,40.3643309285469));
#20464=CARTESIAN_POINT('Ctrl Pts',(0.410465566068641,5.90481308429517,40.3565446999682));
#20465=CARTESIAN_POINT('Ctrl Pts',(0.575471105891679,5.89102105692617,40.3487584713894));
#20466=CARTESIAN_POINT('Ctrl Pts',(0.739598897850327,5.87034275258256,40.3409722428106));
#20467=CARTESIAN_POINT('Ctrl Pts',(0.903769895860926,5.84965900474957,40.3331839645352));
#20468=CARTESIAN_POINT('Ctrl Pts',(1.06706236679312,5.82208539564029,40.3253956862597));
#20469=CARTESIAN_POINT('Ctrl Pts',(1.22889314019929,5.78772426887038,40.3176074079842));
#20470=CARTESIAN_POINT('Ctrl Pts',(1.38274581315085,5.75505711238395,40.3102030842876));
#20471=CARTESIAN_POINT('Ctrl Pts',(1.53527717971602,5.71625560809119,40.302798760591));
#20472=CARTESIAN_POINT('Ctrl Pts',(1.68599585087666,5.67145030422789,40.2953944368944));
#20473=CARTESIAN_POINT('Ctrl Pts',(1.84452399029271,5.62432341939856,40.2876064591328));
#20474=CARTESIAN_POINT('Ctrl Pts',(2.00110330642086,5.57053718620394,40.2798184813711));
#20475=CARTESIAN_POINT('Ctrl Pts',(2.15517227522717,5.51027794458611,40.2720305036095));
#20476=CARTESIAN_POINT('Ctrl Pts',(2.30921095275264,5.45003055045208,40.2642440570311));
#20477=CARTESIAN_POINT('Ctrl Pts',(2.46073997033066,5.38331280352874,40.2564576104528));
#20478=CARTESIAN_POINT('Ctrl Pts',(2.60921633746004,5.31035974928551,40.2486711638744));
#20479=CARTESIAN_POINT('Ctrl Pts',(2.75769836862895,5.23740391204731,40.2408844202606));
#20480=CARTESIAN_POINT('Ctrl Pts',(2.9031272277931,5.15821242888512,40.2330976766468));
#20481=CARTESIAN_POINT('Ctrl Pts',(3.04498248363186,5.07306734006904,40.225310933033));
#20482=CARTESIAN_POINT('Ctrl Pts',(3.18682835680653,4.9879278829637,40.217524704454));
#20483=CARTESIAN_POINT('Ctrl Pts',(3.32510082571255,4.89683577279358,40.209738475875));
#20484=CARTESIAN_POINT('Ctrl Pts',(3.4593063994134,4.80011768579454,40.2019522472961));
#20485=CARTESIAN_POINT('Ctrl Pts',(3.59354730224935,4.70337413810659,40.1941639690204));
#20486=CARTESIAN_POINT('Ctrl Pts',(3.72371891004499,4.60100183957025,40.1863756907447));
#20487=CARTESIAN_POINT('Ctrl Pts',(3.84935818982042,4.49336979214514,40.1785874124691));
#20488=CARTESIAN_POINT('Ctrl Pts',(3.96880357472292,4.39104390046926,40.1711830887733));
#20489=CARTESIAN_POINT('Ctrl Pts',(4.08415254558197,4.28396454000282,40.1637787650775));
#20490=CARTESIAN_POINT('Ctrl Pts',(4.19503615380803,4.17248154348746,40.1563744413817));
#20491=CARTESIAN_POINT('Ctrl Pts',(4.31166518171814,4.0552220700621,40.1485864636202));
#20492=CARTESIAN_POINT('Ctrl Pts',(4.42339553742123,3.93304855110767,40.1407984858588));
#20493=CARTESIAN_POINT('Ctrl Pts',(4.5298233997066,3.80639337562088,40.1330105080973));
#20494=CARTESIAN_POINT('Ctrl Pts',(4.63623033736126,3.6797631016281,40.1252240615191));
#20495=CARTESIAN_POINT('Ctrl Pts',(4.73733665627559,3.54865317371616,40.1174376149409));
#20496=CARTESIAN_POINT('Ctrl Pts',(4.83277812135753,3.41352987276046,40.1096511683627));
#20497=CARTESIAN_POINT('Ctrl Pts',(4.92822322731687,3.27840141715449,40.1018644247491));
#20498=CARTESIAN_POINT('Ctrl Pts',(5.01800285944072,3.13925954086346,40.0940776811355));
#20499=CARTESIAN_POINT('Ctrl Pts',(5.10179508439075,2.99660098768361,40.0862909375218));
#20500=CARTESIAN_POINT('Ctrl Pts',(5.18558176711191,2.85395187029991,40.078504708943));
#20501=CARTESIAN_POINT('Ctrl Pts',(5.26338167340363,2.70778681711519,40.0707184803642));
#20502=CARTESIAN_POINT('Ctrl Pts',(5.3349178892649,2.55862886665912,40.0629322517854));
#20503=CARTESIAN_POINT('Ctrl Pts',(5.40647293677808,2.40943165090829,40.0551439735099));
#20504=CARTESIAN_POINT('Ctrl Pts',(5.4717608589818,2.25724025102981,40.0473556952344));
#20505=CARTESIAN_POINT('Ctrl Pts',(5.53055174379081,2.10260028815569,40.0395674169589));
#20506=CARTESIAN_POINT('Ctrl Pts',(5.58644429489555,1.95558392574076,40.0321630932624));
#20507=CARTESIAN_POINT('Ctrl Pts',(5.63646487922549,1.80635485463067,40.0247587695658));
#20508=CARTESIAN_POINT('Ctrl Pts',(5.68045701476837,1.65539683033067,40.0173544458693));
#20509=CARTESIAN_POINT('Ctrl Pts',(5.72672859706751,1.49661693572192,40.0095664681077));
#20510=CARTESIAN_POINT('Ctrl Pts',(5.76634697001505,1.3358673613977,40.0017784903461));
#20511=CARTESIAN_POINT('Ctrl Pts',(5.79916455054649,1.1737210393381,39.9939905125845));
#20512=CARTESIAN_POINT('Ctrl Pts',(5.83197567886009,1.01160659663632,39.9862040660061));
#20513=CARTESIAN_POINT('Ctrl Pts',(5.857988619303,0.848096267139428,39.9784176194277));
#20514=CARTESIAN_POINT('Ctrl Pts',(5.87710676821336,0.68377379119174,39.9706311728493));
#20515=CARTESIAN_POINT('Ctrl Pts',(5.89622564643809,0.519445046711268,39.9628444292356));
#20516=CARTESIAN_POINT('Ctrl Pts',(5.9084491659655,0.354304410726337,39.9550576856218));
#20517=CARTESIAN_POINT('Ctrl Pts',(5.91373244552398,0.188942121447266,39.947270942008));
#20518=CARTESIAN_POINT('Ctrl Pts',(5.91901537563306,0.023590769645819,39.939484713429));
#20519=CARTESIAN_POINT('Ctrl Pts',(5.91735897429893,-0.141981886694097,
39.93169848485));
#20520=CARTESIAN_POINT('Ctrl Pts',(5.90877047349355,-0.307184071967987,
39.923912256271));
#20521=CARTESIAN_POINT('Ctrl Pts',(5.90017971179623,-0.472429746122778,
39.9161239779954));
#20522=CARTESIAN_POINT('Ctrl Pts',(5.88465321884044,-0.637304434902332,
39.9083356997197));
#20523=CARTESIAN_POINT('Ctrl Pts',(5.86225030366254,-0.801219033541034,
39.900547421444));
#20524=CARTESIAN_POINT('Ctrl Pts',(5.84095183051669,-0.95705280113766,39.8931430977483));
#20525=CARTESIAN_POINT('Ctrl Pts',(5.81343864062051,-1.1120186002606,39.8857387740525));
#20526=CARTESIAN_POINT('Ctrl Pts',(5.7798049012923,-1.2656167925156,39.8783344503567));
#20527=CARTESIAN_POINT('Ctrl Pts',(5.74442843415169,-1.42717365505005,39.8705464725952));
#20528=CARTESIAN_POINT('Ctrl Pts',(5.70226765216034,-1.58727521525857,39.8627584948338));
#20529=CARTESIAN_POINT('Ctrl Pts',(5.65346722174493,-1.74534779776285,39.8549705170723));
#20530=CARTESIAN_POINT('Ctrl Pts',(5.60467638591247,-1.9033893018424,39.8471840704941));
#20531=CARTESIAN_POINT('Ctrl Pts',(5.54924860054122,-2.05940231902604,39.8393976239158));
#20532=CARTESIAN_POINT('Ctrl Pts',(5.48737846539814,-2.21282808640544,39.8316111773375));
#20533=CARTESIAN_POINT('Ctrl Pts',(5.42550597004899,-2.36625970663171,39.8238244337239));
#20534=CARTESIAN_POINT('Ctrl Pts',(5.35719074899398,-2.51710358172856,39.8160376901103));
#20535=CARTESIAN_POINT('Ctrl Pts',(5.28267592438608,-2.66482000150323,39.8082509464966));
#20536=CARTESIAN_POINT('Ctrl Pts',(5.20816602837638,-2.8125266509418,39.8004647179178));
#20537=CARTESIAN_POINT('Ctrl Pts',(5.12745749343406,-2.9571059737336,39.792678489339));
#20538=CARTESIAN_POINT('Ctrl Pts',(5.04083993285009,-3.09804185476631,39.7848922607602));
#20539=CARTESIAN_POINT('Ctrl Pts',(4.95419957050444,-3.23901483666345,39.7771039824847));
#20540=CARTESIAN_POINT('Ctrl Pts',(4.86164724000419,-3.37634218682199,39.7693157042092));
#20541=CARTESIAN_POINT('Ctrl Pts',(4.7635169996695,-3.50953506270556,39.7615274259337));
#20542=CARTESIAN_POINT('Ctrl Pts',(4.67022448518173,-3.63616165875438,39.7541231022373));
#20543=CARTESIAN_POINT('Ctrl Pts',(4.57189094021556,-3.75905139980351,39.7467187785408));
#20544=CARTESIAN_POINT('Ctrl Pts',(4.46883820390687,-3.87781067998457,39.7393144548443));
#20545=CARTESIAN_POINT('Ctrl Pts',(4.36044580352792,-4.00272345675493,39.7315264770827));
#20546=CARTESIAN_POINT('Ctrl Pts',(4.24679340514233,-4.12311105354791,39.7237384993211));
#20547=CARTESIAN_POINT('Ctrl Pts',(4.12828262500392,-4.23853903256662,39.7159505215595));
#20548=CARTESIAN_POINT('Ctrl Pts',(4.00979514510056,-4.35394431745539,39.708164074981));
#20549=CARTESIAN_POINT('Ctrl Pts',(3.88645141812188,-4.46439170736599,39.7003776284026));
#20550=CARTESIAN_POINT('Ctrl Pts',(3.75868976350009,-4.56948375905415,39.6925911818242));
#20551=CARTESIAN_POINT('Ctrl Pts',(3.63092323505921,-4.67457981976716,39.6848044382104));
#20552=CARTESIAN_POINT('Ctrl Pts',(3.4987386860025,-4.7743199274167,39.6770176945966));
#20553=CARTESIAN_POINT('Ctrl Pts',(3.36260791832758,-4.86834659305402,39.6692309509828));
#20554=CARTESIAN_POINT('Ctrl Pts',(3.22648615468537,-4.96236703953025,39.6614447224038));
#20555=CARTESIAN_POINT('Ctrl Pts',(3.08641895776537,-5.05067461870308,39.6536584938249));
#20556=CARTESIAN_POINT('Ctrl Pts',(2.94290765442067,-5.13295481180696,39.645872265246));
#20557=CARTESIAN_POINT('Ctrl Pts',(2.79935857224034,-5.21525666487643,39.6380839869703));
#20558=CARTESIAN_POINT('Ctrl Pts',(2.65236384839128,-5.29152780059809,39.6302957086946));
#20559=CARTESIAN_POINT('Ctrl Pts',(2.50245077780901,-5.3614989198118,39.622507430419));
#20560=CARTESIAN_POINT('Ctrl Pts',(2.35992827648972,-5.42802053058072,39.6151031067232));
#20561=CARTESIAN_POINT('Ctrl Pts',(2.21476847919791,-5.48884821972119,39.6076987830274));
#20562=CARTESIAN_POINT('Ctrl Pts',(2.06744236578854,-5.5437904565958,39.6002944593317));
#20563=CARTESIAN_POINT('Ctrl Pts',(1.91248256904622,-5.60157951830139,39.5925064815702));
#20564=CARTESIAN_POINT('Ctrl Pts',(1.75507056904914,-5.65287769932322,39.5847185038088));
#20565=CARTESIAN_POINT('Ctrl Pts',(1.5957669345808,-5.69749580543932,39.5769305260473));
#20566=CARTESIAN_POINT('Ctrl Pts',(1.4364946205718,-5.7421051392535,39.569144079469));
#20567=CARTESIAN_POINT('Ctrl Pts',(1.27533172168438,-5.78003693257096,39.5613576328907));
#20568=CARTESIAN_POINT('Ctrl Pts',(1.11285332387517,-5.81115204086419,39.5535711863125));
#20569=CARTESIAN_POINT('Ctrl Pts',(0.950368727881924,-5.84226833612854,
39.5457844426988));
#20570=CARTESIAN_POINT('Ctrl Pts',(0.786568845641503,-5.8665673620375,39.5379976990851));
#20571=CARTESIAN_POINT('Ctrl Pts',(0.622039035864958,-5.88396108079924,
39.5302109554715));
#20572=CARTESIAN_POINT('Ctrl Pts',(0.457520108504363,-5.90135364909662,
39.5224247268927));
#20573=CARTESIAN_POINT('Ctrl Pts',(0.292271668039328,-5.9118417907557,39.5146384983139));
#20574=CARTESIAN_POINT('Ctrl Pts',(0.126884427473591,-5.91538932823231,
39.506852269735));
#20575=CARTESIAN_POINT('Ctrl Pts',(-0.0385463506887493,-5.91893779958541,
39.4990639914595));
#20576=CARTESIAN_POINT('Ctrl Pts',(-0.204115682316106,-5.91554200703426,
39.491275713184));
#20577=CARTESIAN_POINT('Ctrl Pts',(-0.369231699670738,-5.90521790575574,
39.4834874349085));
#20578=CARTESIAN_POINT('Ctrl Pts',(-0.526207657220763,-5.89540277267536,
39.4760831112121));
#20579=CARTESIAN_POINT('Ctrl Pts',(-0.68277365677089,-5.87932600977436,
39.4686787875156));
#20580=CARTESIAN_POINT('Ctrl Pts',(-0.838424500269211,-5.85704489651977,
39.4612744638192));
#20581=CARTESIAN_POINT('Ctrl Pts',(-1.00214037189203,-5.8336092902923,39.4534864860575));
#20582=CARTESIAN_POINT('Ctrl Pts',(-1.16490229652459,-5.80330092493929,
39.4456985082959));
#20583=CARTESIAN_POINT('Ctrl Pts',(-1.3261275357285,-5.76622201458482,39.4379105305343));
#20584=CARTESIAN_POINT('Ctrl Pts',(-1.48732107666961,-5.72915039426169,
39.4301240839558));
#20585=CARTESIAN_POINT('Ctrl Pts',(-1.64697822378216,-5.68531095654473,
39.4223376373773));
#20586=CARTESIAN_POINT('Ctrl Pts',(-1.80452744975621,-5.63485680790349,
39.4145511907989));
#20587=CARTESIAN_POINT('Ctrl Pts',(-1.96208268587634,-5.58440073455079,
39.4067644471851));
#20588=CARTESIAN_POINT('Ctrl Pts',(-2.11752953443022,-5.52732953903367,
39.3989777035713));
#20589=CARTESIAN_POINT('Ctrl Pts',(-2.27031191179147,-5.46384611658105,
39.3911909599575));
#20590=CARTESIAN_POINT('Ctrl Pts',(-2.42308418374147,-5.40036689308187,
39.3834047313786));
#20591=CARTESIAN_POINT('Ctrl Pts',(-2.57319204210018,-5.33047641410572,
39.3756185027996));
#20592=CARTESIAN_POINT('Ctrl Pts',(-2.72009952599787,-5.25442567091458,
39.3678322742207));
#20593=CARTESIAN_POINT('Ctrl Pts',(-2.86704568276299,-5.17835490763848,
39.360043995945));
#20594=CARTESIAN_POINT('Ctrl Pts',(-3.01078949673259,-5.09612078498146,
39.3522557176694));
#20595=CARTESIAN_POINT('Ctrl Pts',(-3.15081894741486,-5.00802061927779,
39.3444674393937));
#20596=CARTESIAN_POINT('Ctrl Pts',(-3.28394508172679,-4.92426370646248,
39.337063115698));
#20597=CARTESIAN_POINT('Ctrl Pts',(-3.41371403681091,-4.83520533901766,
39.3296587920023));
#20598=CARTESIAN_POINT('Ctrl Pts',(-3.53970966843084,-4.74113762990669,
39.3222544683066));
#20599=CARTESIAN_POINT('Ctrl Pts',(-3.67223374725513,-4.64219581472816,
39.3144664905452));
#20600=CARTESIAN_POINT('Ctrl Pts',(-3.80063049887293,-4.53767636537523,
39.3066785127838));
#20601=CARTESIAN_POINT('Ctrl Pts',(-3.92443720762358,-4.42794796332564,
39.2988905350224));
#20602=CARTESIAN_POINT('Ctrl Pts',(-4.04821957491413,-4.31824113482038,
39.2911040884441));
#20603=CARTESIAN_POINT('Ctrl Pts',(-4.16741346097805,-4.20332760886863,
39.2833176418659));
#20604=CARTESIAN_POINT('Ctrl Pts',(-4.28159035398739,-4.0836153838409,39.2755311952876));
#20605=CARTESIAN_POINT('Ctrl Pts',(-4.39577160258792,-3.96389859206155,
39.267744451674));
#20606=CARTESIAN_POINT('Ctrl Pts',(-4.50493525176469,-3.83938296340247,
39.2599577080604));
#20607=CARTESIAN_POINT('Ctrl Pts',(-4.60869018143983,-3.71051281819644,
39.2521709644468));
#20608=CARTESIAN_POINT('Ctrl Pts',(-4.71243824850303,-3.58165119678587,
39.244384735868));
#20609=CARTESIAN_POINT('Ctrl Pts',(-4.81077811164378,-3.44843588419347,
39.2365985072891));
#20610=CARTESIAN_POINT('Ctrl Pts',(-4.90335934049069,-3.31134379678745,
39.2288122787103));
#20611=CARTESIAN_POINT('Ctrl Pts',(-4.99596494101312,-3.17421562038246,
39.2210240004348));
#20612=CARTESIAN_POINT('Ctrl Pts',(-5.08280869749645,-3.0332088937969,39.2132357221593));
#20613=CARTESIAN_POINT('Ctrl Pts',(-5.16358337343216,-2.88882974716666,
39.2054474438838));
#20614=CARTESIAN_POINT('Ctrl Pts',(-5.24037593604437,-2.75156835268795,
39.1980431201873));
#20615=CARTESIAN_POINT('Ctrl Pts',(-5.31168327443589,-2.61125927239488,
39.1906387964907));
#20616=CARTESIAN_POINT('Ctrl Pts',(-5.37727984041684,-2.46835817505213,
39.1832344727942));
#20617=CARTESIAN_POINT('Ctrl Pts',(-5.44600563262427,-2.31864010711172,
39.1754769323773));
#20618=CARTESIAN_POINT('Ctrl Pts',(-5.50848877556581,-2.16601916666619,
39.1677193919604));
#20619=CARTESIAN_POINT('Ctrl Pts',(-5.56450037895025,-2.01103607505249,
39.1599618515435));
#20620=CARTESIAN_POINT('Ctrl Pts',(-5.62261559505141,-1.85023232516988,
39.1519129632686));
#20621=CARTESIAN_POINT('Ctrl Pts',(-5.67376357479425,-1.6868858800762,39.1438640749937));
#20622=CARTESIAN_POINT('Ctrl Pts',(-5.71774411285594,-1.52162177376679,
39.1358151867188));
#20623=CARTESIAN_POINT('Ctrl Pts',(-5.76012303573033,-1.36237599998007,
39.1280594104036));
#20624=CARTESIAN_POINT('Ctrl Pts',(-5.79584726755631,-1.20135010997528,
39.1203036340885));
#20625=CARTESIAN_POINT('Ctrl Pts',(-5.82478889000928,-1.03911738957853,
39.1125478577733));
#20626=CARTESIAN_POINT('Ctrl Pts',(-5.85372943094268,-0.876890731656749,
39.1047923712838));
#20627=CARTESIAN_POINT('Ctrl Pts',(-5.87588781401548,-0.713457653276527,
39.0970368847942));
#20628=CARTESIAN_POINT('Ctrl Pts',(-5.89118746677025,-0.549400394857105,
39.0892813983047));
#20629=CARTESIAN_POINT('Ctrl Pts',(-5.90648969860401,-0.385315481128406,
39.0815246044644));
#20630=CARTESIAN_POINT('Ctrl Pts',(-5.91493086209221,-0.220606500444764,
39.0737678106242));
#20631=CARTESIAN_POINT('Ctrl Pts',(-5.91648630544981,-0.0558601819265851,
39.0660110167839));
#20632=CARTESIAN_POINT('Ctrl Pts',(-5.91666248974519,-0.0371994483791566,
39.0651324086042));
#20633=CARTESIAN_POINT('Ctrl Pts',(-5.91675038539335,-0.0185382371664036,
39.0642538004244));
#20634=CARTESIAN_POINT('Ctrl Pts',(-5.91674999872984,0.000122598544141182,
39.0633751922447));
#20635=CARTESIAN_POINT('Ctrl Pts',(-5.91674999852516,0.000132107828751824,
38.8116248077951));
#20636=CARTESIAN_POINT('Ctrl Pts',(-5.9167536915139,-0.165266803763928,
38.8194094218845));
#20637=CARTESIAN_POINT('Ctrl Pts',(-5.90981761062779,-0.330675236470803,
38.8271940359738));
#20638=CARTESIAN_POINT('Ctrl Pts',(-5.89596542934449,-0.495501986347875,
38.8349786500631));
#20639=CARTESIAN_POINT('Ctrl Pts',(-5.88211413062991,-0.660318234562368,
38.8427627681687));
#20640=CARTESIAN_POINT('Ctrl Pts',(-5.86134764036802,-0.824552555352156,
38.8505468862743));
#20641=CARTESIAN_POINT('Ctrl Pts',(-5.83374157440724,-0.987618248885952,
38.8583310043799));
#20642=CARTESIAN_POINT('Ctrl Pts',(-5.80612776919019,-1.1507296572707,38.8661173047336));
#20643=CARTESIAN_POINT('Ctrl Pts',(-5.77167060808896,-1.31267146776595,
38.8739036050873));
#20644=CARTESIAN_POINT('Ctrl Pts',(-5.73049713102611,-1.47286564010488,
38.881689905441));
#20645=CARTESIAN_POINT('Ctrl Pts',(-5.68943104611784,-1.63264198041826,
38.8894558969057));
#20646=CARTESIAN_POINT('Ctrl Pts',(-5.64168374426802,-1.79067948835634,
38.8972218883705));
#20647=CARTESIAN_POINT('Ctrl Pts',(-5.58743109435409,-1.94641833333565,
38.9049878798353));
#20648=CARTESIAN_POINT('Ctrl Pts',(-5.53302391623533,-2.10260077036387,
38.9127759912283));
#20649=CARTESIAN_POINT('Ctrl Pts',(-5.47205439836578,-2.25652843993273,
38.9205641026212));
#20650=CARTESIAN_POINT('Ctrl Pts',(-5.40473466168731,-2.40764901911715,
38.9283522140142));
#20651=CARTESIAN_POINT('Ctrl Pts',(-5.33742814206569,-2.55873992841001,
38.9361387963472));
#20652=CARTESIAN_POINT('Ctrl Pts',(-5.26377402122413,-2.70702455527588,
38.9439253786802));
#20653=CARTESIAN_POINT('Ctrl Pts',(-5.18403221618832,-2.85197134347834,
38.9517119610133));
#20654=CARTESIAN_POINT('Ctrl Pts',(-5.10428737061506,-2.99692365846989,
38.959498840247));
#20655=CARTESIAN_POINT('Ctrl Pts',(-5.01845452692368,-3.13853759827777,
38.9672857194807));
#20656=CARTESIAN_POINT('Ctrl Pts',(-4.92683950299966,-3.27630631568267,
38.9750725987144));
#20657=CARTESIAN_POINT('Ctrl Pts',(-4.83523052561402,-3.41406594043219,
38.9828589640186));
#20658=CARTESIAN_POINT('Ctrl Pts',(-4.73784030872284,-3.54798058461169,
38.9906453293228));
#20659=CARTESIAN_POINT('Ctrl Pts',(-4.63501801240989,-3.67757237687254,
38.998431694627));
#20660=CARTESIAN_POINT('Ctrl Pts',(-4.53216871705015,-3.80719819730614,
39.0062201044726));
#20661=CARTESIAN_POINT('Ctrl Pts',(-4.42388468933028,-3.93249864598739,
39.0140085143182));
#20662=CARTESIAN_POINT('Ctrl Pts',(-4.31055596035097,-4.05302823518203,
39.0217969241637));
#20663=CARTESIAN_POINT('Ctrl Pts',(-4.20318287806859,-4.16722375837033,
39.029176037816));
#20664=CARTESIAN_POINT('Ctrl Pts',(-4.09128185308816,-4.27713677143141,
39.0365551514682));
#20665=CARTESIAN_POINT('Ctrl Pts',(-3.9752156168088,-4.38241843761859,39.0439342651204));
#20666=CARTESIAN_POINT('Ctrl Pts',(-3.85271624632737,-4.49353548805973,
39.0517223765134));
#20667=CARTESIAN_POINT('Ctrl Pts',(-3.72553309577955,-4.59953292097697,
39.0595104879064));
#20668=CARTESIAN_POINT('Ctrl Pts',(-3.59411668417073,-4.70002721514095,
39.0672985992993));
#20669=CARTESIAN_POINT('Ctrl Pts',(-3.46272607388376,-4.80050177900188,
39.0750851816324));
#20670=CARTESIAN_POINT('Ctrl Pts',(-3.32710411454507,-4.89547516594232,
39.0828717639654));
#20671=CARTESIAN_POINT('Ctrl Pts',(-3.18773336047609,-4.98460495776825,
39.0906583462985));
#20672=CARTESIAN_POINT('Ctrl Pts',(-3.0483572922309,-5.07373814809355,39.0984452255322));
#20673=CARTESIAN_POINT('Ctrl Pts',(-2.9052324102819,-5.1570271219814,39.106232104766));
#20674=CARTESIAN_POINT('Ctrl Pts',(-2.75886975387813,-5.23417311937964,
39.1140189839997));
#20675=CARTESIAN_POINT('Ctrl Pts',(-2.61251675732482,-5.31131402518679,
39.1218053493039));
#20676=CARTESIAN_POINT('Ctrl Pts',(-2.46292669668928,-5.3823126169404,39.1295917146081));
#20677=CARTESIAN_POINT('Ctrl Pts',(-2.31063480791587,-5.44691631539788,
39.1373780799123));
#20678=CARTESIAN_POINT('Ctrl Pts',(-2.15830293038553,-5.51153697747447,
39.1451664897579));
#20679=CARTESIAN_POINT('Ctrl Pts',(-2.00326810068891,-5.56975926427218,
39.1529548996035));
#20680=CARTESIAN_POINT('Ctrl Pts',(-1.8460859510802,-5.62137858747517,39.1607433094491));
#20681=CARTESIAN_POINT('Ctrl Pts',(-1.69716403132471,-5.67028521413096,
39.1681224231012));
#20682=CARTESIAN_POINT('Ctrl Pts',(-1.54631492559119,-5.71326494343056,
39.1755015367534));
#20683=CARTESIAN_POINT('Ctrl Pts',(-1.39402405240194,-5.7501849973566,39.1828806504055));
#20684=CARTESIAN_POINT('Ctrl Pts',(-1.23329224361816,-5.78915139713915,
39.1906687617985));
#20685=CARTESIAN_POINT('Ctrl Pts',(-1.07089690620403,-5.82138125835975,
39.1984568731914));
#20686=CARTESIAN_POINT('Ctrl Pts',(-0.907417141262457,-5.84675334645161,
39.2062449845844));
#20687=CARTESIAN_POINT('Ctrl Pts',(-0.743969472723136,-5.87212045317623,
39.2140315669174));
#20688=CARTESIAN_POINT('Ctrl Pts',(-0.579438117025394,-5.89063242427489,
39.2218181492504));
#20689=CARTESIAN_POINT('Ctrl Pts',(-0.414410641072862,-5.90221944551925,
39.2296047315835));
#20690=CARTESIAN_POINT('Ctrl Pts',(-0.249376872659111,-5.91380690857418,
39.2373916108172));
#20691=CARTESIAN_POINT('Ctrl Pts',(-0.0838472645923005,-5.91846886709936,
39.2451784900509));
#20692=CARTESIAN_POINT('Ctrl Pts',(0.081586490553414,-5.91618747227124,
39.2529653692846));
#20693=CARTESIAN_POINT('Ctrl Pts',(0.247009327167273,-5.91390622801386,
39.2607517345888));
#20694=CARTESIAN_POINT('Ctrl Pts',(0.41233600399847,-5.90468255197068,39.268538099893));
#20695=CARTESIAN_POINT('Ctrl Pts',(0.576975675330162,-5.88855072429348,
39.2763244651972));
#20696=CARTESIAN_POINT('Ctrl Pts',(0.741658577696028,-5.87241466072594,
39.2841128750428));
#20697=CARTESIAN_POINT('Ctrl Pts',(0.905653795694052,-5.849366850141,39.2919012848884));
#20698=CARTESIAN_POINT('Ctrl Pts',(1.06837553369385,-5.81949347293254,39.299689694734));
#20699=CARTESIAN_POINT('Ctrl Pts',(1.2225459256214,-5.79119000021253,39.3070688083862));
#20700=CARTESIAN_POINT('Ctrl Pts',(1.37557298684746,-5.75675994990192,39.3144479220384));
#20701=CARTESIAN_POINT('Ctrl Pts',(1.52696693460137,-5.71631896793156,39.3218270356906));
#20702=CARTESIAN_POINT('Ctrl Pts',(1.68675210459546,-5.67363648772193,39.3296151470836));
#20703=CARTESIAN_POINT('Ctrl Pts',(1.84477505944887,-5.62424260847048,39.3374032584765));
#20704=CARTESIAN_POINT('Ctrl Pts',(2.00046927437237,-5.56830793372565,39.3451913698695));
#20705=CARTESIAN_POINT('Ctrl Pts',(2.15613292145087,-5.51238424077915,39.3529779522025));
#20706=CARTESIAN_POINT('Ctrl Pts',(2.30946844033886,-5.44992242260928,39.3607645345356));
#20707=CARTESIAN_POINT('Ctrl Pts',(2.4599264735374,-5.38114228647504,39.3685511168686));
#20708=CARTESIAN_POINT('Ctrl Pts',(2.61039024366752,-5.3123595277694,39.3763379961023));
#20709=CARTESIAN_POINT('Ctrl Pts',(2.75797601632913,-5.23725809827598,39.3841248753361));
#20710=CARTESIAN_POINT('Ctrl Pts',(2.90215567325997,-5.15610541112815,39.3919117545698));
#20711=CARTESIAN_POINT('Ctrl Pts',(3.04632581441721,-5.07495808001053,39.399698119874));
#20712=CARTESIAN_POINT('Ctrl Pts',(3.18709001129192,-4.98776044730135,39.4074844851782));
#20713=CARTESIAN_POINT('Ctrl Pts',(3.32394582960667,-4.89482529661074,39.4152708504824));
#20714=CARTESIAN_POINT('Ctrl Pts',(3.4608375834798,-4.80186574303705,39.423059260328));
#20715=CARTESIAN_POINT('Ctrl Pts',(3.59381864250501,-4.70316583908828,39.4308476701736));
#20716=CARTESIAN_POINT('Ctrl Pts',(3.72241583790705,-4.59908152702241,39.4386360800192));
#20717=CARTESIAN_POINT('Ctrl Pts',(3.84425499879354,-4.50046704943674,39.4460151936714));
#20718=CARTESIAN_POINT('Ctrl Pts',(3.96215900412751,-4.39701969394617,39.4533943073236));
#20719=CARTESIAN_POINT('Ctrl Pts',(4.07575309356943,-4.28907534123139,39.4607734209758));
#20720=CARTESIAN_POINT('Ctrl Pts',(4.19564329500173,-4.1751480211214,39.4685615323688));
#20721=CARTESIAN_POINT('Ctrl Pts',(4.31077508512322,-4.0561703741806,39.4763496437617));
#20722=CARTESIAN_POINT('Ctrl Pts',(4.42073260833838,-3.93256325671612,39.4841377551547));
#20723=CARTESIAN_POINT('Ctrl Pts',(4.53066854331052,-3.80898040735458,39.4919243374877));
#20724=CARTESIAN_POINT('Ctrl Pts',(4.63543202611002,-3.68077013961672,39.4997109198207));
#20725=CARTESIAN_POINT('Ctrl Pts',(4.73464581692109,-3.54838830327398,39.5074975021538));
#20726=CARTESIAN_POINT('Ctrl Pts',(4.83386339073217,-3.41600141924096,39.5152843813875));
#20727=CARTESIAN_POINT('Ctrl Pts',(4.92753065434675,-3.27944290163392,39.5230712606212));
#20728=CARTESIAN_POINT('Ctrl Pts',(5.01531179493667,-3.13920024242944,39.5308581398549));
#20729=CARTESIAN_POINT('Ctrl Pts',(5.10308714202204,-2.99896683915944,39.5386445051591));
#20730=CARTESIAN_POINT('Ctrl Pts',(5.18497697404958,-2.85505005180575,39.5464308704633));
#20731=CARTESIAN_POINT('Ctrl Pts',(5.26068973872044,-2.70796492507224,39.5542172357675));
#20732=CARTESIAN_POINT('Ctrl Pts',(5.33642238402598,-2.56084117677096,39.5620056456131));
#20733=CARTESIAN_POINT('Ctrl Pts',(5.40597457287245,-2.41054771009415,39.5697940554587));
#20734=CARTESIAN_POINT('Ctrl Pts',(5.4691011002856,-2.2576234666912,39.5775824653043));
#20735=CARTESIAN_POINT('Ctrl Pts',(5.52891020503042,-2.11273569182839,39.5849615789565));
#20736=CARTESIAN_POINT('Ctrl Pts',(5.5829515406437,-1.96548677374418,39.5923406926087));
#20737=CARTESIAN_POINT('Ctrl Pts',(5.63105671867893,-1.81635095549315,39.5997198062609));
#20738=CARTESIAN_POINT('Ctrl Pts',(5.68182819378697,-1.65894907500318,39.6075079176538));
#20739=CARTESIAN_POINT('Ctrl Pts',(5.72600494485602,-1.49938897901227,39.6152960290467));
#20740=CARTESIAN_POINT('Ctrl Pts',(5.76342315209342,-1.33823919103186,39.6230841404395));
#20741=CARTESIAN_POINT('Ctrl Pts',(5.80083401291802,-1.1771210420035,39.6308707227725));
#20742=CARTESIAN_POINT('Ctrl Pts',(5.83148890528973,-1.01441413479051,39.6386573051055));
#20743=CARTESIAN_POINT('Ctrl Pts',(5.85527466092086,-0.850699246313389,
39.6464438874384));
#20744=CARTESIAN_POINT('Ctrl Pts',(5.87906132349765,-0.686978115423271,
39.6542307666721));
#20745=CARTESIAN_POINT('Ctrl Pts',(5.8959782753877,-0.52224924199067,39.6620176459057));
#20746=CARTESIAN_POINT('Ctrl Pts',(5.90596386503354,-0.357101368546964,
39.6698045251393));
#20747=CARTESIAN_POINT('Ctrl Pts',(5.9159487956362,-0.191964394767925,39.6775908904434));
#20748=CARTESIAN_POINT('Ctrl Pts',(5.91900326028553,-0.0264087952951148,
39.6853772557475));
#20749=CARTESIAN_POINT('Ctrl Pts',(5.91511765580153,0.138973668459359,39.6931636210516));
#20750=CARTESIAN_POINT('Ctrl Pts',(5.91123103103668,0.30439955829094,39.7009520308971));
#20751=CARTESIAN_POINT('Ctrl Pts',(5.90040070133012,0.469651901865704,39.7087404407427));
#20752=CARTESIAN_POINT('Ctrl Pts',(5.88266919528697,0.634140127512631,39.7165288505882));
#20753=CARTESIAN_POINT('Ctrl Pts',(5.865869514618,0.789984174710317,39.7239079642408));
#20754=CARTESIAN_POINT('Ctrl Pts',(5.8428753700362,0.945142091521705,39.7312870778934));
#20755=CARTESIAN_POINT('Ctrl Pts',(5.81376579040385,1.09911687132437,39.738666191546));
#20756=CARTESIAN_POINT('Ctrl Pts',(5.7830427714266,1.26162591960481,39.7464543029391));
#20757=CARTESIAN_POINT('Ctrl Pts',(5.74549620833344,1.42287499764621,39.7542424143322));
#20758=CARTESIAN_POINT('Ctrl Pts',(5.70125424892118,1.58228649481003,39.7620305257253));
#20759=CARTESIAN_POINT('Ctrl Pts',(5.65702097564673,1.74166669430414,39.7698171080585));
#20760=CARTESIAN_POINT('Ctrl Pts',(5.60609501431728,1.89920972507734,39.7776036903916));
#20761=CARTESIAN_POINT('Ctrl Pts',(5.54865485343531,2.05435144995903,39.7853902727248));
#20762=CARTESIAN_POINT('Ctrl Pts',(5.49121250237248,2.209499090361,39.7931771519586));
#20763=CARTESIAN_POINT('Ctrl Pts',(5.42725556197475,2.36224494064844,39.8009640311925));
#20764=CARTESIAN_POINT('Ctrl Pts',(5.3570115697905,2.51204251628645,39.8087509104263));
#20765=CARTESIAN_POINT('Ctrl Pts',(5.28677221366921,2.66183020537087,39.8165372757307));
#20766=CARTESIAN_POINT('Ctrl Pts',(5.21024677190148,2.8086697199264,39.824323641035));
#20767=CARTESIAN_POINT('Ctrl Pts',(5.12770993124302,2.95203682624924,39.8321100063393));
#20768=CARTESIAN_POINT('Ctrl Pts',(5.04515141808631,3.09544157786278,39.839898416185));
#20769=CARTESIAN_POINT('Ctrl Pts',(4.95657850976868,3.23537182124153,39.8476868260307));
#20770=CARTESIAN_POINT('Ctrl Pts',(4.86231110194224,3.37132930910483,39.8554752358764));
#20771=CARTESIAN_POINT('Ctrl Pts',(4.77299763105797,3.50014196465312,39.862854349528));
#20772=CARTESIAN_POINT('Ctrl Pts',(4.67857292898766,3.6253884634724,39.8702334631796));
#20773=CARTESIAN_POINT('Ctrl Pts',(4.57934417827356,3.74667018289735,39.8776125768312));
#20774=CARTESIAN_POINT('Ctrl Pts',(4.47461553464101,3.87467411201458,39.8854006882241));
#20775=CARTESIAN_POINT('Ctrl Pts',(4.36449779535653,3.99830700837581,39.893188799617));
#20776=CARTESIAN_POINT('Ctrl Pts',(4.24937983922382,4.1171229693195,39.9009769110099));
#20777=CARTESIAN_POINT('Ctrl Pts',(4.13428448449529,4.2359156028202,39.9087634933429));
#20778=CARTESIAN_POINT('Ctrl Pts',(4.01419109391674,4.34989295855654,39.9165500756759));
#20779=CARTESIAN_POINT('Ctrl Pts',(3.88952630543241,4.45864504999549,39.9243366580089));
#20780=CARTESIAN_POINT('Ctrl Pts',(3.76485676350681,4.56740128812804,39.9321235372425));
#20781=CARTESIAN_POINT('Ctrl Pts',(3.635615713068,4.6709316502703,39.9399104164762));
#20782=CARTESIAN_POINT('Ctrl Pts',(3.50226441750365,4.76886511786482,39.9476972957099));
#20783=CARTESIAN_POINT('Ctrl Pts',(3.36892192304767,4.86679212190712,39.955483661014));
#20784=CARTESIAN_POINT('Ctrl Pts',(3.23146998395461,4.95912278155527,39.9632700263182));
#20785=CARTESIAN_POINT('Ctrl Pts',(3.09040062082509,5.04552817505798,39.9710563916224));
#20786=CARTESIAN_POINT('Ctrl Pts',(2.94929421574576,5.13195625686223,39.9788448014679));
#20787=CARTESIAN_POINT('Ctrl Pts',(2.80456876025181,5.21245579493993,39.9866332113135));
#20788=CARTESIAN_POINT('Ctrl Pts',(2.65674354108654,5.28674231634141,39.994421621159));
#20789=CARTESIAN_POINT('Ctrl Pts',(2.51668682674466,5.35712493553271,40.0018007348115));
#20790=CARTESIAN_POINT('Ctrl Pts',(2.37384799876125,5.42193063785565,40.0091798484639));
#20791=CARTESIAN_POINT('Ctrl Pts',(2.22868751627878,5.48095635060918,40.0165589621163));
#20792=CARTESIAN_POINT('Ctrl Pts',(2.07548131013064,5.54325364641247,40.0243470735092));
#20793=CARTESIAN_POINT('Ctrl Pts',(1.91963407228572,5.59913430517782,40.0321351849022));
#20794=CARTESIAN_POINT('Ctrl Pts',(1.76170062165578,5.6483928229327,40.0399232962951));
#20795=CARTESIAN_POINT('Ctrl Pts',(1.60379817850537,5.69764166963643,40.0477098786281));
#20796=CARTESIAN_POINT('Ctrl Pts',(1.44381064467451,5.74027087441918,40.0554964609612));
#20797=CARTESIAN_POINT('Ctrl Pts',(1.28230881269572,5.77612453738516,40.0632830432942));
#20798=CARTESIAN_POINT('Ctrl Pts',(1.12080082268818,5.81197956744329,40.0710699225279));
#20799=CARTESIAN_POINT('Ctrl Pts',(0.957778730061289,5.8410584656247,40.0788568017616));
#20800=CARTESIAN_POINT('Ctrl Pts',(0.793825089086202,5.86325611673559,40.0866436809953));
#20801=CARTESIAN_POINT('Ctrl Pts',(0.629882268956349,5.88545230281437,40.0944300462994));
#20802=CARTESIAN_POINT('Ctrl Pts',(0.465008340192592,5.90076810790694,40.1022164116036));
#20803=CARTESIAN_POINT('Ctrl Pts',(0.299792725080259,5.90915009832116,40.1100027769077));
#20804=CARTESIAN_POINT('Ctrl Pts',(0.134533727702779,5.91753428967583,40.1177911867533));
#20805=CARTESIAN_POINT('Ctrl Pts',(-0.0310668160726866,5.91898101011672,
40.1255795965989));
#20806=CARTESIAN_POINT('Ctrl Pts',(-0.196416806812622,5.9134889025432,40.1333680064444));
#20807=CARTESIAN_POINT('Ctrl Pts',(-0.353077331653457,5.90828541598054,
40.1407471200967));
#20808=CARTESIAN_POINT('Ctrl Pts',(-0.509512700296116,5.89685365014063,
40.1481262337491));
#20809=CARTESIAN_POINT('Ctrl Pts',(-0.665221415915665,5.87923558214052,
40.1555053474014));
#20810=CARTESIAN_POINT('Ctrl Pts',(-0.829560505843994,5.86064100797096,
40.1632934587944));
#20811=CARTESIAN_POINT('Ctrl Pts',(-0.993148800557225,5.83514827565258,
40.1710815701873));
#20812=CARTESIAN_POINT('Ctrl Pts',(-1.1554007805571,5.80284237238856,40.1788696815803));
#20813=CARTESIAN_POINT('Ctrl Pts',(-1.31762090520955,5.77054281182538,40.1866562639134));
#20814=CARTESIAN_POINT('Ctrl Pts',(-1.47850492545557,5.73143281167847,40.1944428462465));
#20815=CARTESIAN_POINT('Ctrl Pts',(-1.63747702733532,5.6856485599665,40.2022294285796));
#20816=CARTESIAN_POINT('Ctrl Pts',(-1.79645519078654,5.63986256251102,40.2100163078133));
#20817=CARTESIAN_POINT('Ctrl Pts',(-1.9535209818679,5.58740188889311,40.2178031870471));
#20818=CARTESIAN_POINT('Ctrl Pts',(-2.10811255556077,5.52845294956799,40.2255900662808));
#20819=CARTESIAN_POINT('Ctrl Pts',(-2.26269392629927,5.46950790083875,40.2333764315851));
#20820=CARTESIAN_POINT('Ctrl Pts',(-2.41480110789138,5.40407555730555,40.2411627968893));
#20821=CARTESIAN_POINT('Ctrl Pts',(-2.56389095061131,5.33239099803019,40.2489491621936));
#20822=CARTESIAN_POINT('Ctrl Pts',(-2.71301994129586,5.26068761584551,40.2567375720392));
#20823=CARTESIAN_POINT('Ctrl Pts',(-2.85912972094247,5.18272887425217,40.2645259818848));
#20824=CARTESIAN_POINT('Ctrl Pts',(-3.0016997042382,5.09879686279776,40.2723143917305));
#20825=CARTESIAN_POINT('Ctrl Pts',(-3.13677735564056,5.01927564295431,40.2796935053825));
#20826=CARTESIAN_POINT('Ctrl Pts',(-3.26867746380742,4.93439295157321,40.2870726190345));
#20827=CARTESIAN_POINT('Ctrl Pts',(-3.39697973626252,4.84442558348478,40.2944517326865));
#20828=CARTESIAN_POINT('Ctrl Pts',(-3.53239334241727,4.74947164762701,40.3022398440794));
#20829=CARTESIAN_POINT('Ctrl Pts',(-3.6638473360425,4.64881948854476,40.3100279554724));
#20830=CARTESIAN_POINT('Ctrl Pts',(-3.79086821997638,4.54282386861665,40.3178160668653));
#20831=CARTESIAN_POINT('Ctrl Pts',(-3.91786416557537,4.43684905907959,40.3256026491984));
#20832=CARTESIAN_POINT('Ctrl Pts',(-4.04042849293809,4.32553308654958,40.3333892315315));
#20833=CARTESIAN_POINT('Ctrl Pts',(-4.15812072383325,4.20927103053824,40.3411758138646));
#20834=CARTESIAN_POINT('Ctrl Pts',(-4.27581744230611,4.09300454148144,40.3489626930983));
#20835=CARTESIAN_POINT('Ctrl Pts',(-4.38864146249824,3.97179181330609,40.356749572332));
#20836=CARTESIAN_POINT('Ctrl Pts',(-4.49618860080912,3.84606534375772,40.3645364515657));
#20837=CARTESIAN_POINT('Ctrl Pts',(-4.60372864107145,3.72034717208317,40.3723228168699));
#20838=CARTESIAN_POINT('Ctrl Pts',(-4.70599228876691,3.59011609809584,40.3801091821741));
#20839=CARTESIAN_POINT('Ctrl Pts',(-4.80261506183598,3.45583841206822,40.3878955474783));
#20840=CARTESIAN_POINT('Ctrl Pts',(-4.89926320608298,3.32152546744725,40.3956839573239));
#20841=CARTESIAN_POINT('Ctrl Pts',(-4.99026732767116,3.18316404597082,40.4034723671695));
#20842=CARTESIAN_POINT('Ctrl Pts',(-5.07530525034122,3.04125092328122,40.4112607770151));
#20843=CARTESIAN_POINT('Ctrl Pts',(-5.15587426360153,2.90679561317031,40.4186398906673));
#20844=CARTESIAN_POINT('Ctrl Pts',(-5.23108788656526,2.76915252125431,40.4260190043195));
#20845=CARTESIAN_POINT('Ctrl Pts',(-5.30070947922281,2.62876579013374,40.4333981179716));
#20846=CARTESIAN_POINT('Ctrl Pts',(-5.37397943633849,2.48102240512659,40.4411639176353));
#20847=CARTESIAN_POINT('Ctrl Pts',(-5.44108311045085,2.3301844437189,40.448929717299));
#20848=CARTESIAN_POINT('Ctrl Pts',(-5.50177518626529,2.1767867057421,40.4566955169627));
#20849=CARTESIAN_POINT('Ctrl Pts',(-5.562454740084,2.0234206168034,40.4644597143858));
#20850=CARTESIAN_POINT('Ctrl Pts',(-5.61672521602865,1.86749610535429,40.4722239118089));
#20851=CARTESIAN_POINT('Ctrl Pts',(-5.66438955980109,1.7095676287636,40.4799881092319));
#20852=CARTESIAN_POINT('Ctrl Pts',(-5.712054462803,1.55163729925204,40.4877523977497));
#20853=CARTESIAN_POINT('Ctrl Pts',(-5.75311298151021,1.39170326583823,40.4955166862674));
#20854=CARTESIAN_POINT('Ctrl Pts',(-5.78741783925445,1.23033544872096,40.5032809747851));
#20855=CARTESIAN_POINT('Ctrl Pts',(-5.82172103481773,1.06897545039469,40.5110448870981));
#20856=CARTESIAN_POINT('Ctrl Pts',(-5.8492711578878,0.90618212369588,40.518808799411));
#20857=CARTESIAN_POINT('Ctrl Pts',(-5.86997195585913,0.742536059681504,
40.5265727117239));
#20858=CARTESIAN_POINT('Ctrl Pts',(-5.89067724266346,0.578854510085715,
40.5343383075906));
#20859=CARTESIAN_POINT('Ctrl Pts',(-5.904530196549,0.414320174490498,40.5421039034572));
#20860=CARTESIAN_POINT('Ctrl Pts',(-5.9114863050132,0.249519995474125,40.5498694993239));
#20861=CARTESIAN_POINT('Ctrl Pts',(-5.91499628252033,0.166363597827879,
40.553787935467));
#20862=CARTESIAN_POINT('Ctrl Pts',(-5.91675107512313,0.0831395781098299,
40.5577063716101));
#20863=CARTESIAN_POINT('Ctrl Pts',(-5.91674999950574,-7.64775397288306E-5,
40.5616248077532));
#20864=CARTESIAN_POINT('Origin',(0.,0.,0.));
#20865=CARTESIAN_POINT('',(-5.91650634169521,0.000138707710825164,42.5633751922049));
#20866=CARTESIAN_POINT('',(-5.91670122177708,-1.61732529071579E-5,42.3116248079793));
#20867=CARTESIAN_POINT('',(-5.91675,-7.2459289488551E-16,0.));
#20868=CARTESIAN_POINT('Ctrl Pts',(-5.91650634169521,0.000138707710825164,
42.5633751922049));
#20869=CARTESIAN_POINT('Ctrl Pts',(-5.91677370638019,0.309337923053453,
42.5488215831681));
#20870=CARTESIAN_POINT('Ctrl Pts',(-5.81712789539372,1.60288454477205,42.4879279756271));
#20871=CARTESIAN_POINT('Ctrl Pts',(-4.88823415802477,3.76173700716183,42.380694369582));
#20872=CARTESIAN_POINT('Ctrl Pts',(-2.49123115743396,5.64262933524277,42.2416743740696));
#20873=CARTESIAN_POINT('Ctrl Pts',(0.513650429588109,6.14667891880822,42.102654378557));
#20874=CARTESIAN_POINT('Ctrl Pts',(3.39319756254412,5.1508939802966,41.9636343830446));
#20875=CARTESIAN_POINT('Ctrl Pts',(5.44477972259265,2.89825331314937,41.8246143875318));
#20876=CARTESIAN_POINT('Ctrl Pts',(6.16779588774671,-0.0615823173574553,
41.6855943920195));
#20877=CARTESIAN_POINT('Ctrl Pts',(5.38582483627265,-3.00639141292502,41.546574396507));
#20878=CARTESIAN_POINT('Ctrl Pts',(3.28967321249204,-5.21761905947031,41.4075544009944));
#20879=CARTESIAN_POINT('Ctrl Pts',(0.39081731286073,-6.15570957101441,41.268534405482));
#20880=CARTESIAN_POINT('Ctrl Pts',(-2.60340086377102,-5.59176201543438,
41.1295144099693));
#20881=CARTESIAN_POINT('Ctrl Pts',(-4.96237022687324,-3.6633837126559,40.9904944144569));
#20882=CARTESIAN_POINT('Ctrl Pts',(-5.83266256480556,-1.52405015064227,
40.8851146769589));
#20883=CARTESIAN_POINT('Ctrl Pts',(-5.91687951771807,-0.269949220235747,
40.8260749379652));
#20884=CARTESIAN_POINT('Ctrl Pts',(-5.91661801913444,-0.000151051921165636,
40.8133751974756));
#20885=CARTESIAN_POINT('Ctrl Pts',(-5.91674999950573,-7.64784292123484E-5,
40.5616248077951));
#20886=CARTESIAN_POINT('Ctrl Pts',(-5.9167490186361,-0.075961409857763,
40.5651980396157));
#20887=CARTESIAN_POINT('Ctrl Pts',(-5.91528801894685,-0.151842421823986,
40.5687712714362));
#20888=CARTESIAN_POINT('Ctrl Pts',(-5.91236824443533,-0.227667091808765,
40.5723445032567));
#20889=CARTESIAN_POINT('Ctrl Pts',(-5.90600438944925,-0.39293232110902,
40.5801326146495));
#20890=CARTESIAN_POINT('Ctrl Pts',(-5.89270570371615,-0.557960059762128,
40.5879207260422));
#20891=CARTESIAN_POINT('Ctrl Pts',(-5.87251354639665,-0.722160099900164,
40.595708837435));
#20892=CARTESIAN_POINT('Ctrl Pts',(-5.85232535345526,-0.886327902222636,
40.6034954197679));
#20893=CARTESIAN_POINT('Ctrl Pts',(-5.82524642836426,-1.0496680133305,40.6112820021008));
#20894=CARTESIAN_POINT('Ctrl Pts',(-5.79136990959353,-1.21159610958217,
40.6190685844337));
#20895=CARTESIAN_POINT('Ctrl Pts',(-5.75749209911871,-1.37353038011595,
40.6268554636673));
#20896=CARTESIAN_POINT('Ctrl Pts',(-5.7168162378872,-1.53405221450648,40.6346423429009));
#20897=CARTESIAN_POINT('Ctrl Pts',(-5.6694865839613,-1.69258749752646,40.6424292221345));
#20898=CARTESIAN_POINT('Ctrl Pts',(-5.62216005376524,-1.85111231730925,
40.6502155874385));
#20899=CARTESIAN_POINT('Ctrl Pts',(-5.56818070120106,-2.00765054192988,
40.6580019527426));
#20900=CARTESIAN_POINT('Ctrl Pts',(-5.50774270464845,-2.16164309308725,
40.6657883180467));
#20901=CARTESIAN_POINT('Ctrl Pts',(-5.44728883830516,-2.31567607956168,
40.6735767278921));
#20902=CARTESIAN_POINT('Ctrl Pts',(-5.38037305420142,-2.46716175854072,
40.6813651377377));
#20903=CARTESIAN_POINT('Ctrl Pts',(-5.30723808422377,-2.61556007001651,
40.6891535475831));
#20904=CARTESIAN_POINT('Ctrl Pts',(-5.23794650016763,-2.75615975955705,
40.6965326612361));
#20905=CARTESIAN_POINT('Ctrl Pts',(-5.16307269353119,-2.89398799656402,
40.7039117748891));
#20906=CARTESIAN_POINT('Ctrl Pts',(-5.08286154899847,-3.02860513045409,
40.7112908885421));
#20907=CARTESIAN_POINT('Ctrl Pts',(-4.99820458910354,-3.17068360809325,
40.719078999935));
#20908=CARTESIAN_POINT('Ctrl Pts',(-4.90757161993195,-3.30923567219652,
40.726867111328));
#20909=CARTESIAN_POINT('Ctrl Pts',(-4.81128133616373,-3.44376283544361,
40.7346552227209));
#20910=CARTESIAN_POINT('Ctrl Pts',(-4.7150099573142,-3.57826358662725,40.742441805054));
#20911=CARTESIAN_POINT('Ctrl Pts',(-4.61308366593718,-3.70874075400858,
40.750228387387));
#20912=CARTESIAN_POINT('Ctrl Pts',(-4.50586381008473,-3.83472579038824,
40.7580149697201));
#20913=CARTESIAN_POINT('Ctrl Pts',(-4.39863986596291,-3.96071563054944,
40.7658018489537));
#20914=CARTESIAN_POINT('Ctrl Pts',(-4.28612215755448,-4.08221275108543,
40.7735887281874));
#20915=CARTESIAN_POINT('Ctrl Pts',(-4.16871203812706,-4.19878202645416,
40.7813756074211));
#20916=CARTESIAN_POINT('Ctrl Pts',(-4.05130966769977,-4.31534360831799,
40.7891619727252));
#20917=CARTESIAN_POINT('Ctrl Pts',(-3.92901575927058,-4.42697777079846,
40.7969483380294));
#20918=CARTESIAN_POINT('Ctrl Pts',(-3.80226830808157,-4.53328647626184,
40.8047347033335));
#20919=CARTESIAN_POINT('Ctrl Pts',(-3.67548757558562,-4.63962309623258,
40.8125231131791));
#20920=CARTESIAN_POINT('Ctrl Pts',(-3.54425120733451,-4.74063125801737,
40.8203115230246));
#20921=CARTESIAN_POINT('Ctrl Pts',(-3.40903073549084,-4.83595285408975,
40.8280999328702));
#20922=CARTESIAN_POINT('Ctrl Pts',(-3.28091636431262,-4.92626511357244,
40.8354790465224));
#20923=CARTESIAN_POINT('Ctrl Pts',(-3.14922607668857,-5.01147296519138,
40.8428581601746));
#20924=CARTESIAN_POINT('Ctrl Pts',(-3.01438525579226,-5.09130750320212,
40.8502372738269));
#20925=CARTESIAN_POINT('Ctrl Pts',(-2.87207069296472,-5.1755669826388,40.8580253852199));
#20926=CARTESIAN_POINT('Ctrl Pts',(-2.72619562056994,-5.25387070427942,
40.865813496613));
#20927=CARTESIAN_POINT('Ctrl Pts',(-2.57727838559369,-5.3259334098026,40.8736016080061));
#20928=CARTESIAN_POINT('Ctrl Pts',(-2.42839038792047,-5.39798196706982,
40.8813881903392));
#20929=CARTESIAN_POINT('Ctrl Pts',(-2.27646170685251,-5.46379181398922,
40.8891747726724));
#20930=CARTESIAN_POINT('Ctrl Pts',(-2.12203381986554,-5.52312439022035,
40.8969613550056));
#20931=CARTESIAN_POINT('Ctrl Pts',(-1.96760004457754,-5.58245922878942,
40.9047482342394));
#20932=CARTESIAN_POINT('Ctrl Pts',(-1.81066716953002,-5.63531618418975,
40.9125351134732));
#20933=CARTESIAN_POINT('Ctrl Pts',(-1.65179581159229,-5.6815051843069,40.9203219927071));
#20934=CARTESIAN_POINT('Ctrl Pts',(-1.49293493907222,-5.72769113597678,
40.9281083580114));
#20935=CARTESIAN_POINT('Ctrl Pts',(-1.33213614656812,-5.76720992393617,
40.9358947233157));
#20936=CARTESIAN_POINT('Ctrl Pts',(-1.16997448294024,-5.79992157462226,
40.94368108862));
#20937=CARTESIAN_POINT('Ctrl Pts',(-1.00777023895262,-5.83264181472352,
40.9514694984657));
#20938=CARTESIAN_POINT('Ctrl Pts',(-0.844202721799262,-5.85855128079383,
40.9592579083114));
#20939=CARTESIAN_POINT('Ctrl Pts',(-0.679857325904446,-5.87756110805443,
40.9670463181571));
#20940=CARTESIAN_POINT('Ctrl Pts',(-0.524148602498533,-5.89557193165432,
40.9744254318088));
#20941=CARTESIAN_POINT('Ctrl Pts',(-0.36774191395847,-5.90738961366641,
40.9818045454605));
#20942=CARTESIAN_POINT('Ctrl Pts',(-0.211139452949608,-5.91298154012915,
40.9891836591122));
#20943=CARTESIAN_POINT('Ctrl Pts',(-0.0458570805245572,-5.91888340697234,
40.9969717705051));
#20944=CARTESIAN_POINT('Ctrl Pts',(0.11970241207362,-5.91785191361215,41.0047598818981));
#20945=CARTESIAN_POINT('Ctrl Pts',(0.284947374884473,-5.90988456368197,
41.012547993291));
#20946=CARTESIAN_POINT('Ctrl Pts',(0.450159894727242,-5.90191877800207,
41.020334575624));
#20947=CARTESIAN_POINT('Ctrl Pts',(0.615057689036556,-5.88701986819625,
41.028121157957));
#20948=CARTESIAN_POINT('Ctrl Pts',(0.779051138401559,-5.86523741090292,
41.03590774029));
#20949=CARTESIAN_POINT('Ctrl Pts',(0.943050840800521,-5.84345412304932,
41.0436946195237));
#20950=CARTESIAN_POINT('Ctrl Pts',(1.10614581200184,-5.81478680066557,41.0514814987574));
#20951=CARTESIAN_POINT('Ctrl Pts',(1.26775282433349,-5.77933675596902,41.0592683779911));
#20952=CARTESIAN_POINT('Ctrl Pts',(1.42934917069571,-5.74388905095493,41.0670547432952));
#20953=CARTESIAN_POINT('Ctrl Pts',(1.58945744260377,-5.70165958804027,41.0748411085993));
#20954=CARTESIAN_POINT('Ctrl Pts',(1.74750570823874,-5.65280057689753,41.0826274739035));
#20955=CARTESIAN_POINT('Ctrl Pts',(1.90559547413876,-5.60392873637065,41.090415883749));
#20956=CARTESIAN_POINT('Ctrl Pts',(2.06162384685479,-5.54842396174471,41.0982042935946));
#20957=CARTESIAN_POINT('Ctrl Pts',(2.21503426213652,-5.48648829216479,41.1059927034401));
#20958=CARTESIAN_POINT('Ctrl Pts',(2.36038265959799,-5.42780746333963,41.1133718170925));
#20959=CARTESIAN_POINT('Ctrl Pts',(2.50338093884655,-5.3633543643843,41.1207509307449));
#20960=CARTESIAN_POINT('Ctrl Pts',(2.64357250937003,-5.29334062291508,41.1281300443973));
#20961=CARTESIAN_POINT('Ctrl Pts',(2.79153439463449,-5.21944627146783,41.1359181557902));
#20962=CARTESIAN_POINT('Ctrl Pts',(2.9364224614312,-5.13933099409852,41.1437062671832));
#20963=CARTESIAN_POINT('Ctrl Pts',(3.07771597407476,-5.0532756648955,41.1514943785761));
#20964=CARTESIAN_POINT('Ctrl Pts',(3.21898174620004,-4.96723723115631,41.1592809609092));
#20965=CARTESIAN_POINT('Ctrl Pts',(3.35665409958061,-4.87526123865677,41.1670675432422));
#20966=CARTESIAN_POINT('Ctrl Pts',(3.49023899516495,-4.77767331649307,41.1748541255752));
#20967=CARTESIAN_POINT('Ctrl Pts',(3.62382898431173,-4.68008167332355,41.1826410048089));
#20968=CARTESIAN_POINT('Ctrl Pts',(3.75333094346604,-4.57687785760383,41.1904278840426));
#20969=CARTESIAN_POINT('Ctrl Pts',(3.87828119843344,-4.46842987058964,41.1982147632763));
#20970=CARTESIAN_POINT('Ctrl Pts',(4.00322320675625,-4.35998904107989,41.2060011285804));
#20971=CARTESIAN_POINT('Ctrl Pts',(4.1236138708036,-4.24630494244777,41.2137874938846));
#20972=CARTESIAN_POINT('Ctrl Pts',(4.23902378666487,-4.12778486583172,41.2215738591887));
#20973=CARTESIAN_POINT('Ctrl Pts',(4.35446400682645,-4.00923366825032,41.2293622690343));
#20974=CARTESIAN_POINT('Ctrl Pts',(4.46492064100376,-3.88584418302148,41.2371506788799));
#20975=CARTESIAN_POINT('Ctrl Pts',(4.57000162007585,-3.75806010529423,41.2449390887255));
#20976=CARTESIAN_POINT('Ctrl Pts',(4.66956038786608,-3.63699133115378,41.2523182023778));
#20977=CARTESIAN_POINT('Ctrl Pts',(4.76429380562663,-3.51197817427837,41.2596973160301));
#20978=CARTESIAN_POINT('Ctrl Pts',(4.85390218092079,-3.38342491871068,41.2670764296824));
#20979=CARTESIAN_POINT('Ctrl Pts',(4.94847722630117,-3.24774641835624,41.2748645410754));
#20980=CARTESIAN_POINT('Ctrl Pts',(5.03737677118627,-3.10807580409691,41.2826526524684));
#20981=CARTESIAN_POINT('Ctrl Pts',(5.12027792575269,-2.96490885619604,41.2904407638614));
#20982=CARTESIAN_POINT('Ctrl Pts',(5.20316280412257,-2.82177001662966,41.2982273461944));
#20983=CARTESIAN_POINT('Ctrl Pts',(5.28005148197605,-2.67513648942692,41.3060139285275));
#20984=CARTESIAN_POINT('Ctrl Pts',(5.35066592478731,-2.52553058263406,41.3138005108606));
#20985=CARTESIAN_POINT('Ctrl Pts',(5.42128306011157,-2.37591897140127,41.3215873900943));
#20986=CARTESIAN_POINT('Ctrl Pts',(5.48562534172978,-2.22333504105345,41.3293742693281));
#20987=CARTESIAN_POINT('Ctrl Pts',(5.54346167152561,-2.06832377997896,41.3371611485618));
#20988=CARTESIAN_POINT('Ctrl Pts',(5.60129418415714,-1.91332274955802,41.344947513866));
#20989=CARTESIAN_POINT('Ctrl Pts',(5.65262149264367,-1.75589500843399,41.3527338791702));
#20990=CARTESIAN_POINT('Ctrl Pts',(5.69726139005274,-1.5966036502258,41.3605202444744));
#20991=CARTESIAN_POINT('Ctrl Pts',(5.74191300899237,-1.43727046534168,41.36830865432));
#20992=CARTESIAN_POINT('Ctrl Pts',(5.77987361989471,-1.27607299290788,41.3760970641656));
#20993=CARTESIAN_POINT('Ctrl Pts',(5.81101121732072,-1.11358843145604,41.3838854740112));
#20994=CARTESIAN_POINT('Ctrl Pts',(5.84051247300888,-0.959642751987385,
41.3912645876633));
#20995=CARTESIAN_POINT('Ctrl Pts',(5.86388934689645,-0.804542037616839,
41.3986437013154));
#20996=CARTESIAN_POINT('Ctrl Pts',(5.88107209595643,-0.648784682820597,
41.4060228149675));
#20997=CARTESIAN_POINT('Ctrl Pts',(5.89920722302258,-0.484394257816035,
41.4138109263604));
#20998=CARTESIAN_POINT('Ctrl Pts',(5.91044859548314,-0.319213626041863,
41.4215990377534));
#20999=CARTESIAN_POINT('Ctrl Pts',(5.91474987517481,-0.153832625342049,
41.4293871491464));
#21000=CARTESIAN_POINT('Ctrl Pts',(5.91905031038518,0.0115159056812921,
41.4371737314794));
#21001=CARTESIAN_POINT('Ctrl Pts',(5.91641336324894,0.177064407914185,41.4449603138124));
#21002=CARTESIAN_POINT('Ctrl Pts',(5.90684477589026,0.342221209217062,41.4527468961455));
#21003=CARTESIAN_POINT('Ctrl Pts',(5.89727582368347,0.507384307912026,41.4605337753792));
#21004=CARTESIAN_POINT('Ctrl Pts',(5.88077471692483,0.672155356581829,41.4683206546129));
#21005=CARTESIAN_POINT('Ctrl Pts',(5.85739926474652,0.835945222994252,41.4761075338466));
#21006=CARTESIAN_POINT('Ctrl Pts',(5.83402535533454,0.999724279370245,41.4838938991507));
#21007=CARTESIAN_POINT('Ctrl Pts',(5.80377805369661,1.16252196674723,41.4916802644549));
#21008=CARTESIAN_POINT('Ctrl Pts',(5.76676676361029,1.32375664554318,41.4994666297591));
#21009=CARTESIAN_POINT('Ctrl Pts',(5.72974575511078,1.48503366129158,41.5072550396047));
#21010=CARTESIAN_POINT('Ctrl Pts',(5.68595727881599,1.64474653629759,41.5150434494503));
#21011=CARTESIAN_POINT('Ctrl Pts',(5.63556156986838,1.80232526329813,41.5228318592959));
#21012=CARTESIAN_POINT('Ctrl Pts',(5.58781425414112,1.95162291952944,41.5302109729481));
#21013=CARTESIAN_POINT('Ctrl Pts',(5.53413636952841,2.09900471805148,41.5375900866004));
#21014=CARTESIAN_POINT('Ctrl Pts',(5.4747051225789,2.24399963977456,41.5449692002526));
#21015=CARTESIAN_POINT('Ctrl Pts',(5.41197981527528,2.39703110873013,41.5527573116456));
#21016=CARTESIAN_POINT('Ctrl Pts',(5.34282288190796,2.54745826098493,41.5605454230386));
#21017=CARTESIAN_POINT('Ctrl Pts',(5.26747583110242,2.69474097665283,41.5683335344316));
#21018=CARTESIAN_POINT('Ctrl Pts',(5.19214357337682,2.84199477592703,41.5761201167646));
#21019=CARTESIAN_POINT('Ctrl Pts',(5.11062376857809,2.98610508613235,41.5839066990977));
#21020=CARTESIAN_POINT('Ctrl Pts',(5.02320453581267,3.12655509369194,41.5916932814308));
#21021=CARTESIAN_POINT('Ctrl Pts',(4.93578196977136,3.26701045657907,41.5994801606645));
#21022=CARTESIAN_POINT('Ctrl Pts',(4.8424596911384,3.40380496419873,41.6072670398982));
#21023=CARTESIAN_POINT('Ctrl Pts',(4.74357032506724,3.53644894401736,41.615053919132));
#21024=CARTESIAN_POINT('Ctrl Pts',(4.64468748563703,3.66908416941007,41.6228402844362));
#21025=CARTESIAN_POINT('Ctrl Pts',(4.54023848513357,3.79756915906116,41.6306266497403));
#21026=CARTESIAN_POINT('Ctrl Pts',(4.43059767039804,3.92144550460203,41.6384130150445));
#21027=CARTESIAN_POINT('Ctrl Pts',(4.32092806621105,4.04535437755567,41.6462014248902));
#21028=CARTESIAN_POINT('Ctrl Pts',(4.20606413416399,4.16465194758013,41.6539898347358));
#21029=CARTESIAN_POINT('Ctrl Pts',(4.0864192919683,4.27891434042904,41.6617782445814));
#21030=CARTESIAN_POINT('Ctrl Pts',(3.9730620205924,4.38717202071458,41.6691573582335));
#21031=CARTESIAN_POINT('Ctrl Pts',(3.85541359519258,4.49090994932463,41.6765364718857));
#21032=CARTESIAN_POINT('Ctrl Pts',(3.73385497702661,4.58979929550668,41.6839155855378));
#21033=CARTESIAN_POINT('Ctrl Pts',(3.6055588016756,4.69416972262684,41.6917036969308));
#21034=CARTESIAN_POINT('Ctrl Pts',(3.47286086561413,4.79317612309264,41.6994918083237));
#21035=CARTESIAN_POINT('Ctrl Pts',(3.3362316554792,4.88645975154595,41.7072799197167));
#21036=CARTESIAN_POINT('Ctrl Pts',(3.19962927010773,4.97972506538509,41.7150665020498));
#21037=CARTESIAN_POINT('Ctrl Pts',(3.05909741443301,5.06726966900224,41.7228530843828));
#21038=CARTESIAN_POINT('Ctrl Pts',(2.9151363542591,5.14877758293918,41.7306396667159));
#21039=CARTESIAN_POINT('Ctrl Pts',(2.77116980488214,5.23028860475466,41.7384265459496));
#21040=CARTESIAN_POINT('Ctrl Pts',(2.62377406546405,5.30576231544556,41.7462134251833));
#21041=CARTESIAN_POINT('Ctrl Pts',(2.47347549835246,5.37492786198569,41.754000304417));
#21042=CARTESIAN_POINT('Ctrl Pts',(2.3231868508594,5.44408884363974,41.7617866697211));
#21043=CARTESIAN_POINT('Ctrl Pts',(2.16999604940352,5.50694236081271,41.7695730350253));
#21044=CARTESIAN_POINT('Ctrl Pts',(2.01445113521985,5.56326497538195,41.7773594003295));
#21045=CARTESIAN_POINT('Ctrl Pts',(1.85886537810032,5.61960237912604,41.7851478101751));
#21046=CARTESIAN_POINT('Ctrl Pts',(1.7009245730516,5.6694053428885,41.7929362200207));
#21047=CARTESIAN_POINT('Ctrl Pts',(1.54119454798986,5.71249944662985,41.8007246298663));
#21048=CARTESIAN_POINT('Ctrl Pts',(1.38985864862549,5.75332887080653,41.8081037435185));
#21049=CARTESIAN_POINT('Ctrl Pts',(1.23691699754553,5.78813635845961,41.8154828571707));
#21050=CARTESIAN_POINT('Ctrl Pts',(1.08286144975423,5.81681542109909,41.8228619708229));
#21051=CARTESIAN_POINT('Ctrl Pts',(0.92026715680235,5.84708406107501,41.8306500822158));
#21052=CARTESIAN_POINT('Ctrl Pts',(0.756373916800877,5.87053646925751,41.8384381936087));
#21053=CARTESIAN_POINT('Ctrl Pts',(0.591766511235335,5.88708272055696,41.8462263050016));
#21054=CARTESIAN_POINT('Ctrl Pts',(0.427191423464346,5.90362572328842,41.8540128873346));
#21055=CARTESIAN_POINT('Ctrl Pts',(0.261902767627809,5.91326524262942,41.8617994696676));
#21056=CARTESIAN_POINT('Ctrl Pts',(0.096491014262999,5.91596315460691,41.8695860520006));
#21057=CARTESIAN_POINT('Ctrl Pts',(-0.068927046215219,5.91866116945518,
41.8773729312342));
#21058=CARTESIAN_POINT('Ctrl Pts',(-0.234467894204855,5.91441703815268,
41.8851598104678));
#21059=CARTESIAN_POINT('Ctrl Pts',(-0.39953973327443,5.90324474878308,41.8929466897015));
#21060=CARTESIAN_POINT('Ctrl Pts',(-0.564600677698008,5.89207319677812,
41.9007330550056));
#21061=CARTESIAN_POINT('Ctrl Pts',(-0.729192356329885,5.87397442343852,
41.9085194203097));
#21062=CARTESIAN_POINT('Ctrl Pts',(-0.892726620974606,5.84901442490128,
41.9163057856139));
#21063=CARTESIAN_POINT('Ctrl Pts',(-1.05630382639649,5.82404787237526,41.9240941954594));
#21064=CARTESIAN_POINT('Ctrl Pts',(-1.21882274664656,5.79221654096599,41.9318826053049));
#21065=CARTESIAN_POINT('Ctrl Pts',(-1.37970306661821,5.75363798048368,41.9396710151504));
#21066=CARTESIAN_POINT('Ctrl Pts',(-1.5321288106491,5.71708679892093,41.9470501288029));
#21067=CARTESIAN_POINT('Ctrl Pts',(-1.68308349512621,5.67447936919105,41.9544292424555));
#21068=CARTESIAN_POINT('Ctrl Pts',(-1.83208426309407,5.62595750209891,41.961808356108));
#21069=CARTESIAN_POINT('Ctrl Pts',(-1.98934360794733,5.57474624235821,41.9695964675011));
#21070=CARTESIAN_POINT('Ctrl Pts',(-2.14448246219937,5.51692803181443,41.9773845788942));
#21071=CARTESIAN_POINT('Ctrl Pts',(-2.29694429254527,5.45270368527795,41.9851726902873));
#21072=CARTESIAN_POINT('Ctrl Pts',(-2.44937618966847,5.38849194807236,41.9929592726205));
#21073=CARTESIAN_POINT('Ctrl Pts',(-2.59913181730158,5.31787670839332,42.0007458549537));
#21074=CARTESIAN_POINT('Ctrl Pts',(-2.7456744299343,5.24110699063709,42.0085324372868));
#21075=CARTESIAN_POINT('Ctrl Pts',(-2.89222263020433,5.16433434566855,42.0163193165207));
#21076=CARTESIAN_POINT('Ctrl Pts',(-3.03555728546627,5.08140689782442,42.0241061957545));
#21077=CARTESIAN_POINT('Ctrl Pts',(-3.17516541815747,4.99262006664206,42.0318930749884));
#21078=CARTESIAN_POINT('Ctrl Pts',(-3.31476433679263,4.90383909533922,42.0396794402927));
#21079=CARTESIAN_POINT('Ctrl Pts',(-3.45063695545803,4.80919968616075,42.047465805597));
#21080=CARTESIAN_POINT('Ctrl Pts',(-3.58229838267708,4.70904118265802,42.0552521709013));
#21081=CARTESIAN_POINT('Ctrl Pts',(-3.71399438151316,4.60885637956626,42.063040580747));
#21082=CARTESIAN_POINT('Ctrl Pts',(-3.84147672368727,4.50314977838328,42.0708289905928));
#21083=CARTESIAN_POINT('Ctrl Pts',(-3.96429206123212,4.39230224549176,42.0786174004385));
#21084=CARTESIAN_POINT('Ctrl Pts',(-4.08065321220568,4.28727996759325,42.0859965140901));
#21085=CARTESIAN_POINT('Ctrl Pts',(-4.19282506951788,4.17764336670298,42.0933756277416));
#21086=CARTESIAN_POINT('Ctrl Pts',(-4.30045147274419,4.06374798592042,42.1007547413932));
#21087=CARTESIAN_POINT('Ctrl Pts',(-4.41404322057784,3.94353979364195,42.1085428527862));
#21088=CARTESIAN_POINT('Ctrl Pts',(-4.52261191896151,3.8185444045299,42.1163309641791));
#21089=CARTESIAN_POINT('Ctrl Pts',(-4.6257649401832,3.68920442381171,42.124119075572));
#21090=CARTESIAN_POINT('Ctrl Pts',(-4.7288977091075,3.55988983674388,42.1319056579051));
#21091=CARTESIAN_POINT('Ctrl Pts',(-4.82661672330823,3.42623260968398,42.1396922402381));
#21092=CARTESIAN_POINT('Ctrl Pts',(-4.91856979635348,3.28870821461851,42.1474788225711));
#21093=CARTESIAN_POINT('Ctrl Pts',(-5.01052637554886,3.15117857577859,42.1552657018048));
#21094=CARTESIAN_POINT('Ctrl Pts',(-5.09671639278192,3.00978173729458,42.1630525810385));
#21095=CARTESIAN_POINT('Ctrl Pts',(-5.17683072986968,2.86502254036107,42.1708394602721));
#21096=CARTESIAN_POINT('Ctrl Pts',(-5.25693977945754,2.72027289745082,42.1786258255763));
#21097=CARTESIAN_POINT('Ctrl Pts',(-5.33097379671375,2.57216161982321,42.1864121908804));
#21098=CARTESIAN_POINT('Ctrl Pts',(-5.39866934128585,2.42121868197818,42.1941985561846));
#21099=CARTESIAN_POINT('Ctrl Pts',(-5.46638266133319,2.27023610958305,42.2019869660302));
#21100=CARTESIAN_POINT('Ctrl Pts',(-5.52775405035683,2.11642068217709,42.2097753758757));
#21101=CARTESIAN_POINT('Ctrl Pts',(-5.58256763306664,1.96032374487907,42.2175637857213));
#21102=CARTESIAN_POINT('Ctrl Pts',(-5.63450065463665,1.81243000739747,42.2249428993736));
#21103=CARTESIAN_POINT('Ctrl Pts',(-5.68054730697709,1.66248863338524,42.2323220130259));
#21104=CARTESIAN_POINT('Ctrl Pts',(-5.72056494184579,1.51098223306064,42.2397011266782));
#21105=CARTESIAN_POINT('Ctrl Pts',(-5.76325408235672,1.34936153676051,42.2475728567438));
#21106=CARTESIAN_POINT('Ctrl Pts',(-5.79909574989067,1.18590779273446,42.2554445868094));
#21107=CARTESIAN_POINT('Ctrl Pts',(-5.82795511545164,1.02120993668349,42.263316316875));
#21108=CARTESIAN_POINT('Ctrl Pts',(-5.85747324313865,0.85275258323201,42.2713677320283));
#21109=CARTESIAN_POINT('Ctrl Pts',(-5.87968639419594,0.68299395580701,42.2794191471817));
#21110=CARTESIAN_POINT('Ctrl Pts',(-5.89450570957145,0.512574874852035,
42.287470562335));
#21111=CARTESIAN_POINT('Ctrl Pts',(-5.90932502494696,0.342155793897115,
42.2955219774884));
#21112=CARTESIAN_POINT('Ctrl Pts',(-5.91675046754537,0.171076599197924,
42.3035733926417));
#21113=CARTESIAN_POINT('Ctrl Pts',(-5.91674999997791,-1.61694723147206E-5,
42.3116248077951));
#21114=CARTESIAN_POINT('Origin',(0.,0.,0.));
#21115=CARTESIAN_POINT('',(-5.917134484543,-9.42401903047951E-5,44.3133751922049));
#21116=CARTESIAN_POINT('',(-5.91674999906443,0.000105219438300132,44.0616248077951));
#21117=CARTESIAN_POINT('',(-5.91675,-7.2459289488551E-16,0.));
#21118=CARTESIAN_POINT('Ctrl Pts',(-5.917134484543,-9.42401903047951E-5,
44.3133751922049));
#21119=CARTESIAN_POINT('Ctrl Pts',(-5.91646026956298,0.887845364419518,
44.2715682318849));
#21120=CARTESIAN_POINT('Ctrl Pts',(-5.48922520664388,2.76062880404801,44.1834212730605));
#21121=CARTESIAN_POINT('Ctrl Pts',(-3.59065886915233,5.01524350157563,44.0489343157323));
#21122=CARTESIAN_POINT('Ctrl Pts',(-0.75195218801304,6.12209656912254,43.9099143202198));
#21123=CARTESIAN_POINT('Ctrl Pts',(2.2702363156626,5.73511338735183,43.7708943247072));
#21124=CARTESIAN_POINT('Ctrl Pts',(4.73847058738315,3.94872067728464,43.6318743291948));
#21125=CARTESIAN_POINT('Ctrl Pts',(6.0504834487093,1.19881129942669,43.492854333682));
#21126=CARTESIAN_POINT('Ctrl Pts',(5.8861341848116,-1.84361678585946,43.3538343381697));
#21127=CARTESIAN_POINT('Ctrl Pts',(4.28552521570779,-4.43618891846033,43.214814342657));
#21128=CARTESIAN_POINT('Ctrl Pts',(1.63921681303447,-5.94629857428774,43.0757943471447));
#21129=CARTESIAN_POINT('Ctrl Pts',(-1.40707245700614,-6.00546797472697,
42.936774351632));
#21130=CARTESIAN_POINT('Ctrl Pts',(-4.11002577701861,-4.59925935417381,
42.7977543561197));
#21131=CARTESIAN_POINT('Ctrl Pts',(-5.6321265650094,-2.33549534064642,42.6732879696438));
#21132=CARTESIAN_POINT('Ctrl Pts',(-5.9159223932062,-0.675180153545571,
42.5951615816723));
#21133=CARTESIAN_POINT('Ctrl Pts',(-5.91650634169521,0.000138707710825164,
42.5633751922049));
#21134=CARTESIAN_POINT('Ctrl Pts',(-5.91624600190987,-1.62085350774297E-5,
42.3116248096983));
#21135=CARTESIAN_POINT('Ctrl Pts',(-5.9162911582345,-0.474720455898875,
42.3339657104534));
#21136=CARTESIAN_POINT('Ctrl Pts',(-5.74279880125224,-1.9335131105899,42.4026220729701));
#21137=CARTESIAN_POINT('Ctrl Pts',(-4.55678795407543,-4.15666021881412,
42.5175938972485));
#21138=CARTESIAN_POINT('Ctrl Pts',(-2.01272668996952,-5.8301862667123,42.6565402825336));
#21139=CARTESIAN_POINT('Ctrl Pts',(1.02194545414071,-6.08257906827687,42.7954866678188));
#21140=CARTESIAN_POINT('Ctrl Pts',(3.80751395140674,-4.85231678097389,42.9344330531039));
#21141=CARTESIAN_POINT('Ctrl Pts',(5.66498437175318,-2.43928118528315,43.0733794383891));
#21142=CARTESIAN_POINT('Ctrl Pts',(6.14159022579141,0.568339802872113,43.212325823674));
#21143=CARTESIAN_POINT('Ctrl Pts',(5.12115676480036,3.43742549350886,43.3512722089594));
#21144=CARTESIAN_POINT('Ctrl Pts',(2.85241908071542,5.46862377761041,43.4902185942444));
#21145=CARTESIAN_POINT('Ctrl Pts',(-0.111608153759956,6.16682124380889,
43.6291649795295));
#21146=CARTESIAN_POINT('Ctrl Pts',(-3.04843041559615,5.36182922465329,43.7681113648146));
#21147=CARTESIAN_POINT('Ctrl Pts',(-5.24218451210158,3.24986802411406,43.9070577500999));
#21148=CARTESIAN_POINT('Ctrl Pts',(-5.88714142667184,1.20495123427865,44.0048955644266));
#21149=CARTESIAN_POINT('Ctrl Pts',(-5.91719016898237,0.110696514981872,
44.0564179169917));
#21150=CARTESIAN_POINT('Ctrl Pts',(-5.91709874397735,0.00010522564014079,
44.0616248077951));
#21151=CARTESIAN_POINT('Origin',(0.,0.,0.));
#21152=CARTESIAN_POINT('',(-5.91670022645612,8.9340538150264E-6,46.0633751921059));
#21153=CARTESIAN_POINT('',(-5.9167499982011,-0.000145901520602546,45.811624807825));
#21154=CARTESIAN_POINT('',(-5.91675,-7.2459289488551E-16,0.));
#21155=CARTESIAN_POINT('Ctrl Pts',(-5.91624311178355,8.95268515702394E-6,
46.0633751911966));
#21156=CARTESIAN_POINT('Ctrl Pts',(-5.91626844413286,0.482775674933225,
46.0406548784336));
#21157=CARTESIAN_POINT('Ctrl Pts',(-5.73873369182433,1.9501676262938,45.9715945671664));
#21158=CARTESIAN_POINT('Ctrl Pts',(-4.53885955463525,4.17663170963269,45.8561942573948));
#21159=CARTESIAN_POINT('Ctrl Pts',(-1.9858849930876,5.83967116274058,45.7171742618825));
#21160=CARTESIAN_POINT('Ctrl Pts',(1.05166000220467,6.07778822718667,45.5781542663699));
#21161=CARTESIAN_POINT('Ctrl Pts',(3.83259228064817,4.83288060115294,45.4391342708575));
#21162=CARTESIAN_POINT('Ctrl Pts',(5.67834406774424,2.40871483224303,45.3001142753448));
#21163=CARTESIAN_POINT('Ctrl Pts',(6.13853845488877,-0.603194937442445,
45.1610942798325));
#21164=CARTESIAN_POINT('Ctrl Pts',(5.10088465258069,-3.46792073955065,45.0220742843197));
#21165=CARTESIAN_POINT('Ctrl Pts',(2.81857776262614,-5.48644856813047,44.8830542888075));
#21166=CARTESIAN_POINT('Ctrl Pts',(-0.151482674794658,-6.1662428993653,
44.7440342932947));
#21167=CARTESIAN_POINT('Ctrl Pts',(-3.08458023385813,-5.3414289544657,44.6050142977824));
#21168=CARTESIAN_POINT('Ctrl Pts',(-5.26501770087436,-3.21326735647927,
44.4659943022696));
#21169=CARTESIAN_POINT('Ctrl Pts',(-5.89138148615921,-1.17682672319444,
44.3687812670773));
#21170=CARTESIAN_POINT('Ctrl Pts',(-5.91720758821343,-0.0963716088886832,
44.317908230389));
#21171=CARTESIAN_POINT('Ctrl Pts',(-5.917134484543,-9.42401903047951E-5,
44.3133751922049));
#21172=CARTESIAN_POINT('Ctrl Pts',(-5.91674999906443,0.000105219438300132,
44.0616248077951));
#21173=CARTESIAN_POINT('Ctrl Pts',(-5.91675292974581,-0.164694264183333,
44.0693844018043));
#21174=CARTESIAN_POINT('Ctrl Pts',(-5.90986626711654,-0.329524092285221,
44.0771439958136));
#21175=CARTESIAN_POINT('Ctrl Pts',(-5.89610847089198,-0.493796984575521,
44.0849035898228));
#21176=CARTESIAN_POINT('Ctrl Pts',(-5.88235316316463,-0.658040163339901,
44.092661780284));
#21177=CARTESIAN_POINT('Ctrl Pts',(-5.86172922869553,-0.821726284461634,
44.1004199707452));
#21178=CARTESIAN_POINT('Ctrl Pts',(-5.83430709207036,-0.98427197355076,
44.1081781612064));
#21179=CARTESIAN_POINT('Ctrl Pts',(-5.80688388374666,-1.14682401517105,
44.1159366548694));
#21180=CARTESIAN_POINT('Ctrl Pts',(-5.7726619930524,-1.30823521555114,44.1236951485324));
#21181=CARTESIAN_POINT('Ctrl Pts',(-5.73176329488124,-1.46793054806834,
44.1314536421954));
#21182=CARTESIAN_POINT('Ctrl Pts',(-5.6908653830365,-1.62762281025159,44.139211986692));
#21183=CARTESIAN_POINT('Ctrl Pts',(-5.64329100328209,-1.78559895718424,
44.1469703311887));
#21184=CARTESIAN_POINT('Ctrl Pts',(-5.58921245617926,-1.94129716483352,
44.1547286756854));
#21185=CARTESIAN_POINT('Ctrl Pts',(-5.53512176998858,-2.09703032227937,
44.1624887617086));
#21186=CARTESIAN_POINT('Ctrl Pts',(-5.47452410735967,-2.25048421314287,
44.1702488477318));
#21187=CARTESIAN_POINT('Ctrl Pts',(-5.40764088713853,-2.40111444921886,
44.178008933755));
#21188=CARTESIAN_POINT('Ctrl Pts',(-5.38769799454131,-2.44602859375355,
44.18032279606));
#21189=CARTESIAN_POINT('Ctrl Pts',(-5.36719658841139,-2.49069182920989,
44.182636658365));
#21190=CARTESIAN_POINT('Ctrl Pts',(-5.34614335675952,-2.53509009139243,
44.18495052067));
#21191=CARTESIAN_POINT('Ctrl Pts',(-5.27528135562149,-2.684527942898,44.192738632063));
#21192=CARTESIAN_POINT('Ctrl Pts',(-5.1981370458312,-2.83101946154697,44.2005267434561));
#21193=CARTESIAN_POINT('Ctrl Pts',(-5.11498062512479,-2.97403829280964,
44.2083148548492));
#21194=CARTESIAN_POINT('Ctrl Pts',(-5.03184053073186,-3.11702904481811,
44.2161014371824));
#21195=CARTESIAN_POINT('Ctrl Pts',(-4.94269084112915,-3.25654819377814,
44.2238880195156));
#21196=CARTESIAN_POINT('Ctrl Pts',(-4.84784704410832,-3.39209516367543,
44.2316746018488));
#21197=CARTESIAN_POINT('Ctrl Pts',(-4.75299963071467,-3.52764730194843,
44.2394614810826));
#21198=CARTESIAN_POINT('Ctrl Pts',(-4.65245785540012,-3.65922669403395,
44.2472483603165));
#21199=CARTESIAN_POINT('Ctrl Pts',(-4.54658018845511,-3.78636225848076,
44.2550352395503));
#21200=CARTESIAN_POINT('Ctrl Pts',(-4.44070950937486,-3.91348943205387,
44.2628216048546));
#21201=CARTESIAN_POINT('Ctrl Pts',(-4.32950384798739,-4.03617311942931,
44.270607970159));
#21202=CARTESIAN_POINT('Ctrl Pts',(-4.21336165507873,-4.1539757011822,44.2783943354633));
#21203=CARTESIAN_POINT('Ctrl Pts',(-4.09718896558881,-4.27180921550076,
44.286182745309));
#21204=CARTESIAN_POINT('Ctrl Pts',(-3.97607737753084,-4.38475883408334,
44.2939711551547));
#21205=CARTESIAN_POINT('Ctrl Pts',(-3.85046249940051,-4.49242352224391,
44.3017595650005));
#21206=CARTESIAN_POINT('Ctrl Pts',(-3.73144892918354,-4.59443022013675,
44.309138678652));
#21207=CARTESIAN_POINT('Ctrl Pts',(-3.60839340594453,-4.69169299836114,
44.3165177923036));
#21208=CARTESIAN_POINT('Ctrl Pts',(-3.48169401885481,-4.78390398331432,
44.3238969059552));
#21209=CARTESIAN_POINT('Ctrl Pts',(-3.34797214023092,-4.8812258916592,44.3316850173481));
#21210=CARTESIAN_POINT('Ctrl Pts',(-3.21014325251378,-4.97295487987166,
44.339473128741));
#21211=CARTESIAN_POINT('Ctrl Pts',(-3.0686964490714,-5.05875801614948,44.3472612401339));
#21212=CARTESIAN_POINT('Ctrl Pts',(-2.92727741624261,-5.14454430647754,
44.355047822467));
#21213=CARTESIAN_POINT('Ctrl Pts',(-2.78224215800226,-5.22440690065538,
44.3628344048));
#21214=CARTESIAN_POINT('Ctrl Pts',(-2.63410720459904,-5.29805717194326,
44.370620987133));
#21215=CARTESIAN_POINT('Ctrl Pts',(-2.48596660284336,-5.37171025149943,
44.3784078663667));
#21216=CARTESIAN_POINT('Ctrl Pts',(-2.33472635377261,-5.43915038839738,
44.3861947456004));
#21217=CARTESIAN_POINT('Ctrl Pts',(-2.1809266203098,-5.50013542008959,44.393981624834));
#21218=CARTESIAN_POINT('Ctrl Pts',(-2.02713703754053,-5.56111642680494,
44.4017679901382));
#21219=CARTESIAN_POINT('Ctrl Pts',(-1.87078860551923,-5.61564306319405,
44.4095543554424));
#21220=CARTESIAN_POINT('Ctrl Pts',(-1.71244058554131,-5.66352167855752,
44.4173407207465));
#21221=CARTESIAN_POINT('Ctrl Pts',(-1.55405098658872,-5.71141286587316,
44.4251291305921));
#21222=CARTESIAN_POINT('Ctrl Pts',(-1.3936610560103,-5.75265244962214,44.4329175404376));
#21223=CARTESIAN_POINT('Ctrl Pts',(-1.23184518070523,-5.78709668255796,
44.4407059502832));
#21224=CARTESIAN_POINT('Ctrl Pts',(-1.07853304660958,-5.81973080358423,
44.4480850639356));
#21225=CARTESIAN_POINT('Ctrl Pts',(-0.92394123975902,-5.84626536760117,
44.4554641775879));
#21226=CARTESIAN_POINT('Ctrl Pts',(-0.768566628930374,-5.86662048366814,
44.4628432912403));
#21227=CARTESIAN_POINT('Ctrl Pts',(-0.604580162022182,-5.88810381063853,
44.4706314026333));
#21228=CARTESIAN_POINT('Ctrl Pts',(-0.439663086899155,-5.90271092879514,
44.4784195140262));
#21229=CARTESIAN_POINT('Ctrl Pts',(-0.274404173926619,-5.91038348263729,
44.4862076254191));
#21230=CARTESIAN_POINT('Ctrl Pts',(-0.10917770666087,-5.91805453010723,
44.4939942077521));
#21231=CARTESIAN_POINT('Ctrl Pts',(0.0563901455546477,-5.91879371501194,
44.5017807900851));
#21232=CARTESIAN_POINT('Ctrl Pts',(0.22170771650763,-5.91259471390869,44.5095673724182));
#21233=CARTESIAN_POINT('Ctrl Pts',(0.38703159098281,-5.90639547643891,44.5173542516518));
#21234=CARTESIAN_POINT('Ctrl Pts',(0.552104845660218,-5.89325753162055,
44.5251411308855));
#21235=CARTESIAN_POINT('Ctrl Pts',(0.716337292044847,-5.87322666398342,
44.5329280101192));
#21236=CARTESIAN_POINT('Ctrl Pts',(0.88055889918308,-5.85319711837197,44.5407143754233));
#21237=CARTESIAN_POINT('Ctrl Pts',(1.04393949188983,-5.8262755991296,44.5485007407275));
#21238=CARTESIAN_POINT('Ctrl Pts',(1.20589532073218,-5.79255962748216,44.5562871060316));
#21239=CARTESIAN_POINT('Ctrl Pts',(1.3678936758865,-5.7588348027052,44.5640755158772));
#21240=CARTESIAN_POINT('Ctrl Pts',(1.52846620619538,-5.71831202381455,44.5718639257228));
#21241=CARTESIAN_POINT('Ctrl Pts',(1.68703975565961,-5.67113987001943,44.5796523355683));
#21242=CARTESIAN_POINT('Ctrl Pts',(1.83727995448778,-5.62644670530641,44.5870314492207));
#21243=CARTESIAN_POINT('Ctrl Pts',(1.9857256200061,-5.57578513978001,44.594410562873));
#21244=CARTESIAN_POINT('Ctrl Pts',(2.13190221775661,-5.5193227389259,44.6017896765254));
#21245=CARTESIAN_POINT('Ctrl Pts',(2.28618085879148,-5.45973083018408,44.6095777879184));
#21246=CARTESIAN_POINT('Ctrl Pts',(2.437986867365,-5.39365552973634,44.6173658993113));
#21247=CARTESIAN_POINT('Ctrl Pts',(2.58677531145044,-5.3213272827905,44.6251540107043));
#21248=CARTESIAN_POINT('Ctrl Pts',(2.7355345435187,-5.24901323623505,44.6329405930374));
#21249=CARTESIAN_POINT('Ctrl Pts',(2.88127710600939,-5.17044883233235,44.6407271753705));
#21250=CARTESIAN_POINT('Ctrl Pts',(3.02348041795781,-5.08591159230336,44.6485137577035));
#21251=CARTESIAN_POINT('Ctrl Pts',(3.16568915208702,-5.00137112888812,44.6563006369373));
#21252=CARTESIAN_POINT('Ctrl Pts',(3.30435808897071,-4.91085753351266,44.664087516171));
#21253=CARTESIAN_POINT('Ctrl Pts',(3.43899087555306,-4.81469337760597,44.6718743954047));
#21254=CARTESIAN_POINT('Ctrl Pts',(3.57361477644938,-4.71853556847794,44.6796607607089));
#21255=CARTESIAN_POINT('Ctrl Pts',(3.70420280015421,-4.61672813094623,44.6874471260131));
#21256=CARTESIAN_POINT('Ctrl Pts',(3.83028900055894,-4.50963598693921,44.6952334913173));
#21257=CARTESIAN_POINT('Ctrl Pts',(3.9564083086395,-4.40251572270987,44.703021901163));
#21258=CARTESIAN_POINT('Ctrl Pts',(4.07802318640741,-4.2901081846857,44.7108103110086));
#21259=CARTESIAN_POINT('Ctrl Pts',(4.19470141802977,-4.17281806170351,44.7185987208542));
#21260=CARTESIAN_POINT('Ctrl Pts',(4.30524798002809,-4.06169176443491,44.7259778345063));
#21261=CARTESIAN_POINT('Ctrl Pts',(4.41136322794721,-3.94618304619205,44.7333569481584));
#21262=CARTESIAN_POINT('Ctrl Pts',(4.51271063148502,-3.82666608407137,44.7407360618105));
#21263=CARTESIAN_POINT('Ctrl Pts',(4.61967535724367,-3.70052472641955,44.7485241732034));
#21264=CARTESIAN_POINT('Ctrl Pts',(4.72136692477582,-3.5698731490814,44.7563122845964));
#21265=CARTESIAN_POINT('Ctrl Pts',(4.81741706994369,-3.43517442595208,44.7641003959894));
#21266=CARTESIAN_POINT('Ctrl Pts',(4.9134483573405,-3.30050214856813,44.7718869783224));
#21267=CARTESIAN_POINT('Ctrl Pts',(5.00384024695538,-3.1617845708287,44.7796735606555));
#21268=CARTESIAN_POINT('Ctrl Pts',(5.08826662445309,-3.01951541161438,44.7874601429886));
#21269=CARTESIAN_POINT('Ctrl Pts',(5.17269622110941,-2.87724082770931,44.7952470222223));
#21270=CARTESIAN_POINT('Ctrl Pts',(5.25115968403862,-2.73141466411298,44.803033901456));
#21271=CARTESIAN_POINT('Ctrl Pts',(5.3233754838391,-2.58255765096557,44.8108207806897));
#21272=CARTESIAN_POINT('Ctrl Pts',(5.39558651743858,-2.43371046229491,44.8186071459939));
#21273=CARTESIAN_POINT('Ctrl Pts',(5.46155057369599,-2.28183311193025,44.8263935112981));
#21274=CARTESIAN_POINT('Ctrl Pts',(5.52103308621654,-2.12746897119613,44.8341798766023));
#21275=CARTESIAN_POINT('Ctrl Pts',(5.58053121763691,-1.97306429757344,44.8419682864479));
#21276=CARTESIAN_POINT('Ctrl Pts',(5.63354428774699,-1.81617182644615,44.8497566962934));
#21277=CARTESIAN_POINT('Ctrl Pts',(5.67988637536829,-1.65735371161551,44.857545106139));
#21278=CARTESIAN_POINT('Ctrl Pts',(5.7237930955098,-1.50688179981352,44.8649242197912));
#21279=CARTESIAN_POINT('Ctrl Pts',(5.76171187287224,-1.3546816810388,44.8723033334434));
#21280=CARTESIAN_POINT('Ctrl Pts',(5.7935262120333,-1.20124293670474,44.8796824470956));
#21281=CARTESIAN_POINT('Ctrl Pts',(5.8271039056369,-1.03929963440678,44.8874705584886));
#21282=CARTESIAN_POINT('Ctrl Pts',(5.85389327048895,-0.875918670096511,
44.8952586698815));
#21283=CARTESIAN_POINT('Ctrl Pts',(5.87379247632503,-0.71168287008151,44.9030467812745));
#21284=CARTESIAN_POINT('Ctrl Pts',(5.89368777529901,-0.547479314902179,
44.9108333636076));
#21285=CARTESIAN_POINT('Ctrl Pts',(5.90669557601055,-0.382421575905723,
44.9186199459407));
#21286=CARTESIAN_POINT('Ctrl Pts',(5.91276572254066,-0.217099223509076,
44.9264065282737));
#21287=CARTESIAN_POINT('Ctrl Pts',(5.91883610052409,-0.0517705674081396,
44.9341934075075));
#21288=CARTESIAN_POINT('Ctrl Pts',(5.91796827932953,0.113822403126622,44.9419802867412));
#21289=CARTESIAN_POINT('Ctrl Pts',(5.91016417722504,0.279087729479209,44.9497671659749));
#21290=CARTESIAN_POINT('Ctrl Pts',(5.90236059018677,0.444342148415976,44.9575535312791));
#21291=CARTESIAN_POINT('Ctrl Pts',(5.88762165353856,0.609268647252071,44.9653398965833));
#21292=CARTESIAN_POINT('Ctrl Pts',(5.86600135717776,0.773277854389171,44.9731262618875));
#21293=CARTESIAN_POINT('Ctrl Pts',(5.84437538376618,0.937330127013461,44.9809146717331));
#21294=CARTESIAN_POINT('Ctrl Pts',(5.81586447993154,1.10046430939594,44.9887030815787));
#21295=CARTESIAN_POINT('Ctrl Pts',(5.78057433824521,1.26209781020368,44.9964914914244));
#21296=CARTESIAN_POINT('Ctrl Pts',(5.74713876263145,1.41523715393347,45.0038706050765));
#21297=CARTESIAN_POINT('Ctrl Pts',(5.7076182026209,1.56702923267224,45.0112497187287));
#21298=CARTESIAN_POINT('Ctrl Pts',(5.6621445939367,1.71698839828737,45.0186288323808));
#21299=CARTESIAN_POINT('Ctrl Pts',(5.61415054660697,1.87525926132885,45.0264169437738));
#21300=CARTESIAN_POINT('Ctrl Pts',(5.5595076846427,2.03154479234359,45.0342050551667));
#21301=CARTESIAN_POINT('Ctrl Pts',(5.49840543322243,2.18528447905761,45.0419931665597));
#21302=CARTESIAN_POINT('Ctrl Pts',(5.43731517816377,2.33899398166495,45.0497797488928));
#21303=CARTESIAN_POINT('Ctrl Pts',(5.36976818200352,2.4901583405325,45.0575663312259));
#21304=CARTESIAN_POINT('Ctrl Pts',(5.29600247296227,2.63823584405897,45.065352913559));
#21305=CARTESIAN_POINT('Ctrl Pts',(5.22223395125119,2.7863189937472,45.0731397927927));
#21306=CARTESIAN_POINT('Ctrl Pts',(5.14224638112126,2.9313147648196,45.0809266720264));
#21307=CARTESIAN_POINT('Ctrl Pts',(5.056324660924,3.07270426267022,45.0887135512601));
#21308=CARTESIAN_POINT('Ctrl Pts',(4.97040861151069,3.21408442889559,45.0964999165643));
#21309=CARTESIAN_POINT('Ctrl Pts',(4.87855936183501,3.3518585251756,45.1042862818685));
#21310=CARTESIAN_POINT('Ctrl Pts',(4.78110629781429,3.48553484152727,45.1120726471727));
#21311=CARTESIAN_POINT('Ctrl Pts',(4.68362764459801,3.61924625856495,45.1198610570183));
#21312=CARTESIAN_POINT('Ctrl Pts',(4.58054242356535,3.74885748610181,45.1276494668639));
#21313=CARTESIAN_POINT('Ctrl Pts',(4.47222217801387,3.87390750444314,45.1354378767095));
#21314=CARTESIAN_POINT('Ctrl Pts',(4.36959437354556,3.99238589937065,45.1428169903616));
#21315=CARTESIAN_POINT('Ctrl Pts',(4.26226778446086,4.10676995904151,45.1501961040138));
#21316=CARTESIAN_POINT('Ctrl Pts',(4.15059061772226,4.21669634744737,45.1575752176659));
#21317=CARTESIAN_POINT('Ctrl Pts',(4.03272358712737,4.33271556036083,45.1653633290588));
#21318=CARTESIAN_POINT('Ctrl Pts',(3.90996793348465,4.44381038052038,45.1731514404517));
#21319=CARTESIAN_POINT('Ctrl Pts',(3.7827581642049,4.54957923698898,45.1809395518445));
#21320=CARTESIAN_POINT('Ctrl Pts',(3.65557337034532,4.65532732758679,45.1887261341775));
#21321=CARTESIAN_POINT('Ctrl Pts',(3.52393645125614,4.75575133673834,45.1965127165105));
#21322=CARTESIAN_POINT('Ctrl Pts',(3.388315598884,4.85048945621567,45.2042992988435));
#21323=CARTESIAN_POINT('Ctrl Pts',(3.25268957531885,4.94523118803647,45.2120861780772));
#21324=CARTESIAN_POINT('Ctrl Pts',(3.11307957418037,5.03428641015035,45.2198730573108));
#21325=CARTESIAN_POINT('Ctrl Pts',(2.9699840286919,5.11733577477724,45.2276599365445));
#21326=CARTESIAN_POINT('Ctrl Pts',(2.82689792742734,5.20037965819372,45.2354463018486));
#21327=CARTESIAN_POINT('Ctrl Pts',(2.68032701860359,5.27741831704511,45.2432326671527));
#21328=CARTESIAN_POINT('Ctrl Pts',(2.53079579490881,5.34817755940955,45.2510190324567));
#21329=CARTESIAN_POINT('Ctrl Pts',(2.38122530735057,5.41895538171443,45.2588074423023));
#21330=CARTESIAN_POINT('Ctrl Pts',(2.22869323985966,5.48345035427393,45.2665958521478));
#21331=CARTESIAN_POINT('Ctrl Pts',(2.07374642116591,5.54143540458621,45.2743842619933));
#21332=CARTESIAN_POINT('Ctrl Pts',(1.92694236129699,5.59637322692623,45.2817633756459));
#21333=CARTESIAN_POINT('Ctrl Pts',(1.77797106576764,5.64546765576021,45.2891424892985));
#21334=CARTESIAN_POINT('Ctrl Pts',(1.62731213581907,5.68856623193542,45.296521602951));
#21335=CARTESIAN_POINT('Ctrl Pts',(1.46830272302965,5.73405360724083,45.3043097143441));
#21336=CARTESIAN_POINT('Ctrl Pts',(1.30735650189762,5.77287787120483,45.3120978257372));
#21337=CARTESIAN_POINT('Ctrl Pts',(1.14504714899589,5.80489427888884,45.3198859371303));
#21338=CARTESIAN_POINT('Ctrl Pts',(0.982769662705261,5.8369044007095,45.3276725194635));
#21339=CARTESIAN_POINT('Ctrl Pts',(0.819129891934903,5.86210927137328,45.3354591017967));
#21340=CARTESIAN_POINT('Ctrl Pts',(0.654712068535333,5.88041517835384,45.3432456841299));
#21341=CARTESIAN_POINT('Ctrl Pts',(0.490287975921632,5.89872178333446,45.3510325633637));
#21342=CARTESIAN_POINT('Ctrl Pts',(0.325086088431835,5.91012885897701,45.3588194425975));
#21343=CARTESIAN_POINT('Ctrl Pts',(0.159696878896288,5.91459444673688,45.3666063218314));
#21344=CARTESIAN_POINT('Ctrl Pts',(-0.0056814150471084,5.91905973977055,
45.3743926871357));
#21345=CARTESIAN_POINT('Ctrl Pts',(-0.171246686855606,5.91658445321134,
45.38217905244));
#21346=CARTESIAN_POINT('Ctrl Pts',(-0.336407184442936,5.90717874867141,
45.3899654177442));
#21347=CARTESIAN_POINT('Ctrl Pts',(-0.501611049823396,5.89777057438445,
45.39775382759));
#21348=CARTESIAN_POINT('Ctrl Pts',(-0.666409609270265,5.8814283620441,45.4055422374357));
#21349=CARTESIAN_POINT('Ctrl Pts',(-0.830214040501387,5.8582143362508,45.4133306472814));
#21350=CARTESIAN_POINT('Ctrl Pts',(-0.985410227993851,5.83622025298702,
45.420709760933));
#21351=CARTESIAN_POINT('Ctrl Pts',(-1.13971382907723,5.8080580705383,45.4280888745846));
#21352=CARTESIAN_POINT('Ctrl Pts',(-1.29263075311924,5.77382336918877,45.4354679882362));
#21353=CARTESIAN_POINT('Ctrl Pts',(-1.45402331251518,5.73769116141929,45.4432560996291));
#21354=CARTESIAN_POINT('Ctrl Pts',(-1.61392876009556,5.69478128607549,45.451044211022));
#21355=CARTESIAN_POINT('Ctrl Pts',(-1.7717740862838,5.64524110642523,45.4588323224149));
#21356=CARTESIAN_POINT('Ctrl Pts',(-1.92958842229475,5.59571065312537,45.466618904748));
#21357=CARTESIAN_POINT('Ctrl Pts',(-2.08534313927165,5.5395525885105,45.474405487081));
#21358=CARTESIAN_POINT('Ctrl Pts',(-2.2384803745134,5.47696413859159,45.4821920694141));
#21359=CARTESIAN_POINT('Ctrl Pts',(-2.39162344884292,5.4143733021894,45.4899789486478));
#21360=CARTESIAN_POINT('Ctrl Pts',(-2.54214854446916,5.34535170708692,45.4977658278815));
#21361=CARTESIAN_POINT('Ctrl Pts',(-2.68951707927402,5.27014501155266,45.5055527071151));
#21362=CARTESIAN_POINT('Ctrl Pts',(-2.83687588784108,5.19494327961667,45.5133390724193));
#21363=CARTESIAN_POINT('Ctrl Pts',(-2.98107826791173,5.11355740950706,45.5211254377235));
#21364=CARTESIAN_POINT('Ctrl Pts',(-3.12160945014501,5.02627943943285,45.5289118030276));
#21365=CARTESIAN_POINT('Ctrl Pts',(-3.26217753301292,4.93897855193608,45.5367002128732));
#21366=CARTESIAN_POINT('Ctrl Pts',(-3.39907221916424,4.84578263999627,45.5444886227188));
#21367=CARTESIAN_POINT('Ctrl Pts',(-3.53180622075539,4.74702805779928,45.5522770325643));
#21368=CARTESIAN_POINT('Ctrl Pts',(-3.6575647905649,4.65346322233621,45.5596561462167));
#21369=CARTESIAN_POINT('Ctrl Pts',(-3.77958852371299,4.55490908299573,45.567035259869));
#21370=CARTESIAN_POINT('Ctrl Pts',(-3.89748927691541,4.45168596138917,45.5744143735213));
#21371=CARTESIAN_POINT('Ctrl Pts',(-4.02192484499469,4.34274155325654,45.5822024849142));
#21372=CARTESIAN_POINT('Ctrl Pts',(-4.14181187106979,4.22855700725017,45.5899905963072));
#21373=CARTESIAN_POINT('Ctrl Pts',(-4.25671768613563,4.10953587440725,45.5977787077001));
#21374=CARTESIAN_POINT('Ctrl Pts',(-4.3716009414481,3.99053810928859,45.6055652900331));
#21375=CARTESIAN_POINT('Ctrl Pts',(-4.48150471530554,3.86670588176482,45.6133518723661));
#21376=CARTESIAN_POINT('Ctrl Pts',(-4.58603349561461,3.73847928168672,45.6211384546991));
#21377=CARTESIAN_POINT('Ctrl Pts',(-4.69056626158296,3.61024779235671,45.6289253339328));
#21378=CARTESIAN_POINT('Ctrl Pts',(-4.78972341895787,3.4776218403516,45.6367122131665));
#21379=CARTESIAN_POINT('Ctrl Pts',(-4.88314955806598,3.34107482048217,45.6444990924002));
#21380=CARTESIAN_POINT('Ctrl Pts',(-4.97656953110303,3.20453681263698,45.6522854577043));
#21381=CARTESIAN_POINT('Ctrl Pts',(-5.0642590624491,3.06407851859942,45.6600718230085));
#21382=CARTESIAN_POINT('Ctrl Pts',(-5.14590584277307,2.92020266759243,45.6678581883127));
#21383=CARTESIAN_POINT('Ctrl Pts',(-5.22757406188339,2.77628903770896,45.6756465981582));
#21384=CARTESIAN_POINT('Ctrl Pts',(-5.30319619991197,2.62895633482615,45.6834350080038));
#21385=CARTESIAN_POINT('Ctrl Pts',(-5.37250528198391,2.47873305492039,45.6912234178494));
#21386=CARTESIAN_POINT('Ctrl Pts',(-5.43817203603136,2.33640430262884,45.6986025315017));
#21387=CARTESIAN_POINT('Ctrl Pts',(-5.49817208583667,2.1914812062773,45.7059816451541));
#21388=CARTESIAN_POINT('Ctrl Pts',(-5.55231784707662,2.04443074901901,45.7133607588064));
#21389=CARTESIAN_POINT('Ctrl Pts',(-5.60936455460306,1.88950182688849,45.7211352203467));
#21390=CARTESIAN_POINT('Ctrl Pts',(-5.65993365776862,1.73215368485384,45.728909681887));
#21391=CARTESIAN_POINT('Ctrl Pts',(-5.70383841306928,1.57294561892497,45.7366841434273));
#21392=CARTESIAN_POINT('Ctrl Pts',(-5.74773600855045,1.41376351603831,45.7444573371382));
#21393=CARTESIAN_POINT('Ctrl Pts',(-5.78497133736338,1.25272240398576,45.752230530849));
#21394=CARTESIAN_POINT('Ctrl Pts',(-5.81540773362642,1.09039600796133,45.7600037245599));
#21395=CARTESIAN_POINT('Ctrl Pts',(-5.84583994428435,0.928091935019634,
45.7677758493032));
#21396=CARTESIAN_POINT('Ctrl Pts',(-5.86947503018122,0.764503247196753,
45.7755479740466));
#21397=CARTESIAN_POINT('Ctrl Pts',(-5.88622751631293,0.600213452615404,
45.7833200987899));
#21398=CARTESIAN_POINT('Ctrl Pts',(-5.90298054378356,0.435918349182701,
45.7910924746812));
#21399=CARTESIAN_POINT('Ctrl Pts',(-5.91285049410255,0.270922413718954,
45.7988648505726));
#21400=CARTESIAN_POINT('Ctrl Pts',(-5.91580373762763,0.105814462012333,
45.8066372264639));
#21401=CARTESIAN_POINT('Ctrl Pts',(-5.91643544246187,0.0704975332260584,
45.8082997535743));
#21402=CARTESIAN_POINT('Ctrl Pts',(-5.91675086918974,0.0351754882530035,
45.8099622806847));
#21403=CARTESIAN_POINT('Ctrl Pts',(-5.91674999820112,-0.000145900885215194,
45.8116248077951));
#21404=CARTESIAN_POINT('Origin',(0.,0.,0.));
#21405=CARTESIAN_POINT('',(-5.91674999948831,7.78145713578612E-5,47.8133751922472));
#21406=CARTESIAN_POINT('',(-5.91674999827337,0.000142940948123385,47.5616248068849));
#21407=CARTESIAN_POINT('',(-5.91675,-7.2459289488551E-16,0.));
#21408=CARTESIAN_POINT('Ctrl Pts',(-5.9167499994883,7.78154695080284E-5,
47.8133751922049));
#21409=CARTESIAN_POINT('Ctrl Pts',(-5.91674898459005,0.0772462657434625,
47.8097415263266));
#21410=CARTESIAN_POINT('Ctrl Pts',(-5.91523813879494,0.154410604020374,
47.8061078604484));
#21411=CARTESIAN_POINT('Ctrl Pts',(-5.91221879226667,0.231515690329624,
47.8024741945702));
#21412=CARTESIAN_POINT('Ctrl Pts',(-5.90574747158356,0.396773879521906,
47.7946862123254));
#21413=CARTESIAN_POINT('Ctrl Pts',(-5.89234171448409,0.561790118658018,
47.7868982300805));
#21414=CARTESIAN_POINT('Ctrl Pts',(-5.87204325230494,0.725974245796646,
47.7791102478357));
#21415=CARTESIAN_POINT('Ctrl Pts',(-5.85174878075666,0.890126094714365,
47.7713237966902));
#21416=CARTESIAN_POINT('Ctrl Pts',(-5.82456434711627,1.05344584110727,47.7635373455446));
#21417=CARTESIAN_POINT('Ctrl Pts',(-5.79058345830377,1.21534923989721,47.7557508943991));
#21418=CARTESIAN_POINT('Ctrl Pts',(-5.75660127282074,1.37725881672939,47.7479641461318));
#21419=CARTESIAN_POINT('Ctrl Pts',(-5.7158221749785,1.53775162427468,47.7401773978645));
#21420=CARTESIAN_POINT('Ctrl Pts',(-5.66839078491173,1.69625365792614,47.7323906495971));
#21421=CARTESIAN_POINT('Ctrl Pts',(-5.62096253184304,1.85474520863424,47.7246044163266));
#21422=CARTESIAN_POINT('Ctrl Pts',(-5.56688295871592,2.01124594280084,47.7168181830561));
#21423=CARTESIAN_POINT('Ctrl Pts',(-5.5063465964238,2.16519692465883,47.7090319497856));
#21424=CARTESIAN_POINT('Ctrl Pts',(-5.44579429801664,2.31918843390339,47.7012436667997));
#21425=CARTESIAN_POINT('Ctrl Pts',(-5.37878192919868,2.47062855130434,47.6934553838139));
#21426=CARTESIAN_POINT('Ctrl Pts',(-5.30555256273948,2.61897738946112,47.685667100828));
#21427=CARTESIAN_POINT('Ctrl Pts',(-5.23593359251548,2.76001224809471,47.6782628002379));
#21428=CARTESIAN_POINT('Ctrl Pts',(-5.16069600116256,2.89825306412585,47.6708584996478));
#21429=CARTESIAN_POINT('Ctrl Pts',(-5.08008754470556,3.03325585808838,47.6634541990577));
#21430=CARTESIAN_POINT('Ctrl Pts',(-4.9953021689467,3.17525414359971,47.6556662269843));
#21431=CARTESIAN_POINT('Ctrl Pts',(-4.90454421118265,3.31372072242619,47.6478782549109));
#21432=CARTESIAN_POINT('Ctrl Pts',(-4.80813280107613,3.44815741080882,47.6400902828376));
#21433=CARTESIAN_POINT('Ctrl Pts',(-4.71174034733736,3.58256766631073,47.6323038420318));
#21434=CARTESIAN_POINT('Ctrl Pts',(-4.60969684529718,3.71294935283312,47.624517401226));
#21435=CARTESIAN_POINT('Ctrl Pts',(-4.50236405122898,3.83883426481282,47.6167309604202));
#21436=CARTESIAN_POINT('Ctrl Pts',(-4.39502716369273,3.96472397780296,47.6089442226544));
#21437=CARTESIAN_POINT('Ctrl Pts',(-4.2824007847869,4.0861163273587,47.6011574848886));
#21438=CARTESIAN_POINT('Ctrl Pts',(-4.16488664625825,4.20257656519422,47.5933707471228));
#21439=CARTESIAN_POINT('Ctrl Pts',(-4.04738028086294,4.31902909960812,47.5855845244215));
#21440=CARTESIAN_POINT('Ctrl Pts',(-3.92498702990236,4.43054995028435,47.5777983017201));
#21441=CARTESIAN_POINT('Ctrl Pts',(-3.79814523366374,4.53674148993497,47.5700120790187));
#21442=CARTESIAN_POINT('Ctrl Pts',(-3.67127004663938,4.64296098424292,47.5622238066137));
#21443=CARTESIAN_POINT('Ctrl Pts',(-3.53994421822294,4.7438481574137,47.5544355342087));
#21444=CARTESIAN_POINT('Ctrl Pts',(-3.40463959049158,4.83904534194063,47.5466472618036));
#21445=CARTESIAN_POINT('Ctrl Pts',(-3.27600474816551,4.9295498208105,47.5392429090508));
#21446=CARTESIAN_POINT('Ctrl Pts',(-3.14377414026063,5.01491161890032,47.531838556298));
#21447=CARTESIAN_POINT('Ctrl Pts',(-3.00837782388234,5.09485951045492,47.5244342035451));
#21448=CARTESIAN_POINT('Ctrl Pts',(-2.86596645185795,5.17894960412437,47.516646221843));
#21449=CARTESIAN_POINT('Ctrl Pts',(-2.72000168091004,5.25707997556426,47.5088582401409));
#21450=CARTESIAN_POINT('Ctrl Pts',(-2.57100217162245,5.3289659781249,47.5010702584388));
#21451=CARTESIAN_POINT('Ctrl Pts',(-2.4220319558704,5.4008378477855,47.4932838078661));
#21452=CARTESIAN_POINT('Ctrl Pts',(-2.27002847986774,5.46646765932704,47.4854973572933));
#21453=CARTESIAN_POINT('Ctrl Pts',(-2.11553348056156,5.52561749084418,47.4777109067205));
#21454=CARTESIAN_POINT('Ctrl Pts',(-1.96103258672679,5.5847695791358,47.4699241590672));
#21455=CARTESIAN_POINT('Ctrl Pts',(-1.8040402763721,5.63744107473975,47.4621374114139));
#21456=CARTESIAN_POINT('Ctrl Pts',(-1.64511736981318,5.68344256608959,47.4543506637606));
#21457=CARTESIAN_POINT('Ctrl Pts',(-1.48620497447095,5.72944101488468,47.4465644311255));
#21458=CARTESIAN_POINT('Ctrl Pts',(-1.32536254545813,5.76877025349844,47.4387781984904));
#21459=CARTESIAN_POINT('Ctrl Pts',(-1.16316527660633,5.80129098578905,47.4309919658554));
#21460=CARTESIAN_POINT('Ctrl Pts',(-1.0009253101604,5.83382027899464,47.4232036835347));
#21461=CARTESIAN_POINT('Ctrl Pts',(-0.837330104342507,5.85953741969641,
47.4154154012141));
#21462=CARTESIAN_POINT('Ctrl Pts',(-0.672965139961038,5.87835423251247,
47.4076271188934));
#21463=CARTESIAN_POINT('Ctrl Pts',(-0.516703714051457,5.89624333687711,
47.4002228152732));
#21464=CARTESIAN_POINT('Ctrl Pts',(-0.35974686430779,5.90789609377089,47.3928185116529));
#21465=CARTESIAN_POINT('Ctrl Pts',(-0.202601995391641,5.91328022285122,
47.3854142080327));
#21466=CARTESIAN_POINT('Ctrl Pts',(-0.0373142810084133,5.91894334373941,
47.3776262323232));
#21467=CARTESIAN_POINT('Ctrl Pts',(0.12824058182807,5.91767296532762,47.3698382566137));
#21468=CARTESIAN_POINT('Ctrl Pts',(0.293470960870003,5.90946743434855,47.3620502809042));
#21469=CARTESIAN_POINT('Ctrl Pts',(0.458668853635842,5.90126351667538,47.3542638364042));
#21470=CARTESIAN_POINT('Ctrl Pts',(0.623542070940536,5.88612718292717,47.3464773919043));
#21471=CARTESIAN_POINT('Ctrl Pts',(0.787501085140527,5.86410884989378,47.3386909474043));
#21472=CARTESIAN_POINT('Ctrl Pts',(0.951466353570333,5.84208967696929,47.3309042058898));
#21473=CARTESIAN_POINT('Ctrl Pts',(1.11451703189257,5.81318801807413,47.3231174643753));
#21474=CARTESIAN_POINT('Ctrl Pts',(1.27607005762088,5.777506016487,47.3153307228608));
#21475=CARTESIAN_POINT('Ctrl Pts',(1.43761239767306,5.74182637503092,47.3075444963883));
#21476=CARTESIAN_POINT('Ctrl Pts',(1.59765697133325,5.6993673573832,47.2997582699158));
#21477=CARTESIAN_POINT('Ctrl Pts',(1.75563208481372,5.65028198811994,47.2919720434433));
#21478=CARTESIAN_POINT('Ctrl Pts',(1.91364878485282,5.6011836972544,47.284183767266));
#21479=CARTESIAN_POINT('Ctrl Pts',(2.06959463018358,5.54545566216622,47.2763954910886));
#21480=CARTESIAN_POINT('Ctrl Pts',(2.22291336491067,5.48330071531751,47.2686072149112));
#21481=CARTESIAN_POINT('Ctrl Pts',(2.36867387911287,5.42420984798806,47.2612028807808));
#21482=CARTESIAN_POINT('Ctrl Pts',(2.51205981894196,5.35931056493724,47.2537985466505));
#21483=CARTESIAN_POINT('Ctrl Pts',(2.65261022735003,5.28881740507819,47.2463942125201));
#21484=CARTESIAN_POINT('Ctrl Pts',(2.80044304389721,5.21467174810495,47.2386062339468));
#21485=CARTESIAN_POINT('Ctrl Pts',(2.94519157314257,5.1343106245189,47.2308182553735));
#21486=CARTESIAN_POINT('Ctrl Pts',(3.08633557248104,5.0480157781586,47.2230302768002));
#21487=CARTESIAN_POINT('Ctrl Pts',(3.22745182187502,4.96173789799741,47.2152438294006));
#21488=CARTESIAN_POINT('Ctrl Pts',(3.36496468291711,4.8695287893827,47.207457382001));
#21489=CARTESIAN_POINT('Ctrl Pts',(3.49838068508846,4.77171490605841,47.1996709346013));
#21490=CARTESIAN_POINT('Ctrl Pts',(3.63180177689697,4.67389729126887,47.1918841901594));
#21491=CARTESIAN_POINT('Ctrl Pts',(3.76112543705835,4.57047465966712,47.1840974457175));
#21492=CARTESIAN_POINT('Ctrl Pts',(3.88588863122912,4.46181578599837,47.1763107012756));
#21493=CARTESIAN_POINT('Ctrl Pts',(4.01064357328261,4.35316409927105,47.1685244718664));
#21494=CARTESIAN_POINT('Ctrl Pts',(4.13083841205318,4.23927707351932,47.1607382424572));
#21495=CARTESIAN_POINT('Ctrl Pts',(4.2460444500956,4.12056271525048,47.1529520130481));
#21496=CARTESIAN_POINT('Ctrl Pts',(4.36128081564456,4.00181710592449,47.1451637339466));
#21497=CARTESIAN_POINT('Ctrl Pts',(4.47152553215949,3.87824185291479,47.1373754548452));
#21498=CARTESIAN_POINT('Ctrl Pts',(4.57638729802127,3.75028130425033,47.1295871757438));
#21499=CARTESIAN_POINT('Ctrl Pts',(4.67607941433032,3.62862916730995,47.1221828561651));
#21500=CARTESIAN_POINT('Ctrl Pts',(4.77090638293935,3.5030139099496,47.1147785365864));
#21501=CARTESIAN_POINT('Ctrl Pts',(4.86056617987861,3.3738445390267,47.1073742170077));
#21502=CARTESIAN_POINT('Ctrl Pts',(4.95487173760899,3.23798220180973,47.0995862394378));
#21503=CARTESIAN_POINT('Ctrl Pts',(5.04349416322125,3.09813905595918,47.0917982618679));
#21504=CARTESIAN_POINT('Ctrl Pts',(5.12611154720542,2.95481149451318,47.084010284298));
#21505=CARTESIAN_POINT('Ctrl Pts',(5.20871268788547,2.811512112526,47.076223837913));
#21506=CARTESIAN_POINT('Ctrl Pts',(5.28531098318517,2.66472995853285,47.068437391528));
#21507=CARTESIAN_POINT('Ctrl Pts',(5.35562943055617,2.51498786578794,47.060650945143));
#21508=CARTESIAN_POINT('Ctrl Pts',(5.42595056041088,2.36524006073369,47.0528642017234));
#21509=CARTESIAN_POINT('Ctrl Pts',(5.48999122356693,2.21253237853772,47.0450774583037));
#21510=CARTESIAN_POINT('Ctrl Pts',(5.5475213980055,2.0574102413401,47.0372907148841));
#21511=CARTESIAN_POINT('Ctrl Pts',(5.60504776725328,1.90229836431174,47.0295044864993));
#21512=CARTESIAN_POINT('Ctrl Pts',(5.65606439849992,1.74477265153495,47.0217182581145));
#21513=CARTESIAN_POINT('Ctrl Pts',(5.70039019635951,1.58539653454536,47.0139320297296));
#21514=CARTESIAN_POINT('Ctrl Pts',(5.74472766283695,1.42597846232665,47.0061437516463));
#21515=CARTESIAN_POINT('Ctrl Pts',(5.78237068883484,1.26470932008741,46.9983554735629));
#21516=CARTESIAN_POINT('Ctrl Pts',(5.81318840786456,1.10216654692885,46.9905671954796));
#21517=CARTESIAN_POINT('Ctrl Pts',(5.84248684772252,0.947636951174592,46.9831628708181));
#21518=CARTESIAN_POINT('Ctrl Pts',(5.8656166809451,0.79195653557368,46.9757585461566));
#21519=CARTESIAN_POINT('Ctrl Pts',(5.88250850967426,0.63562897677016,46.9683542214951));
#21520=CARTESIAN_POINT('Ctrl Pts',(5.90027558389392,0.471201348218344,46.9605662437743));
#21521=CARTESIAN_POINT('Ctrl Pts',(5.91114740556107,0.305998913864915,46.9527782660534));
#21522=CARTESIAN_POINT('Ctrl Pts',(5.91507894643294,0.140611592572644,46.9449902883326));
#21523=CARTESIAN_POINT('Ctrl Pts',(5.91900971432966,-0.0247432121329748,
46.9372038417959));
#21524=CARTESIAN_POINT('Ctrl Pts',(5.91600291646002,-0.190282511983973,
46.9294173952592));
#21525=CARTESIAN_POINT('Ctrl Pts',(5.90606560879723,-0.355414669200131,
46.9216309487226));
#21526=CARTESIAN_POINT('Ctrl Pts',(5.89612792205001,-0.520553125811444,
46.9138442051517));
#21527=CARTESIAN_POINT('Ctrl Pts',(5.87925921172332,-0.685284089509624,
46.9060574615808));
#21528=CARTESIAN_POINT('Ctrl Pts',(5.85551859508534,-0.849018577599937,
46.8982707180099));
#21529=CARTESIAN_POINT('Ctrl Pts',(5.83177954871321,-1.01274223586728,46.8904844894744));
#21530=CARTESIAN_POINT('Ctrl Pts',(5.80116955157325,-1.17546923416822,46.8826982609389));
#21531=CARTESIAN_POINT('Ctrl Pts',(5.76379929884797,-1.33661819720503,46.8749120324034));
#21532=CARTESIAN_POINT('Ctrl Pts',(5.72641920854025,-1.49780958211737,46.8671237541717));
#21533=CARTESIAN_POINT('Ctrl Pts',(5.68227537693676,-1.65742178974595,46.85933547594));
#21534=CARTESIAN_POINT('Ctrl Pts',(5.63152930497246,-1.81488518913357,46.8515471977083));
#21535=CARTESIAN_POINT('Ctrl Pts',(5.5832849635749,-1.96458580050346,46.8441428737997));
#21536=CARTESIAN_POINT('Ctrl Pts',(5.52907374942506,-2.11234411743046,46.8367385498912));
#21537=CARTESIAN_POINT('Ctrl Pts',(5.4690758249451,-2.25768469532418,46.8293342259826));
#21538=CARTESIAN_POINT('Ctrl Pts',(5.40596911694961,-2.41055607360159,46.8215462481342));
#21539=CARTESIAN_POINT('Ctrl Pts',(5.33643752795683,-2.56080719631072,46.8137582702858));
#21540=CARTESIAN_POINT('Ctrl Pts',(5.26072389823664,-2.70789856328148,46.8059702924374));
#21541=CARTESIAN_POINT('Ctrl Pts',(5.18502515445198,-2.85496101085406,46.7981838457709));
#21542=CARTESIAN_POINT('Ctrl Pts',(5.10314694126047,-2.99886465828883,46.7903973991044));
#21543=CARTESIAN_POINT('Ctrl Pts',(5.01537865147266,-3.13909342722581,46.7826109524378));
#21544=CARTESIAN_POINT('Ctrl Pts',(4.92760701350867,-3.27932754559623,46.7748242087346));
#21545=CARTESIAN_POINT('Ctrl Pts',(4.83394501550904,-3.41588623199086,46.7670374650315));
#21546=CARTESIAN_POINT('Ctrl Pts',(4.73472648900826,-3.5482806592466,46.7592507213283));
#21547=CARTESIAN_POINT('Ctrl Pts',(4.6355145250644,-3.68066632960991,46.7514644926595));
#21548=CARTESIAN_POINT('Ctrl Pts',(4.53074695982799,-3.80888803635458,46.7436782639907));
#21549=CARTESIAN_POINT('Ctrl Pts',(4.42079926864124,-3.93248832024725,46.7358920353219));
#21550=CARTESIAN_POINT('Ctrl Pts',(4.31082263412062,-4.05612114146967,46.7281037569564));
#21551=CARTESIAN_POINT('Ctrl Pts',(4.19566335985543,-4.17512986865475,46.720315478591));
#21552=CARTESIAN_POINT('Ctrl Pts',(4.07573590682066,-4.28909167311132,46.7125272002255));
#21553=CARTESIAN_POINT('Ctrl Pts',(3.9617207692809,-4.39743526317843,46.7051228769737));
#21554=CARTESIAN_POINT('Ctrl Pts',(3.84339645293024,-4.50121737957754,46.6977185537218));
#21555=CARTESIAN_POINT('Ctrl Pts',(3.72114871939846,-4.60010682165308,46.69031423047));
#21556=CARTESIAN_POINT('Ctrl Pts',(3.5925667289145,-4.70412021259759,46.6825262527759));
#21557=CARTESIAN_POINT('Ctrl Pts',(3.45959794722756,-4.80275764836333,46.6747382750817));
#21558=CARTESIAN_POINT('Ctrl Pts',(3.32271382828637,-4.89566168947718,46.6669502973876));
#21559=CARTESIAN_POINT('Ctrl Pts',(3.18585662195332,-4.98854746484865,46.6591638508776));
#21560=CARTESIAN_POINT('Ctrl Pts',(3.04508587856359,-5.07570191539245,46.6513774043676));
#21561=CARTESIAN_POINT('Ctrl Pts',(2.90090271377241,-5.15681044907876,46.6435909578576));
#21562=CARTESIAN_POINT('Ctrl Pts',(2.75671404873331,-5.23792207686447,46.635804214313));
#21563=CARTESIAN_POINT('Ctrl Pts',(2.60911297836769,-5.31298716617101,46.6280174707684));
#21564=CARTESIAN_POINT('Ctrl Pts',(2.45862659111139,-5.38173632278468,46.6202307272238));
#21565=CARTESIAN_POINT('Ctrl Pts',(2.30815015740981,-5.45048093215322,46.6124444987143));
#21566=CARTESIAN_POINT('Ctrl Pts',(2.15478907944805,-5.51291031212031,46.6046582702049));
#21567=CARTESIAN_POINT('Ctrl Pts',(1.99909199397069,-5.56880254292988,46.5968720416954));
#21568=CARTESIAN_POINT('Ctrl Pts',(1.84335392179122,-5.62470948716975,46.5890837634891));
#21569=CARTESIAN_POINT('Ctrl Pts',(1.68527891360305,-5.67407573368967,46.5812954852828));
#21570=CARTESIAN_POINT('Ctrl Pts',(1.52543325888557,-5.71672842937162,46.5735072070765));
#21571=CARTESIAN_POINT('Ctrl Pts',(1.37346783180315,-5.75727839068888,46.5661028830368));
#21572=CARTESIAN_POINT('Ctrl Pts',(1.21990238946817,-5.79176073038744,46.5586985589971));
#21573=CARTESIAN_POINT('Ctrl Pts',(1.06523416428594,-5.82006930695314,46.5512942349575));
#21574=CARTESIAN_POINT('Ctrl Pts',(0.902551831972747,-5.84984468747975,
46.5435062571582));
#21575=CARTESIAN_POINT('Ctrl Pts',(0.738591207079472,-5.8728001851706,46.5357182793589));
#21576=CARTESIAN_POINT('Ctrl Pts',(0.573937319065931,-5.88884763907875,
46.5279303015596));
#21577=CARTESIAN_POINT('Ctrl Pts',(0.409315803407721,-5.90489193792093,
46.520143854943));
#21578=CARTESIAN_POINT('Ctrl Pts',(0.244001614438643,-5.91403087197179,
46.5123574083264));
#21579=CARTESIAN_POINT('Ctrl Pts',(0.0785853148167597,-5.91622809827302,
46.5045709617098));
#21580=CARTESIAN_POINT('Ctrl Pts',(-0.0868372950723568,-5.91842540839359,
46.4967842180574));
#21581=CARTESIAN_POINT('Ctrl Pts',(-0.252361703950604,-5.91368047267539,
46.4889974744051));
#21582=CARTESIAN_POINT('Ctrl Pts',(-0.417396179871646,-5.90200906399919,
46.4812107307527));
#21583=CARTESIAN_POINT('Ctrl Pts',(-0.58241973999981,-5.89033842729914,
46.473424502135));
#21584=CARTESIAN_POINT('Ctrl Pts',(-0.74695311324624,-5.87174225709385,
46.4656382735173));
#21585=CARTESIAN_POINT('Ctrl Pts',(-0.910408372800225,-5.84628832313591,
46.4578520448996));
#21586=CARTESIAN_POINT('Ctrl Pts',(-1.07390666136105,-5.82082768852177,
46.4500637665854));
#21587=CARTESIAN_POINT('Ctrl Pts',(-1.23632595286218,-5.78850573009129,
46.4422754882712));
#21588=CARTESIAN_POINT('Ctrl Pts',(-1.39708630805294,-5.74944174771351,
46.4344872099569));
#21589=CARTESIAN_POINT('Ctrl Pts',(-1.54992132863309,-5.71230358299892,
46.427082886453));
#21590=CARTESIAN_POINT('Ctrl Pts',(-1.7012567847426,-5.66907219451902,46.419678562949));
#21591=CARTESIAN_POINT('Ctrl Pts',(-1.85060530178236,-5.61989239928266,
46.4122742394451));
#21592=CARTESIAN_POINT('Ctrl Pts',(-2.00769229647846,-5.56816435814387,
46.4044862616998));
#21593=CARTESIAN_POINT('Ctrl Pts',(-2.16263717236233,-5.50983660796316,
46.3966982839546));
#21594=CARTESIAN_POINT('Ctrl Pts',(-2.31488407594503,-5.44511177823157,
46.3889103062093));
#21595=CARTESIAN_POINT('Ctrl Pts',(-2.46710104647754,-5.38039967395797,
46.3811238596475));
#21596=CARTESIAN_POINT('Ctrl Pts',(-2.61662080920446,-5.30929312460174,
46.3733374130856));
#21597=CARTESIAN_POINT('Ctrl Pts',(-2.76290745608669,-5.23204290422017,
46.3655509665237));
#21598=CARTESIAN_POINT('Ctrl Pts',(-2.9091996834718,-5.15478973691838,46.3577642229266));
#21599=CARTESIAN_POINT('Ctrl Pts',(-3.0522582638074,-5.07139257533503,46.3499774793295));
#21600=CARTESIAN_POINT('Ctrl Pts',(-3.19157120857266,-4.98214851074414,
46.3421907357324));
#21601=CARTESIAN_POINT('Ctrl Pts',(-3.33087493882796,-4.89291034898104,
46.3344045071702));
#21602=CARTESIAN_POINT('Ctrl Pts',(-3.46643326025359,-4.79782623059214,
46.326618278608));
#21603=CARTESIAN_POINT('Ctrl Pts',(-3.59776241442733,-4.69723707852116,
46.3188320500458));
#21604=CARTESIAN_POINT('Ctrl Pts',(-3.72912614053044,-4.59662144671625,
46.3110437717868));
#21605=CARTESIAN_POINT('Ctrl Pts',(-3.85625821970206,-4.49049807834508,
46.3032554935278));
#21606=CARTESIAN_POINT('Ctrl Pts',(-3.97870657235139,-4.37924931622166,
46.2954672152689));
#21607=CARTESIAN_POINT('Ctrl Pts',(-4.09511834130026,-4.27348500896921,
46.2880628914901));
#21608=CARTESIAN_POINT('Ctrl Pts',(-4.2072968706866,-4.16308866564848,46.2806585677113));
#21609=CARTESIAN_POINT('Ctrl Pts',(-4.31488356651933,-4.0484207254041,46.2732542439325));
#21610=CARTESIAN_POINT('Ctrl Pts',(-4.42804485175323,-3.92781128208266,
46.2654662661662));
#21611=CARTESIAN_POINT('Ctrl Pts',(-4.53616629937832,-3.80243268057,46.2576782883999));
#21612=CARTESIAN_POINT('Ctrl Pts',(-4.63885686417549,-3.67272889772604,
46.2498903106336));
#21613=CARTESIAN_POINT('Ctrl Pts',(-4.74152723912757,-3.54305061575734,
46.2421038640504));
#21614=CARTESIAN_POINT('Ctrl Pts',(-4.83876866350964,-3.40904909957154,
46.2343174174673));
#21615=CARTESIAN_POINT('Ctrl Pts',(-4.9302306493656,-3.27120104954679,46.2265309708841));
#21616=CARTESIAN_POINT('Ctrl Pts',(-5.02169612429075,-3.13334774092878,
46.2187442272656));
#21617=CARTESIAN_POINT('Ctrl Pts',(-5.10738153956141,-2.99164786892421,
46.210957483647));
#21618=CARTESIAN_POINT('Ctrl Pts',(-5.18697957900952,-2.84660735076656,
46.2031707400284));
#21619=CARTESIAN_POINT('Ctrl Pts',(-5.26657235364277,-2.70157642595418,
46.1953845114447));
#21620=CARTESIAN_POINT('Ctrl Pts',(-5.34007840453294,-2.55320557737503,
46.1875982828609));
#21621=CARTESIAN_POINT('Ctrl Pts',(-5.40723618222366,-2.40202569348276,
46.1798120542772));
#21622=CARTESIAN_POINT('Ctrl Pts',(-5.47441163895776,-2.2508060120299,46.1720237759968));
#21623=CARTESIAN_POINT('Ctrl Pts',(-5.53523535156062,-2.09677610908315,
46.1642354977164));
#21624=CARTESIAN_POINT('Ctrl Pts',(-5.58949341081284,-1.94048807596951,
46.156447219436));
#21625=CARTESIAN_POINT('Ctrl Pts',(-5.64107660006892,-1.79190489216843,
46.149042895764));
#21626=CARTESIAN_POINT('Ctrl Pts',(-5.68672581629164,-1.64128111112891,
46.141638572092));
#21627=CARTESIAN_POINT('Ctrl Pts',(-5.72629874571322,-1.48910484430855,
46.13423424842));
#21628=CARTESIAN_POINT('Ctrl Pts',(-5.76840197275352,-1.32719840963888,
46.1263564914483));
#21629=CARTESIAN_POINT('Ctrl Pts',(-5.80364017635744,-1.16348277679236,
46.1184787344766));
#21630=CARTESIAN_POINT('Ctrl Pts',(-5.83188064495595,-0.998548299026231,
46.1106009775049));
#21631=CARTESIAN_POINT('Ctrl Pts',(-5.8601159255073,-0.833644121318528,
46.1027246677533));
#21632=CARTESIAN_POINT('Ctrl Pts',(-5.88135598412391,-0.667521844660853,
46.0948483580017));
#21633=CARTESIAN_POINT('Ctrl Pts',(-5.8955193839581,-0.500781145685749,
46.0869720482502));
#21634=CARTESIAN_POINT('Ctrl Pts',(-5.90966355881241,-0.334266775601957,
46.0791064295684));
#21635=CARTESIAN_POINT('Ctrl Pts',(-5.916750252318,-0.167135962851299,46.0712408108866));
#21636=CARTESIAN_POINT('Ctrl Pts',(-5.91674999999326,8.93202511665269E-6,
46.0633751922049));
#21637=CARTESIAN_POINT('Ctrl Pts',(-5.9167499982011,-0.000145901520597427,
45.811624807825));
#21638=CARTESIAN_POINT('Ctrl Pts',(-5.91674574497461,-0.172627159573382,
45.8197432531791));
#21639=CARTESIAN_POINT('Ctrl Pts',(-5.90919506021176,-0.345071345143527,
45.8278616985332));
#21640=CARTESIAN_POINT('Ctrl Pts',(-5.89413362177757,-0.516835961530533,
45.8359801438873));
#21641=CARTESIAN_POINT('Ctrl Pts',(-5.88403693874417,-0.631981197863106,
45.8414224772887));
#21642=CARTESIAN_POINT('Ctrl Pts',(-5.8705660667189,-0.746821081022063,
45.8468648106901));
#21643=CARTESIAN_POINT('Ctrl Pts',(-5.85374480608386,-0.861163345565901,
45.8523071440916));
#21644=CARTESIAN_POINT('Ctrl Pts',(-5.82967317321384,-1.02478990562834,
45.8600952554845));
#21645=CARTESIAN_POINT('Ctrl Pts',(-5.79873229853884,-1.18743575353866,
45.8678833668775));
#21646=CARTESIAN_POINT('Ctrl Pts',(-5.7610266728846,-1.34851853410037,45.8756714782704));
#21647=CARTESIAN_POINT('Ctrl Pts',(-5.7233284500727,-1.50956968886598,45.8834580606035));
#21648=CARTESIAN_POINT('Ctrl Pts',(-5.6788681990981,-1.66905807767523,45.8912446429365));
#21649=CARTESIAN_POINT('Ctrl Pts',(-5.62780125897437,-1.82641275509849,
45.8990312252695));
#21650=CARTESIAN_POINT('Ctrl Pts',(-5.57673237167957,-1.98377343242065,
45.9068181045032));
#21651=CARTESIAN_POINT('Ctrl Pts',(-5.51905638603465,-2.13899993042873,
45.9146049837369));
#21652=CARTESIAN_POINT('Ctrl Pts',(-5.45497836904886,-2.29153694181636,
45.9223918629706));
#21653=CARTESIAN_POINT('Ctrl Pts',(-5.3909045811751,-2.44406388584953,45.9301782282748));
#21654=CARTESIAN_POINT('Ctrl Pts',(-5.32042973137928,-2.59390140390795,
45.9379645935789));
#21655=CARTESIAN_POINT('Ctrl Pts',(-5.2438069038857,-2.74051449864085,45.9457509588831));
#21656=CARTESIAN_POINT('Ctrl Pts',(-5.16716395679363,-2.88716609099508,
45.9535393687286));
#21657=CARTESIAN_POINT('Ctrl Pts',(-5.08436995260354,-3.03059128393218,
45.9613277785742));
#21658=CARTESIAN_POINT('Ctrl Pts',(-4.99572420636531,-3.17027920165334,
45.9691161884198));
#21659=CARTESIAN_POINT('Ctrl Pts',(-4.91173696773099,-3.30262624567786,
45.9764953020721));
#21660=CARTESIAN_POINT('Ctrl Pts',(-4.82249734826175,-3.43161849408526,
45.9838744157243));
#21661=CARTESIAN_POINT('Ctrl Pts',(-4.72829602237616,-3.55684513119166,
45.9912535293766));
#21662=CARTESIAN_POINT('Ctrl Pts',(-4.62887345566512,-3.68901263058366,
45.9990416407696));
#21663=CARTESIAN_POINT('Ctrl Pts',(-4.52388805820152,-3.81703245673406,
46.0068297521625));
#21664=CARTESIAN_POINT('Ctrl Pts',(-4.41371020502661,-3.94044322234745,
46.0146178635555));
#21665=CARTESIAN_POINT('Ctrl Pts',(-4.30355398335264,-4.06382975840822,
46.0224044458885));
#21666=CARTESIAN_POINT('Ctrl Pts',(-4.18820755273805,-4.18260880128283,
46.0301910282216));
#21667=CARTESIAN_POINT('Ctrl Pts',(-4.0680804803437,-4.2963533104188,46.0379776105546));
#21668=CARTESIAN_POINT('Ctrl Pts',(-3.94794882753073,-4.41010215660767,
46.0457644897883));
#21669=CARTESIAN_POINT('Ctrl Pts',(-3.82303639748256,-4.51881586238337,
46.053551369022));
#21670=CARTESIAN_POINT('Ctrl Pts',(-3.69378894281856,-4.62210491101309,
46.0613382482558));
#21671=CARTESIAN_POINT('Ctrl Pts',(-3.56455001841176,-4.7253871426254,46.0691246135599));
#21672=CARTESIAN_POINT('Ctrl Pts',(-3.43097689164286,-4.82324523415024,
46.0769109788641));
#21673=CARTESIAN_POINT('Ctrl Pts',(-3.29354776314487,-4.91533047661939,
46.0846973441683));
#21674=CARTESIAN_POINT('Ctrl Pts',(-3.15608254854857,-5.0074398988032,46.0924857540139));
#21675=CARTESIAN_POINT('Ctrl Pts',(-3.01475957356343,-5.0937732633865,46.1002741638595));
#21676=CARTESIAN_POINT('Ctrl Pts',(-2.87008609456459,-5.17402516154367,
46.1080625737051));
#21677=CARTESIAN_POINT('Ctrl Pts',(-2.73301549027402,-5.250059665255,46.1154416873573));
#21678=CARTESIAN_POINT('Ctrl Pts',(-2.5929377030047,-5.32063532214679,46.1228208010096));
#21679=CARTESIAN_POINT('Ctrl Pts',(-2.45030452930873,-5.38553045448163,
46.1301999146618));
#21680=CARTESIAN_POINT('Ctrl Pts',(-2.29976571158208,-5.45402249069423,
46.1379880260548));
#21681=CARTESIAN_POINT('Ctrl Pts',(-2.14632643833284,-5.51621090595828,
46.1457761374478));
#21682=CARTESIAN_POINT('Ctrl Pts',(-1.99053268829148,-5.5718677460384,46.1535642488408));
#21683=CARTESIAN_POINT('Ctrl Pts',(-1.83476952563732,-5.62751365886812,
46.1613508311738));
#21684=CARTESIAN_POINT('Ctrl Pts',(-1.67665310925573,-5.67663044777479,
46.1691374135069));
#21685=CARTESIAN_POINT('Ctrl Pts',(-1.51674740067902,-5.71903907007405,
46.1769239958399));
#21686=CARTESIAN_POINT('Ctrl Pts',(-1.35683559493295,-5.76144930940471,
46.1847108750737));
#21687=CARTESIAN_POINT('Ctrl Pts',(-1.19513466829972,-5.79715078458653,
46.1924977543074));
#21688=CARTESIAN_POINT('Ctrl Pts',(-1.03222240487017,-5.82601471585715,
46.2002846335411));
#21689=CARTESIAN_POINT('Ctrl Pts',(-0.869320893555808,-5.85487674212499,
46.2080709988453));
#21690=CARTESIAN_POINT('Ctrl Pts',(-0.70520852010587,-5.8769020719177,46.2158573641495));
#21691=CARTESIAN_POINT('Ctrl Pts',(-0.540472038079021,-5.89201328397643,
46.2236437294537));
#21692=CARTESIAN_POINT('Ctrl Pts',(-0.375692299597308,-5.90712846393258,
46.2314321392993));
#21693=CARTESIAN_POINT('Ctrl Pts',(-0.210288443300414,-5.91532586725346,
46.2392205491449));
#21694=CARTESIAN_POINT('Ctrl Pts',(-0.0448520209422557,-5.91657999681551,
46.2470089589905));
#21695=CARTESIAN_POINT('Ctrl Pts',(0.111890393360747,-5.91776821941246,
46.2543880726427));
#21696=CARTESIAN_POINT('Ctrl Pts',(0.268661778863087,-5.91272416162945,
46.2617671862948));
#21697=CARTESIAN_POINT('Ctrl Pts',(0.424959344252692,-5.90146931858773,
46.2691462999469));
#21698=CARTESIAN_POINT('Ctrl Pts',(0.589919921780186,-5.88959066005894,
46.2769344113398));
#21699=CARTESIAN_POINT('Ctrl Pts',(0.754411580958356,-5.87078896788286,
46.2847225227327));
#21700=CARTESIAN_POINT('Ctrl Pts',(0.917845824056466,-5.8451252857199,46.2925106341257));
#21701=CARTESIAN_POINT('Ctrl Pts',(1.08124797968991,-5.81946664217356,46.3002972164587));
#21702=CARTESIAN_POINT('Ctrl Pts',(1.24359281801192,-5.78694874630574,46.3080837987917));
#21703=CARTESIAN_POINT('Ctrl Pts',(1.4042994511938,-5.74768419573282,46.3158703811247));
#21704=CARTESIAN_POINT('Ctrl Pts',(1.56501221208391,-5.70841814801131,46.3236572603584));
#21705=CARTESIAN_POINT('Ctrl Pts',(1.72408633151957,-5.66240500282972,46.331444139592));
#21706=CARTESIAN_POINT('Ctrl Pts',(1.88095283132228,-5.60980810802301,46.3392310188257));
#21707=CARTESIAN_POINT('Ctrl Pts',(2.03780897802685,-5.5572146845809,46.3470173841298));
#21708=CARTESIAN_POINT('Ctrl Pts',(2.19245749373133,-5.49803848276105,46.354803749434));
#21709=CARTESIAN_POINT('Ctrl Pts',(2.34434609568193,-5.43249224078239,46.3625901147381));
#21710=CARTESIAN_POINT('Ctrl Pts',(2.49627458049495,-5.36692878769167,46.3703785245837));
#21711=CARTESIAN_POINT('Ctrl Pts',(2.64544140911902,-5.29499207705749,46.3781669344292));
#21712=CARTESIAN_POINT('Ctrl Pts',(2.79131492773295,-5.21694273849304,46.3859553442748));
#21713=CARTESIAN_POINT('Ctrl Pts',(2.92952250721046,-5.14299504555116,46.3933344579272));
#21714=CARTESIAN_POINT('Ctrl Pts',(3.06477378425196,-5.06356078410268,46.4007135715797));
#21715=CARTESIAN_POINT('Ctrl Pts',(3.19663753035329,-4.97889938259821,46.4080926852321));
#21716=CARTESIAN_POINT('Ctrl Pts',(3.33581000982796,-4.88954550398078,46.4158807966251));
#21717=CARTESIAN_POINT('Ctrl Pts',(3.47125849796741,-4.79433669856308,46.4236689080181));
#21718=CARTESIAN_POINT('Ctrl Pts',(3.6024954269207,-4.69360812824371,46.431457019411));
#21719=CARTESIAN_POINT('Ctrl Pts',(3.73370658979074,-4.59289933422321,46.4392436017441));
#21720=CARTESIAN_POINT('Ctrl Pts',(3.86070759000126,-4.48667313205314,46.4470301840772));
#21721=CARTESIAN_POINT('Ctrl Pts',(3.98304220736054,-4.37530631349218,46.4548167664102));
#21722=CARTESIAN_POINT('Ctrl Pts',(4.1053814893116,-4.26393524853917,46.462603645644));
#21723=CARTESIAN_POINT('Ctrl Pts',(4.22305379344426,-4.14742338715017,46.4703905248777));
#21724=CARTESIAN_POINT('Ctrl Pts',(4.33563763839668,-4.02618638801262,46.4781774041114));
#21725=CARTESIAN_POINT('Ctrl Pts',(4.44821405288046,-3.90495739044687,46.4859637694156));
#21726=CARTESIAN_POINT('Ctrl Pts',(4.55570246288126,-3.77900411344552,46.4937501347198));
#21727=CARTESIAN_POINT('Ctrl Pts',(4.65771967777217,-3.64877759883963,46.501536500024));
#21728=CARTESIAN_POINT('Ctrl Pts',(4.75976368031205,-3.51851688939553,46.5093249098696));
#21729=CARTESIAN_POINT('Ctrl Pts',(4.85633341835975,-3.38398095073037,46.5171133197152));
#21730=CARTESIAN_POINT('Ctrl Pts',(4.9470867289568,-3.24565300959291,46.5249017295608));
#21731=CARTESIAN_POINT('Ctrl Pts',(5.03307077531267,-3.11459447272162,46.532280843213));
#21732=CARTESIAN_POINT('Ctrl Pts',(5.11383385716742,-2.98013245414141,46.5396599568651));
#21733=CARTESIAN_POINT('Ctrl Pts',(5.18912142264732,-2.84270107881969,46.5470390705172));
#21734=CARTESIAN_POINT('Ctrl Pts',(5.26858190721559,-2.69765237644318,46.5548271819105));
#21735=CARTESIAN_POINT('Ctrl Pts',(5.34197106653847,-2.54924401797225,46.5626152933037));
#21736=CARTESIAN_POINT('Ctrl Pts',(5.40902110942795,-2.39800358637405,46.570403404697));
#21737=CARTESIAN_POINT('Ctrl Pts',(5.47605798821034,-2.24679284819814,46.5781899870303));
#21738=CARTESIAN_POINT('Ctrl Pts',(5.53675810443455,-2.09275143826518,46.5859765693637));
#21739=CARTESIAN_POINT('Ctrl Pts',(5.59090111120075,-1.93642849784706,46.593763151697));
#21740=CARTESIAN_POINT('Ctrl Pts',(5.64504618242775,-1.78009959687001,46.601550030931));
#21741=CARTESIAN_POINT('Ctrl Pts',(5.69263353560257,-1.62148929195939,46.609336910165));
#21742=CARTESIAN_POINT('Ctrl Pts',(5.73349192409416,-1.46116423404319,46.617123789399));
#21743=CARTESIAN_POINT('Ctrl Pts',(5.77434761595574,-1.30084975748813,46.6249101547034));
#21744=CARTESIAN_POINT('Ctrl Pts',(5.80847515306132,-1.13882106408848,46.6326965200079));
#21745=CARTESIAN_POINT('Ctrl Pts',(5.83575384129191,-0.975657555880504,
46.6404828853124));
#21746=CARTESIAN_POINT('Ctrl Pts',(5.86303969235206,-0.81245120424876,46.6482712951582));
#21747=CARTESIAN_POINT('Ctrl Pts',(5.88347304638301,-0.648109757425478,
46.6560597050041));
#21748=CARTESIAN_POINT('Ctrl Pts',(5.8969846349975,-0.483221250674439,46.66384811485));
#21749=CARTESIAN_POINT('Ctrl Pts',(5.90978616316074,-0.326997957974139,
46.6712272285008));
#21750=CARTESIAN_POINT('Ctrl Pts',(5.9163746975525,-0.170283883823899,46.6786063421515));
#21751=CARTESIAN_POINT('Ctrl Pts',(5.91673441105521,-0.0135820298596808,
46.6859854558023));
#21752=CARTESIAN_POINT('Ctrl Pts',(5.9171140621842,0.15180524452064,46.6937735671945));
#21753=CARTESIAN_POINT('Ctrl Pts',(5.91055496608031,0.317237973511844,46.7015616785868));
#21754=CARTESIAN_POINT('Ctrl Pts',(5.89707438348461,0.482124753720084,46.709349789979));
#21755=CARTESIAN_POINT('Ctrl Pts',(5.8835964475663,0.646979161283371,46.7171363723114));
#21756=CARTESIAN_POINT('Ctrl Pts',(5.86319976261266,0.811287515665438,46.7249229546437));
#21757=CARTESIAN_POINT('Ctrl Pts',(5.83595356553042,0.974462181653458,46.732709536976));
#21758=CARTESIAN_POINT('Ctrl Pts',(5.80870632955674,1.13764306945519,46.740496416209));
#21759=CARTESIAN_POINT('Ctrl Pts',(5.77460910758077,1.29968986656213,46.748283295442));
#21760=CARTESIAN_POINT('Ctrl Pts',(5.73378262981295,1.46002305343281,46.7560701746749));
#21761=CARTESIAN_POINT('Ctrl Pts',(5.69295884656904,1.62034565840597,46.7638565399784));
#21762=CARTESIAN_POINT('Ctrl Pts',(5.64540677526719,1.7789545698254,46.7716429052819));
#21763=CARTESIAN_POINT('Ctrl Pts',(5.59129763801248,1.93528325721484,46.7794292705853));
#21764=CARTESIAN_POINT('Ctrl Pts',(5.53717429279703,2.09165299334327,46.7872176804302));
#21765=CARTESIAN_POINT('Ctrl Pts',(5.47649054395599,2.24574100624698,46.7950060902751));
#21766=CARTESIAN_POINT('Ctrl Pts',(5.40946690214381,2.39699778829907,46.80279450012));
#21767=CARTESIAN_POINT('Ctrl Pts',(5.34596548395855,2.5403057302543,46.8101736137758));
#21768=CARTESIAN_POINT('Ctrl Pts',(5.27677348696139,2.68107212328657,46.8175527274316));
#21769=CARTESIAN_POINT('Ctrl Pts',(5.20211766672,2.81884769792547,46.8249318410874));
#21770=CARTESIAN_POINT('Ctrl Pts',(5.12332394278771,2.96425967729436,46.8327199524816));
#21771=CARTESIAN_POINT('Ctrl Pts',(5.0384153994314,3.10639183003049,46.8405080638757));
#21772=CARTESIAN_POINT('Ctrl Pts',(4.94769014194066,3.24473308946102,46.8482961752698));
#21773=CARTESIAN_POINT('Ctrl Pts',(4.85698269677268,3.38304718799686,46.8560827576041));
#21774=CARTESIAN_POINT('Ctrl Pts',(4.76046099124113,3.51757161124834,46.8638693399383));
#21775=CARTESIAN_POINT('Ctrl Pts',(4.65846696926244,3.64782346869895,46.8716559222726));
#21776=CARTESIAN_POINT('Ctrl Pts',(4.55646905827439,3.77808029262389,46.8794428015074));
#21777=CARTESIAN_POINT('Ctrl Pts',(4.44899860719475,3.90406397076062,46.8872296807423));
#21778=CARTESIAN_POINT('Ctrl Pts',(4.33643889456204,4.02532337536123,46.8950165599772));
#21779=CARTESIAN_POINT('Ctrl Pts',(4.22388661080532,4.14657477691121,46.9028029252826));
#21780=CARTESIAN_POINT('Ctrl Pts',(4.10624595514678,4.26310229476014,46.9105892905879));
#21781=CARTESIAN_POINT('Ctrl Pts',(3.98393832978329,4.37449036425771,46.9183756558933));
#21782=CARTESIAN_POINT('Ctrl Pts',(3.86159858892146,4.48590768200002,46.92616406574));
#21783=CARTESIAN_POINT('Ctrl Pts',(3.73458966473574,4.59218263805356,46.9339524755868));
#21784=CARTESIAN_POINT('Ctrl Pts',(3.60336809649189,4.69293819730075,46.9417408854335));
#21785=CARTESIAN_POINT('Ctrl Pts',(3.47904247881391,4.78839885445902,46.9491199990799));
#21786=CARTESIAN_POINT('Ctrl Pts',(3.3509358006243,4.87890514593129,46.9564991127262));
#21787=CARTESIAN_POINT('Ctrl Pts',(3.21946212751893,4.96417104580123,46.9638782263726));
#21788=CARTESIAN_POINT('Ctrl Pts',(3.08070134129333,5.05416292801406,46.9716663377643));
#21789=CARTESIAN_POINT('Ctrl Pts',(2.93814017727367,5.13834917435367,46.979454449156));
#21790=CARTESIAN_POINT('Ctrl Pts',(2.79228492083751,5.21642362959178,46.9872425605476));
#21791=CARTESIAN_POINT('Ctrl Pts',(2.64645830053852,5.29448275627153,46.9950291428794));
#21792=CARTESIAN_POINT('Ctrl Pts',(2.49733915979091,5.36643233539255,47.0028157252111));
#21793=CARTESIAN_POINT('Ctrl Pts',(2.34545879920438,5.43201192779754,47.0106023075429));
#21794=CARTESIAN_POINT('Ctrl Pts',(2.19357264745324,5.49759402073791,47.0183891867753));
#21795=CARTESIAN_POINT('Ctrl Pts',(2.03892535696227,5.55680551066272,47.0261760660077));
#21796=CARTESIAN_POINT('Ctrl Pts',(1.88206932878776,5.60943362596764,47.0339629452402));
#21797=CARTESIAN_POINT('Ctrl Pts',(1.7252236530201,5.66205826784748,47.0417493105431));
#21798=CARTESIAN_POINT('Ctrl Pts',(1.56616983428111,5.70810030307102,47.049535675846));
#21799=CARTESIAN_POINT('Ctrl Pts',(1.40547673624174,5.74739642850424,47.0573220411489));
#21800=CARTESIAN_POINT('Ctrl Pts',(1.24474144345755,5.78670287230213,47.0651104509932));
#21801=CARTESIAN_POINT('Ctrl Pts',(1.08236632138698,5.81925978896817,47.0728988608376));
#21802=CARTESIAN_POINT('Ctrl Pts',(0.918932654476083,5.84495451984338,47.0806872706819));
#21803=CARTESIAN_POINT('Ctrl Pts',(0.764087746737819,5.869298942305,47.0880663843405));
#21804=CARTESIAN_POINT('Ctrl Pts',(0.60829294670612,5.88748383046348,47.0954454979991));
#21805=CARTESIAN_POINT('Ctrl Pts',(0.452048699719725,5.89945612201512,47.1028246116577));
#21806=CARTESIAN_POINT('Ctrl Pts',(0.287144395986138,5.91209199463443,47.1106127230507));
#21807=CARTESIAN_POINT('Ctrl Pts',(0.121680514692252,5.91781157111677,47.1184008344436));
#21808=CARTESIAN_POINT('Ctrl Pts',(-0.0437518879576071,5.91658823434588,
47.1261889458366));
#21809=CARTESIAN_POINT('Ctrl Pts',(-0.209151810839005,5.91536513775584,
47.1339755281696));
#21810=CARTESIAN_POINT('Ctrl Pts',(-0.374519948085462,5.90720185010354,
47.1417621105027));
#21811=CARTESIAN_POINT('Ctrl Pts',(-0.539265149226785,5.89212386676735,
47.1495486928358));
#21812=CARTESIAN_POINT('Ctrl Pts',(-0.704016632065692,5.87704530851104,
47.1573355720695));
#21813=CARTESIAN_POINT('Ctrl Pts',(-0.868144812725076,5.85505155218487,
47.1651224513032));
#21814=CARTESIAN_POINT('Ctrl Pts',(-1.03106281778922,5.82622004633129,47.1729093305369));
#21815=CARTESIAN_POINT('Ctrl Pts',(-1.19397007035901,5.79739044334046,47.180695695841));
#21816=CARTESIAN_POINT('Ctrl Pts',(-1.35566699252405,5.76172404971993,47.1884820611452));
#21817=CARTESIAN_POINT('Ctrl Pts',(-1.51557592213154,5.71934962970049,47.1962684264494));
#21818=CARTESIAN_POINT('Ctrl Pts',(-1.67552684057655,5.67696408301889,47.2040568362949));
#21819=CARTESIAN_POINT('Ctrl Pts',(-1.83368851875553,5.62786707033558,47.2118452461405));
#21820=CARTESIAN_POINT('Ctrl Pts',(-1.98949661765231,5.57223777048773,47.219633655986));
#21821=CARTESIAN_POINT('Ctrl Pts',(-2.13711669575537,5.51953189931348,47.2270127696383));
#21822=CARTESIAN_POINT('Ctrl Pts',(-2.28262395754884,5.46096273850716,47.2343918832905));
#21823=CARTESIAN_POINT('Ctrl Pts',(-2.42555356368133,5.3967231235457,47.2417709969428));
#21824=CARTESIAN_POINT('Ctrl Pts',(-2.5764052441222,5.32892293763579,47.2495591083406));
#21825=CARTESIAN_POINT('Ctrl Pts',(-2.72443930242105,5.25478167256802,47.2573472197384));
#21826=CARTESIAN_POINT('Ctrl Pts',(-2.86912398406555,5.17455873737654,47.2651353311363));
#21827=CARTESIAN_POINT('Ctrl Pts',(-3.01378025939573,5.09435155255949,47.2729219134742));
#21828=CARTESIAN_POINT('Ctrl Pts',(-3.15508819088794,5.00806523491198,47.2807084958122));
#21829=CARTESIAN_POINT('Ctrl Pts',(-3.29254087370797,4.91600499973936,47.2884950781501));
#21830=CARTESIAN_POINT('Ctrl Pts',(-3.42999879756825,4.82394125433043,47.2962819573887));
#21831=CARTESIAN_POINT('Ctrl Pts',(-3.56360091093889,4.72610332538268,47.3040688366274));
#21832=CARTESIAN_POINT('Ctrl Pts',(-3.69286892099062,4.62284000316706,47.311855715866));
#21833=CARTESIAN_POINT('Ctrl Pts',(-3.82212839942829,4.5195834962711,47.319642081175));
#21834=CARTESIAN_POINT('Ctrl Pts',(-3.94705409737575,4.41090251220354,47.3274284464841));
#21835=CARTESIAN_POINT('Ctrl Pts',(-4.06720036185885,4.29718649571964,47.3352148117932));
#21836=CARTESIAN_POINT('Ctrl Pts',(-4.18737817431023,4.18344061971995,47.3430032216436));
#21837=CARTESIAN_POINT('Ctrl Pts',(-4.30277381202874,4.06465728785799,47.350791631494));
#21838=CARTESIAN_POINT('Ctrl Pts',(-4.41297744151611,3.94126384084724,47.3585800413444));
#21839=CARTESIAN_POINT('Ctrl Pts',(-4.51738965399641,3.82435496163977,47.3659591549723));
#21840=CARTESIAN_POINT('Ctrl Pts',(-4.61714134975592,3.70330823982444,47.3733382686001));
#21841=CARTESIAN_POINT('Ctrl Pts',(-4.71191660204499,3.57851540416871,47.3807173822279));
#21842=CARTESIAN_POINT('Ctrl Pts',(-4.81194490595416,3.44680575012756,47.3885054936042));
#21843=CARTESIAN_POINT('Ctrl Pts',(-4.90646519569752,3.31087589954584,47.3962936049805));
#21844=CARTESIAN_POINT('Ctrl Pts',(-4.99513463593049,3.17120805552515,47.4040817163568));
#21845=CARTESIAN_POINT('Ctrl Pts',(-5.08378666746387,3.03156763285201,47.4118682986732));
#21846=CARTESIAN_POINT('Ctrl Pts',(-5.1665899703572,2.88819095065933,47.4196548809895));
#21847=CARTESIAN_POINT('Ctrl Pts',(-5.24324544567091,2.74158854661878,47.4274414633059));
#21848=CARTESIAN_POINT('Ctrl Pts',(-5.31990384384115,2.59498055266058,47.4352283425229));
#21849=CARTESIAN_POINT('Ctrl Pts',(-5.39041379381665,2.44514687205506,47.4430152217399));
#21850=CARTESIAN_POINT('Ctrl Pts',(-5.45452216931258,2.29262261765377,47.4508021009569));
#21851=CARTESIAN_POINT('Ctrl Pts',(-5.51862631369322,2.14010842976407,47.4585884662445));
#21852=CARTESIAN_POINT('Ctrl Pts',(-5.57632960537021,1.98490431807098,47.466374831532));
#21853=CARTESIAN_POINT('Ctrl Pts',(-5.62742703039951,1.82756547899902,47.4741611968196));
#21854=CARTESIAN_POINT('Ctrl Pts',(-5.67853787257673,1.67018532593765,47.4819496066488));
#21855=CARTESIAN_POINT('Ctrl Pts',(-5.72303928147326,1.51066962893358,47.489738016478));
#21856=CARTESIAN_POINT('Ctrl Pts',(-5.76077582780725,1.34958972441691,47.4975264263072));
#21857=CARTESIAN_POINT('Ctrl Pts',(-5.79652924519047,1.19697488236795,47.5049055400425));
#21858=CARTESIAN_POINT('Ctrl Pts',(-5.82621046646223,1.04295626177493,47.5122846537778));
#21859=CARTESIAN_POINT('Ctrl Pts',(-5.84972948598496,0.888028999131292,
47.5196637675131));
#21860=CARTESIAN_POINT('Ctrl Pts',(-5.87556177675534,0.717863482962543,
47.5277686722033));
#21861=CARTESIAN_POINT('Ctrl Pts',(-5.89396637127144,0.546559387938223,
47.5358735768934));
#21862=CARTESIAN_POINT('Ctrl Pts',(-5.90487006217366,0.374753400712039,
47.5439784815836));
#21863=CARTESIAN_POINT('Ctrl Pts',(-5.91278338067241,0.250065759700836,
47.5498605900174));
#21864=CARTESIAN_POINT('Ctrl Pts',(-5.91674697913699,0.125113954375808,
47.5557426984511));
#21865=CARTESIAN_POINT('Ctrl Pts',(-5.91674999827337,0.000142940948123385,
47.5616248068849));
#21866=CARTESIAN_POINT('Origin',(0.,0.,-3.23514056400928));
#21867=CARTESIAN_POINT('',(-4.76403455895385,1.22194835553447,1.41535621473006));
#21868=CARTESIAN_POINT('',(-4.76403458704967,1.22194824599671,1.06992377601457));
#21869=CARTESIAN_POINT('',(-4.76403458704967,1.22194824599672,-3.23514056400928));
#21870=CARTESIAN_POINT('',(-2.8553491342286,-4.00451799648347,2.16840434497101E-18));
#21871=CARTESIAN_POINT('Ctrl Pts',(-4.76403455895385,1.22194835553447,1.41535621473006));
#21872=CARTESIAN_POINT('Ctrl Pts',(-4.70800458999606,1.44039351914803,1.40248102012867));
#21873=CARTESIAN_POINT('Ctrl Pts',(-4.63700314305273,1.65477845756619,1.38953413322633));
#21874=CARTESIAN_POINT('Ctrl Pts',(-4.53470696246686,1.90462138753004,1.37415813085186));
#21875=CARTESIAN_POINT('Ctrl Pts',(-4.51734827967389,1.94543425658411,1.37163740433799));
#21876=CARTESIAN_POINT('Ctrl Pts',(-4.48332579221817,2.02251461500581,1.36686209249771));
#21877=CARTESIAN_POINT('Ctrl Pts',(-4.46676799018909,2.05882473359429,1.36460659436931));
#21878=CARTESIAN_POINT('Ctrl Pts',(-4.39436976654198,2.21260337620139,1.35501920397534));
#21879=CARTESIAN_POINT('Ctrl Pts',(-4.33432290960145,2.32803458784841,1.34773327110701));
#21880=CARTESIAN_POINT('Ctrl Pts',(-4.18113760089329,2.59599006489001,1.33044134998623));
#21881=CARTESIAN_POINT('Ctrl Pts',(-4.08412679119583,2.74608509668859,1.32044467337898));
#21882=CARTESIAN_POINT('Ctrl Pts',(-3.94196421486327,2.94178662712893,1.3068095633645));
#21883=CARTESIAN_POINT('Ctrl Pts',(-3.90377401407975,2.99227986154057,1.30323425584314));
#21884=CARTESIAN_POINT('Ctrl Pts',(-3.82025735868806,3.09838040828677,1.29559038274552));
#21885=CARTESIAN_POINT('Ctrl Pts',(-3.77466746673069,3.15376168985781,1.29152035466386));
#21886=CARTESIAN_POINT('Ctrl Pts',(-3.61460481143815,3.33975654501333,1.27756165950139));
#21887=CARTESIAN_POINT('Ctrl Pts',(-3.49443546192976,3.46529380119033,1.26762995378764));
#21888=CARTESIAN_POINT('Ctrl Pts',(-3.28103729949359,3.66581203918653,1.25086736292124));
#21889=CARTESIAN_POINT('Ctrl Pts',(-3.1912562490297,3.74423125195052,1.24404822497318));
#21890=CARTESIAN_POINT('Ctrl Pts',(-3.06518498035832,3.84651640082668,1.23480436463534));
#21891=CARTESIAN_POINT('Ctrl Pts',(-3.03129780311374,3.87327782015248,1.23235080372801));
#21892=CARTESIAN_POINT('Ctrl Pts',(-2.96477228891903,3.92440656182911,1.22759642534413));
#21893=CARTESIAN_POINT('Ctrl Pts',(-2.9321749923349,3.94882152596272,1.22529519661884));
#21894=CARTESIAN_POINT('Ctrl Pts',(-2.79208576872101,4.05105537801711,1.21551518142562));
#21895=CARTESIAN_POINT('Ctrl Pts',(-2.68177020542182,4.12491235949855,1.20808331305876));
#21896=CARTESIAN_POINT('Ctrl Pts',(-2.45204274421959,4.2656008941963,1.19299175042516));
#21897=CARTESIAN_POINT('Ctrl Pts',(-2.33255928461634,4.33209318646586,1.18533827960573));
#21898=CARTESIAN_POINT('Ctrl Pts',(-2.13833567289214,4.42981069090453,1.17310919377991));
#21899=CARTESIAN_POINT('Ctrl Pts',(-2.06532668337509,4.46431715818869,1.16855816212231));
#21900=CARTESIAN_POINT('Ctrl Pts',(-1.92938341482113,4.52451966249412,1.16015281534676));
#21901=CARTESIAN_POINT('Ctrl Pts',(-1.86670200509481,4.55073862400259,1.15630340995557));
#21902=CARTESIAN_POINT('Ctrl Pts',(-1.7025417419909,4.6154425868246,1.1462812007209));
#21903=CARTESIAN_POINT('Ctrl Pts',(-1.60029717189643,4.65188210785799,1.14009623174922));
#21904=CARTESIAN_POINT('Ctrl Pts',(-1.41032909081309,4.71258111216489,1.12869998971155));
#21905=CARTESIAN_POINT('Ctrl Pts',(-1.3229755827362,4.73784596503927,1.12349580990551));
#21906=CARTESIAN_POINT('Ctrl Pts',(-1.11494925858713,4.79181032440926,1.1111934385348));
#21907=CARTESIAN_POINT('Ctrl Pts',(-0.993790475945812,4.81839590232615,
1.10409881184008));
#21908=CARTESIAN_POINT('Ctrl Pts',(-0.832058031315079,4.84752406127705,
1.09474836862278));
#21909=CARTESIAN_POINT('Ctrl Pts',(-0.79227343934583,4.85418509642126,1.09245790434709));
#21910=CARTESIAN_POINT('Ctrl Pts',(-0.70921897981244,4.86704240413971,1.08769850294539));
#21911=CARTESIAN_POINT('Ctrl Pts',(-0.665939352632694,4.8731527950463,1.08523061740399));
#21912=CARTESIAN_POINT('Ctrl Pts',(-0.569007689189142,4.88552253571552,
1.07972410819372));
#21913=CARTESIAN_POINT('Ctrl Pts',(-0.515322334762011,4.89147658294237,
1.07668845170441));
#21914=CARTESIAN_POINT('Ctrl Pts',(-0.324104999640068,4.90950077418687,
1.06590772639198));
#21915=CARTESIAN_POINT('Ctrl Pts',(-0.18617567718527,4.91666357473129,1.05818794873214));
#21916=CARTESIAN_POINT('Ctrl Pts',(0.0696233275322052,4.91916683216118,
1.04384335123138));
#21917=CARTESIAN_POINT('Ctrl Pts',(0.187376707626406,4.91608982794185,1.03722941185142));
#21918=CARTESIAN_POINT('Ctrl Pts',(0.373250962939735,4.90454442225307,1.02672394956429));
#21919=CARTESIAN_POINT('Ctrl Pts',(0.441500390548411,4.89887227198899,1.02285279364985));
#21920=CARTESIAN_POINT('Ctrl Pts',(0.587500701242777,4.88366245920214,1.01453356174002));
#21921=CARTESIAN_POINT('Ctrl Pts',(0.665187208179159,4.8736887328254,1.01008363000141));
#21922=CARTESIAN_POINT('Ctrl Pts',(0.832459861589463,4.8481394882327,1.00044440941763));
#21923=CARTESIAN_POINT('Ctrl Pts',(0.921919570274004,4.83192611678681,0.995252988755495));
#21924=CARTESIAN_POINT('Ctrl Pts',(1.16936495129481,4.77995761069626,0.980790344560267));
#21925=CARTESIAN_POINT('Ctrl Pts',(1.32611175780708,4.73886453699499,0.971507779099062));
#21926=CARTESIAN_POINT('Ctrl Pts',(1.52923323236656,4.6747444305644,0.959362192624918));
#21927=CARTESIAN_POINT('Ctrl Pts',(1.57767903108842,4.65861768445817,0.956456788706344));
#21928=CARTESIAN_POINT('Ctrl Pts',(1.65758129799825,4.6306302617227,0.951653830300278));
#21929=CARTESIAN_POINT('Ctrl Pts',(1.68918250879534,4.6191963428178,0.949751679951918));
#21930=CARTESIAN_POINT('Ctrl Pts',(1.78387064679191,4.58383472440289,0.944041783846336));
#21931=CARTESIAN_POINT('Ctrl Pts',(1.84658506085465,4.55893178806036,0.940245321199586));
#21932=CARTESIAN_POINT('Ctrl Pts',(2.01218282940812,4.48919753266307,0.93015388892282));
#21933=CARTESIAN_POINT('Ctrl Pts',(2.11407766251384,4.44212224904136,0.923873921626289));
#21934=CARTESIAN_POINT('Ctrl Pts',(2.34194827429732,4.32722847802811,0.909575184603036));
#21935=CARTESIAN_POINT('Ctrl Pts',(2.4667538503199,4.2573175520126,0.901557789427352));
#21936=CARTESIAN_POINT('Ctrl Pts',(2.64212712942223,4.14877684306496,0.889931669827502));
#21937=CARTESIAN_POINT('Ctrl Pts',(2.69527157592141,4.11444966985275,0.886358710261123));
#21938=CARTESIAN_POINT('Ctrl Pts',(2.80726530176578,4.03900926546058,0.878714432627161));
#21939=CARTESIAN_POINT('Ctrl Pts',(2.86590656927715,3.99761350015156,0.874641627471378));
#21940=CARTESIAN_POINT('Ctrl Pts',(2.95578878974989,3.93116979732131,0.868283265482476));
#21941=CARTESIAN_POINT('Ctrl Pts',(2.98766568027562,3.90699847750105,0.866004827442259));
#21942=CARTESIAN_POINT('Ctrl Pts',(3.1648082201486,3.76924067396294,0.853209122484264));
#21943=CARTESIAN_POINT('Ctrl Pts',(3.30389020817152,3.6479439271942,0.84264291284247));
#21944=CARTESIAN_POINT('Ctrl Pts',(3.49264722396826,3.46365466272917,0.827556885825742));
#21945=CARTESIAN_POINT('Ctrl Pts',(3.54811236656066,3.4068148032227,0.823023055605946));
#21946=CARTESIAN_POINT('Ctrl Pts',(3.62627891112114,3.32273040893692,0.816493249232355));
#21947=CARTESIAN_POINT('Ctrl Pts',(3.65009999875253,3.29654457727735,0.814483556612904));
#21948=CARTESIAN_POINT('Ctrl Pts',(3.70214958748059,3.23807203690915,0.810049707746506));
#21949=CARTESIAN_POINT('Ctrl Pts',(3.73024274954224,3.20566859974127,0.807627819375163));
#21950=CARTESIAN_POINT('Ctrl Pts',(3.77538619953825,3.15220177867906,0.803683841414471));
#21951=CARTESIAN_POINT('Ctrl Pts',(3.79269239028166,3.13135776501974,0.802158917798039));
#21952=CARTESIAN_POINT('Ctrl Pts',(3.86066637610091,3.04809793389413,0.796114856427663));
#21953=CARTESIAN_POINT('Ctrl Pts',(3.90997302083059,2.98458657226352,0.791608110070563));
#21954=CARTESIAN_POINT('Ctrl Pts',(4.02309178955499,2.83126247167256,0.780931632574437));
#21955=CARTESIAN_POINT('Ctrl Pts',(4.08548662973932,2.74045865314341,0.774766370665049));
#21956=CARTESIAN_POINT('Ctrl Pts',(4.20013243126663,2.56098479366827,0.762814316050396));
#21957=CARTESIAN_POINT('Ctrl Pts',(4.25275332125629,2.47261892936278,0.757032639913442));
#21958=CARTESIAN_POINT('Ctrl Pts',(4.33532968791823,2.32350458598782,0.747411870026766));
#21959=CARTESIAN_POINT('Ctrl Pts',(4.36686990759476,2.26367050146169,0.743586333707472));
#21960=CARTESIAN_POINT('Ctrl Pts',(4.43432676579941,2.1290398462895,0.735047442657509));
#21961=CARTESIAN_POINT('Ctrl Pts',(4.46960488461165,2.05394656017347,0.730330602418138));
#21962=CARTESIAN_POINT('Ctrl Pts',(4.54363744908731,1.88540937436285,0.719836914730252));
#21963=CARTESIAN_POINT('Ctrl Pts',(4.58144269902896,1.79158932299904,0.71405651546578));
#21964=CARTESIAN_POINT('Ctrl Pts',(4.67356443828738,1.54094312972681,0.698774043179428));
#21965=CARTESIAN_POINT('Ctrl Pts',(4.72288402861999,1.38241729777547,0.689267197930461));
#21966=CARTESIAN_POINT('Ctrl Pts',(4.77299690510432,1.1869991856083,0.677790897478523));
#21967=CARTESIAN_POINT('Ctrl Pts',(4.78151662810783,1.15220019699886,0.675756637819336));
#21968=CARTESIAN_POINT('Ctrl Pts',(4.79922305390596,1.07629681946347,0.67134147583945));
#21969=CARTESIAN_POINT('Ctrl Pts',(4.80826354195133,1.03516111357796,0.668962561024106));
#21970=CARTESIAN_POINT('Ctrl Pts',(4.82709104058373,0.94391799637511,0.663710637263908));
#21971=CARTESIAN_POINT('Ctrl Pts',(4.83662847959172,0.893764014389616,0.660840171746807));
#21972=CARTESIAN_POINT('Ctrl Pts',(4.8659840072216,0.725128821764615,0.651228679364703));
#21973=CARTESIAN_POINT('Ctrl Pts',(4.88224223726022,0.606071875210853,0.644507959084496));
#21974=CARTESIAN_POINT('Ctrl Pts',(4.8989175476528,0.438333912222894,0.635061534370354));
#21975=CARTESIAN_POINT('Ctrl Pts',(4.90299727991083,0.390060776575174,0.632345676530746));
#21976=CARTESIAN_POINT('Ctrl Pts',(4.91350445818342,0.239207114951488,0.623858992564783));
#21977=CARTESIAN_POINT('Ctrl Pts',(4.91743008254092,0.136481191992652,0.618079906910746));
#21978=CARTESIAN_POINT('Ctrl Pts',(4.91859788618268,-0.0339022982125286,
0.608462805207919));
#21979=CARTESIAN_POINT('Ctrl Pts',(4.91766703455457,-0.101515191490959,
0.604638334234605));
#21980=CARTESIAN_POINT('Ctrl Pts',(4.91249170121569,-0.251961745133505,
0.596102261461636));
#21981=CARTESIAN_POINT('Ctrl Pts',(4.90754534292472,-0.334750513753387,
0.591387176854443));
#21982=CARTESIAN_POINT('Ctrl Pts',(4.89193099862737,-0.518083088487674,
0.580898301712649));
#21983=CARTESIAN_POINT('Ctrl Pts',(4.8802512632039,-0.618503289527568,0.575120963629649));
#21984=CARTESIAN_POINT('Ctrl Pts',(4.84122182036858,-0.882803168354224,
0.559831221571236));
#21985=CARTESIAN_POINT('Ctrl Pts',(4.80864971356233,-1.04578149136887,0.550313978955285));
#21986=CARTESIAN_POINT('Ctrl Pts',(4.75911102118852,-1.24150179945074,0.538829159195305));
#21987=CARTESIAN_POINT('Ctrl Pts',(4.74994898948943,-1.27610699534426,0.536796572194886));
#21988=CARTESIAN_POINT('Ctrl Pts',(4.72917785234302,-1.35123518461451,0.532381129816443));
#21989=CARTESIAN_POINT('Ctrl Pts',(4.7174238988848,-1.39171530736654,0.530000275641919));
#21990=CARTESIAN_POINT('Ctrl Pts',(4.69026905621618,-1.48093604635368,0.524742963330227));
#21991=CARTESIAN_POINT('Ctrl Pts',(4.67462575583941,-1.52959782333168,0.521869056859459));
#21992=CARTESIAN_POINT('Ctrl Pts',(4.61958074967787,-1.6920889190974,0.512235723518684));
#21993=CARTESIAN_POINT('Ctrl Pts',(4.57675681652586,-1.80471284968568,0.505496692101554));
#21994=CARTESIAN_POINT('Ctrl Pts',(4.4784101881611,-2.03726804454011,0.491346642355479));
#21995=CARTESIAN_POINT('Ctrl Pts',(4.42210257272034,-2.15676311186973,0.483938811092049));
#21996=CARTESIAN_POINT('Ctrl Pts',(4.33187517835345,-2.32981204292907,0.472936981507766));
#21997=CARTESIAN_POINT('Ctrl Pts',(4.30162036882072,-2.38521043338096,0.469372014032746));
#21998=CARTESIAN_POINT('Ctrl Pts',(4.25129151571578,-2.47329188882621,0.463628789000986));
#21999=CARTESIAN_POINT('Ctrl Pts',(4.23188670723431,-2.50634937533143,0.461455933981613));
#22000=CARTESIAN_POINT('Ctrl Pts',(4.1661067037804,-2.61546813496452,0.454223616716428));
#22001=CARTESIAN_POINT('Ctrl Pts',(4.11805203383028,-2.69049545619224,0.449152393739429));
#22002=CARTESIAN_POINT('Ctrl Pts',(3.9976919724941,-2.86762716283573,0.436930591734692));
#22003=CARTESIAN_POINT('Ctrl Pts',(3.92347685323226,-2.96835909051039,0.429771484919504));
#22004=CARTESIAN_POINT('Ctrl Pts',(3.77446042501811,-3.15525238391744,0.416089089147852));
#22005=CARTESIAN_POINT('Ctrl Pts',(3.70034154221736,-3.2418578022171,0.409570143745308));
#22006=CARTESIAN_POINT('Ctrl Pts',(3.59486287702776,-3.3567707773681,0.400690987727624));
#22007=CARTESIAN_POINT('Ctrl Pts',(3.56604898498235,-3.38736532533066,0.398303584216129));
#22008=CARTESIAN_POINT('Ctrl Pts',(3.52758504865158,-3.4271714896889,0.395167716502782));
#22009=CARTESIAN_POINT('Ctrl Pts',(3.51828483542188,-3.43671827677309,0.39441334647493));
#22010=CARTESIAN_POINT('Ctrl Pts',(3.50720905887663,-3.44799562411524,0.393519403773952));
#22011=CARTESIAN_POINT('Ctrl Pts',(3.50547087311366,-3.4497627692854,0.393379241384583));
#22012=CARTESIAN_POINT('Ctrl Pts',(3.50154773318927,-3.45374524486064,0.39306318043343));
#22013=CARTESIAN_POINT('Ctrl Pts',(3.49936201069401,-3.45595981781253,0.392887293943682));
#22014=CARTESIAN_POINT('Ctrl Pts',(3.49529564620845,-3.46007204346587,0.392560444902864));
#22015=CARTESIAN_POINT('Ctrl Pts',(3.4934155570471,-3.46197024050948,0.392409473979546));
#22016=CARTESIAN_POINT('Ctrl Pts',(3.4898060579431,-3.46560856984013,0.392119914366113));
#22017=CARTESIAN_POINT('Ctrl Pts',(3.48807689098957,-3.46734894176531,0.391981322084046));
#22018=CARTESIAN_POINT('Ctrl Pts',(3.48467787356313,-3.4707648689987,0.391709134410787));
#22019=CARTESIAN_POINT('Ctrl Pts',(3.48300811507393,-3.47244051478418,0.391575537707908));
#22020=CARTESIAN_POINT('Ctrl Pts',(3.4796623408941,-3.47579324435343,0.391308072399589));
#22021=CARTESIAN_POINT('Ctrl Pts',(3.47798632009024,-3.47747032214568,0.391174203910555));
#22022=CARTESIAN_POINT('Ctrl Pts',(3.47457233874385,-3.48088151952984,0.390901751935026));
#22023=CARTESIAN_POINT('Ctrl Pts',(3.47283429109789,-3.4826155510985,0.390763169734242));
#22024=CARTESIAN_POINT('Ctrl Pts',(3.4692417279892,-3.48619444925671,0.390476970149689));
#22025=CARTESIAN_POINT('Ctrl Pts',(3.46738703753967,-3.48803913928207,0.390329355266043));
#22026=CARTESIAN_POINT('Ctrl Pts',(3.46350156233611,-3.49189750266945,0.390020397528303));
#22027=CARTESIAN_POINT('Ctrl Pts',(3.46147049097223,-3.49391088632748,0.389859058671085));
#22028=CARTESIAN_POINT('Ctrl Pts',(3.45716175431413,-3.4981746552999,0.389517138197447));
#22029=CARTESIAN_POINT('Ctrl Pts',(3.45488364502583,-3.50042459050742,0.389336562628139));
#22030=CARTESIAN_POINT('Ctrl Pts',(3.44999300849109,-3.50524531782098,0.388949338658751));
#22031=CARTESIAN_POINT('Ctrl Pts',(3.4473798009595,-3.50781541770806,0.388742699290535));
#22032=CARTESIAN_POINT('Ctrl Pts',(3.44170577658994,-3.51338337868411,0.388294597423941));
#22033=CARTESIAN_POINT('Ctrl Pts',(3.4386439100999,-3.51638016684864,0.388053148464375));
#22034=CARTESIAN_POINT('Ctrl Pts',(3.39615462748598,-3.55785779711908,0.384707521223595));
#22035=CARTESIAN_POINT('Ctrl Pts',(3.35608700325326,-3.59567774704789,0.381611414952683));
#22036=CARTESIAN_POINT('Ctrl Pts',(3.20803239819903,-3.730795788619,0.370361704603109));
#22037=CARTESIAN_POINT('Ctrl Pts',(3.09638189732583,-3.82396762409812,0.362235442278122));
#22038=CARTESIAN_POINT('Ctrl Pts',(2.89234687366823,-3.97943089669666,0.347846628514966));
#22039=CARTESIAN_POINT('Ctrl Pts',(2.8016665598546,-4.04378594179957,0.341599942079325));
#22040=CARTESIAN_POINT('Ctrl Pts',(2.66451101283828,-4.13429444620673,0.332328067910208));
#22041=CARTESIAN_POINT('Ctrl Pts',(2.61966587564448,-4.1628548065556,0.329323306095288));
#22042=CARTESIAN_POINT('Ctrl Pts',(2.51655861475035,-4.22619435072219,0.322470893460467));
#22043=CARTESIAN_POINT('Ctrl Pts',(2.45802225513673,-4.26050612127827,0.318620301091709));
#22044=CARTESIAN_POINT('Ctrl Pts',(2.33119038067773,-4.33136600754815,0.310355522240256));
#22045=CARTESIAN_POINT('Ctrl Pts',(2.26270331285743,-4.36753404505853,0.305939760305673));
#22046=CARTESIAN_POINT('Ctrl Pts',(2.04696815636872,-4.47502703512429,0.292170303537145));
#22047=CARTESIAN_POINT('Ctrl Pts',(1.89699652614637,-4.54063316588837,0.282793734797807));
#22048=CARTESIAN_POINT('Ctrl Pts',(1.67696400021694,-4.62408049431107,0.269346058299386));
#22049=CARTESIAN_POINT('Ctrl Pts',(1.6093434487895,-4.64804717326741,0.265254487534897));
#22050=CARTESIAN_POINT('Ctrl Pts',(1.50912331455892,-4.68111871561968,0.25925777296061));
#22051=CARTESIAN_POINT('Ctrl Pts',(1.47691570451368,-4.6913799305283,0.257340843342974));
#22052=CARTESIAN_POINT('Ctrl Pts',(1.40993169889658,-4.71196258281475,0.253375818361156));
#22053=CARTESIAN_POINT('Ctrl Pts',(1.37514185940846,-4.72223291226185,0.251328168260566));
#22054=CARTESIAN_POINT('Ctrl Pts',(1.32431137831679,-4.73662923991965,0.248350921459366));
#22055=CARTESIAN_POINT('Ctrl Pts',(1.30835865813774,-4.74106051505588,0.247418608939291));
#22056=CARTESIAN_POINT('Ctrl Pts',(1.22630414057961,-4.76340756320277,0.242632996103116));
#22057=CARTESIAN_POINT('Ctrl Pts',(1.15985534548363,-4.78002187760958,0.238790169932708));
#22058=CARTESIAN_POINT('Ctrl Pts',(0.876893333134046,-4.84452337805585,
0.222520662097336));
#22059=CARTESIAN_POINT('Ctrl Pts',(0.657622635982413,-4.87912696044817,
0.210134065576976));
#22060=CARTESIAN_POINT('Ctrl Pts',(0.36920778394442,-4.90484142278869,0.193805420862475));
#22061=CARTESIAN_POINT('Ctrl Pts',(0.301530401692974,-4.90946667701105,
0.189972417139949));
#22062=CARTESIAN_POINT('Ctrl Pts',(0.22249308080866,-4.91322781521364,0.185489744185811));
#22063=CARTESIAN_POINT('Ctrl Pts',(0.211204815300942,-4.91372600584816,
0.184849374109209));
#22064=CARTESIAN_POINT('Ctrl Pts',(0.184504539836169,-4.9148122050559,0.183334320200665));
#22065=CARTESIAN_POINT('Ctrl Pts',(0.169091294900664,-4.91536662605794,
0.182459427987104));
#22066=CARTESIAN_POINT('Ctrl Pts',(0.0616604243043279,-4.91872505271733,
0.176359092274275));
#22067=CARTESIAN_POINT('Ctrl Pts',(-0.0304166115604183,-4.91901744999519,
0.17111840040058));
#22068=CARTESIAN_POINT('Ctrl Pts',(-0.249210191133736,-4.91356859160635,
0.158627210766751));
#22069=CARTESIAN_POINT('Ctrl Pts',(-0.375803584891369,-4.90551050793662,
0.151368589394854));
#22070=CARTESIAN_POINT('Ctrl Pts',(-0.61074667165503,-4.88140701142047,
0.137849933703064));
#22071=CARTESIAN_POINT('Ctrl Pts',(-0.719148645031559,-4.86661807870668,
0.131593773414491));
#22072=CARTESIAN_POINT('Ctrl Pts',(-0.868949575330054,-4.8410663525139,
0.12294221769599));
#22073=CARTESIAN_POINT('Ctrl Pts',(-0.910836712257016,-4.83336045969209,
0.120522507688562));
#22074=CARTESIAN_POINT('Ctrl Pts',(-0.991361723899217,-4.81746245629585,
0.115872036592666));
#22075=CARTESIAN_POINT('Ctrl Pts',(-1.03001141151743,-4.80934705763011,
0.113640555909532));
#22076=CARTESIAN_POINT('Ctrl Pts',(-1.28868875145496,-4.75177040217614,
0.0986950052671175));
#22077=CARTESIAN_POINT('Ctrl Pts',(-1.50518972358113,-4.68769099446982,
0.0861225413595998));
#22078=CARTESIAN_POINT('Ctrl Pts',(-1.81125436013622,-4.57370287505729,
0.0677891040393032));
#22079=CARTESIAN_POINT('Ctrl Pts',(-1.90486781891452,-4.53551304514553,
0.0621040996125177));
#22080=CARTESIAN_POINT('Ctrl Pts',(-2.05706093635756,-4.46788193455122,
0.0527025580373686));
#22081=CARTESIAN_POINT('Ctrl Pts',(-2.11634755714247,-4.44010603164832,
0.0489992994415321));
#22082=CARTESIAN_POINT('Ctrl Pts',(-2.23227254641777,-4.38294549566522,
0.041670234120012));
#22083=CARTESIAN_POINT('Ctrl Pts',(-2.28892885677717,-4.35362567505692,
0.0380455713974877));
#22084=CARTESIAN_POINT('Ctrl Pts',(-2.52146244390851,-4.22749472134931,
0.0229824627520859));
#22085=CARTESIAN_POINT('Ctrl Pts',(-2.69189827355834,-4.12106367661615,
0.0114832924308145));
#22086=CARTESIAN_POINT('Ctrl Pts',(-2.8553491342286,-4.00451799648347,2.16840434497101E-18));
#22087=CARTESIAN_POINT('',(2.85706463458462,-4.00329423553975,0.));
#22088=CARTESIAN_POINT('Origin',(0.,0.,0.));
#22089=CARTESIAN_POINT('Ctrl Pts',(2.85706463458456,-4.0032942355398,0.));
#22090=CARTESIAN_POINT('Ctrl Pts',(2.97498500626953,-3.91913701305856,0.00820407285754789));
#22091=CARTESIAN_POINT('Ctrl Pts',(3.08919334481163,-3.82975975962187,0.0164081457150967));
#22092=CARTESIAN_POINT('Ctrl Pts',(3.19923812022538,-3.73551315251289,0.0246122185726447));
#22093=CARTESIAN_POINT('Ctrl Pts',(3.30927402805244,-3.64127413994854,0.0328156303326808));
#22094=CARTESIAN_POINT('Ctrl Pts',(3.41514679505572,-3.54216676932236,0.0410190420927171));
#22095=CARTESIAN_POINT('Ctrl Pts',(3.51643872130203,-3.43858136181591,0.0492224538527535));
#22096=CARTESIAN_POINT('Ctrl Pts',(3.61774645859056,-3.33497978526902,0.0574271461145484));
#22097=CARTESIAN_POINT('Ctrl Pts',(3.71447169625567,-3.22689900641972,0.0656318383763429));
#22098=CARTESIAN_POINT('Ctrl Pts',(3.80623385628371,-3.11476594526452,0.0738365306381379));
#22099=CARTESIAN_POINT('Ctrl Pts',(3.89799542774863,-3.00263360333156,0.0820411702749799));
#22100=CARTESIAN_POINT('Ctrl Pts',(3.98479378129704,-2.88644928568954,0.0902458099118233));
#22101=CARTESIAN_POINT('Ctrl Pts',(4.06628890577333,-2.76667265813734,0.0984504495486656));
#22102=CARTESIAN_POINT('Ctrl Pts',(4.14780581620183,-2.64686401090421,0.106657282517786));
#22103=CARTESIAN_POINT('Ctrl Pts',(4.22401648141588,-2.52346140481058,0.114864115486905));
#22104=CARTESIAN_POINT('Ctrl Pts',(4.29462408636437,-2.39695369569772,0.123070948456026));
#22105=CARTESIAN_POINT('Ctrl Pts',(4.34036337126301,-2.31500257792212,0.12838729747486));
#22106=CARTESIAN_POINT('Ctrl Pts',(4.38375228545424,-2.23174901418395,0.133703646493694));
#22107=CARTESIAN_POINT('Ctrl Pts',(4.42472038127204,-2.14733150911911,0.139019995512528));
#22108=CARTESIAN_POINT('Ctrl Pts',(4.48738131754991,-2.01821445351738,0.147151381666807));
#22109=CARTESIAN_POINT('Ctrl Pts',(4.54440167627658,-1.8863219557833,0.155282767821084));
#22110=CARTESIAN_POINT('Ctrl Pts',(4.59555177087547,-1.75216636872852,0.163414153975364));
#22111=CARTESIAN_POINT('Ctrl Pts',(4.64668895824192,-1.6180446345407,0.171543488252865));
#22112=CARTESIAN_POINT('Ctrl Pts',(4.6919587153246,-1.48166126644035,0.179672822530368));
#22113=CARTESIAN_POINT('Ctrl Pts',(4.73117981574852,-1.34354777122133,0.187802156807869));
#22114=CARTESIAN_POINT('Ctrl Pts',(4.77040064845697,-1.20543521873771,0.195931435596143));
#22115=CARTESIAN_POINT('Ctrl Pts',(4.80357280941589,-1.06559288723808,0.204060714384417));
#22116=CARTESIAN_POINT('Ctrl Pts',(4.83056506717866,-0.924567030697748,
0.21218999317269));
#22117=CARTESIAN_POINT('Ctrl Pts',(4.857555278148,-0.783551867994089,0.220318655526632));
#22118=CARTESIAN_POINT('Ctrl Pts',(4.87836645982945,-0.641353692644201,
0.228447317880575));
#22119=CARTESIAN_POINT('Ctrl Pts',(4.8929186014829,-0.498528456321814,0.236575980234517));
#22120=CARTESIAN_POINT('Ctrl Pts',(4.907474371369,-0.355667609901753,0.244706669278334));
#22121=CARTESIAN_POINT('Ctrl Pts',(4.91576794811031,-0.212179727344983,
0.252837358322151));
#22122=CARTESIAN_POINT('Ctrl Pts',(4.9177711962389,-0.0686259713447046,
0.260968047365969));
#22123=CARTESIAN_POINT('Ctrl Pts',(4.9191732643376,0.0318469250800603,0.266658695252324));
#22124=CARTESIAN_POINT('Ctrl Pts',(4.91749506144905,0.132351984443032,0.27234934313868));
#22125=CARTESIAN_POINT('Ctrl Pts',(4.91274213444373,0.232696761819521,0.278039991025036));
#22126=CARTESIAN_POINT('Ctrl Pts',(4.90591850659579,0.376758603403428,0.286209875255664));
#22127=CARTESIAN_POINT('Ctrl Pts',(4.89275270583794,0.520543405431197,0.294379759486292));
#22128=CARTESIAN_POINT('Ctrl Pts',(4.87329139158351,0.663486303715512,0.30254964371692));
#22129=CARTESIAN_POINT('Ctrl Pts',(4.85383357489287,0.806403512475477,0.31071805966586));
#22130=CARTESIAN_POINT('Ctrl Pts',(4.82808254692009,0.948478790263434,0.318886475614799));
#22131=CARTESIAN_POINT('Ctrl Pts',(4.79613665314498,1.08915392248261,0.327054891563739));
#22132=CARTESIAN_POINT('Ctrl Pts',(4.76418902515154,1.22983669140763,0.335223750944214));
#22133=CARTESIAN_POINT('Ctrl Pts',(4.72604592905617,1.36911883791727,0.34339261032469));
#22134=CARTESIAN_POINT('Ctrl Pts',(4.68185662625592,1.50645331613149,0.351561469705165));
#22135=CARTESIAN_POINT('Ctrl Pts',(4.63766962985419,1.64378062636571,0.35972990272351));
#22136=CARTESIAN_POINT('Ctrl Pts',(4.5874371611,1.77916015569849,0.367898335741856));
#22137=CARTESIAN_POINT('Ctrl Pts',(4.53135804752916,1.91206101042637,0.376066768760201));
#22138=CARTESIAN_POINT('Ctrl Pts',(4.47526545410476,2.04499381081007,0.384237165241838));
#22139=CARTESIAN_POINT('Ctrl Pts',(4.41332353671453,2.17544643965099,0.392407561723476));
#22140=CARTESIAN_POINT('Ctrl Pts',(4.34577911951618,2.30290835833239,0.400577958205113));
#22141=CARTESIAN_POINT('Ctrl Pts',(4.30036031189514,2.38861741621942,0.406071967649259));
#22142=CARTESIAN_POINT('Ctrl Pts',(4.25240926499502,2.47297462776637,0.411565977093405));
#22143=CARTESIAN_POINT('Ctrl Pts',(4.2020126881557,2.5558310646595,0.41705998653755));
#22144=CARTESIAN_POINT('Ctrl Pts',(4.12724913271787,2.67874897300851,0.425210375024508));
#22145=CARTESIAN_POINT('Ctrl Pts',(4.04707367061566,2.79840842495914,0.433360763511466));
#22146=CARTESIAN_POINT('Ctrl Pts',(3.96179514680109,2.91433736504258,0.441511151998423));
#22147=CARTESIAN_POINT('Ctrl Pts',(3.8765348031365,3.03024159074984,0.449659802940235));
#22148=CARTESIAN_POINT('Ctrl Pts',(3.7861737667134,3.14241662086398,0.457808453882048));
#22149=CARTESIAN_POINT('Ctrl Pts',(3.6910631515518,3.25042087640301,0.46595710482386));
#22150=CARTESIAN_POINT('Ctrl Pts',(3.59594979774117,3.35842824185514,0.474105990400838));
#22151=CARTESIAN_POINT('Ctrl Pts',(3.4960868103159,3.46226433786603,0.482254875977814));
#22152=CARTESIAN_POINT('Ctrl Pts',(3.39186471754661,3.56152169730334,0.490403761554792));
#22153=CARTESIAN_POINT('Ctrl Pts',(3.28764897207037,3.66077301180784,0.498552150851533));
#22154=CARTESIAN_POINT('Ctrl Pts',(3.17907489601818,3.75544591673984,0.506700540148273));
#22155=CARTESIAN_POINT('Ctrl Pts',(3.06656885309214,3.84517080657611,0.514848929445014));
#22156=CARTESIAN_POINT('Ctrl Pts',(2.95403465952901,3.93491814687588,0.52299935758646));
#22157=CARTESIAN_POINT('Ctrl Pts',(2.83756679555529,4.01971478857669,0.531149785727906));
#22158=CARTESIAN_POINT('Ctrl Pts',(2.71762405879757,4.09923194483364,0.539300213869352));
#22159=CARTESIAN_POINT('Ctrl Pts',(2.63531299150039,4.1538008347629,0.544893469929588));
#22160=CARTESIAN_POINT('Ctrl Pts',(2.55136612578541,4.20588424380603,0.550486725989824));
#22161=CARTESIAN_POINT('Ctrl Pts',(2.46593947468516,4.25538782835236,0.55607998205006));
#22162=CARTESIAN_POINT('Ctrl Pts',(2.34133909001987,4.32759205967059,0.56423811358935));
#22163=CARTESIAN_POINT('Ctrl Pts',(2.21354229625245,4.39433327040732,0.572396245128639));
#22164=CARTESIAN_POINT('Ctrl Pts',(2.08304736530668,4.45534473822048,0.580554376667929));
#22165=CARTESIAN_POINT('Ctrl Pts',(1.95257870163044,4.51634392506105,0.588710866060368));
#22166=CARTESIAN_POINT('Ctrl Pts',(1.81941328694919,4.57161552832907,0.596867355452807));
#22167=CARTESIAN_POINT('Ctrl Pts',(1.68407187559563,4.6209398373413,0.605023844845245));
#22168=CARTESIAN_POINT('Ctrl Pts',(1.54872546381792,4.67026596872603,0.61318063559339));
#22169=CARTESIAN_POINT('Ctrl Pts',(1.41120320734963,4.71364424822052,0.621337426341534));
#22170=CARTESIAN_POINT('Ctrl Pts',(1.2720441076259,4.75090379304341,0.629494217089679));
#22171=CARTESIAN_POINT('Ctrl Pts',(1.13289314689424,4.78816115866895,0.637650530771966));
#22172=CARTESIAN_POINT('Ctrl Pts',(0.992105857661266,4.81930042003483,0.645806844454254));
#22173=CARTESIAN_POINT('Ctrl Pts',(0.850234559639156,4.84420109575307,0.653963158136542));
#22174=CARTESIAN_POINT('Ctrl Pts',(0.708328534722006,4.86910786659529,0.662121468300521));
#22175=CARTESIAN_POINT('Ctrl Pts',(0.565338300220735,4.88777294231582,0.6702797784645));
#22176=CARTESIAN_POINT('Ctrl Pts',(0.421825098856181,4.90012720737686,0.678438088628479));
#22177=CARTESIAN_POINT('Ctrl Pts',(0.324125086081751,4.90853766608593,0.683992051606518));
#22178=CARTESIAN_POINT('Ctrl Pts',(0.226182877781484,4.91402443261673,0.689546014584557));
#22179=CARTESIAN_POINT('Ctrl Pts',(0.128176613847126,4.91657948355996,0.695099977562596));
#22180=CARTESIAN_POINT('Ctrl Pts',(-0.0157489469344976,4.92033166352343,
0.703256162729597));
#22181=CARTESIAN_POINT('Ctrl Pts',(-0.159866312834054,4.91776039312803,
0.711412347896599));
#22182=CARTESIAN_POINT('Ctrl Pts',(-0.303610595441317,4.90886989732217,
0.7195685330636));
#22183=CARTESIAN_POINT('Ctrl Pts',(-0.447325607793905,4.89998121186362,
0.727723057408949));
#22184=CARTESIAN_POINT('Ctrl Pts',(-0.590667354579191,4.88477588866314,
0.735877581754297));
#22185=CARTESIAN_POINT('Ctrl Pts',(-0.733073701145311,4.86331019072289,
0.744032106099646));
#22186=CARTESIAN_POINT('Ctrl Pts',(-0.875485160104212,4.84184372216334,
0.752186923192701));
#22187=CARTESIAN_POINT('Ctrl Pts',(-1.01696082017052,4.81411647531375,0.760341740285757));
#22188=CARTESIAN_POINT('Ctrl Pts',(-1.15694589139997,4.78023631914498,0.768496557378813));
#22189=CARTESIAN_POINT('Ctrl Pts',(-1.29692276993108,4.74635814582979,0.776650897207));
#22190=CARTESIAN_POINT('Ctrl Pts',(-1.43540890909048,4.70632786328913,0.784805237035187));
#22191=CARTESIAN_POINT('Ctrl Pts',(-1.5718619475062,4.66030396867865,0.792959576863375));
#22192=CARTESIAN_POINT('Ctrl Pts',(-1.7083486942186,4.61426870468342,0.801115931076213));
#22193=CARTESIAN_POINT('Ctrl Pts',(-1.84280101926073,4.56223697680967,0.809272285289051));
#22194=CARTESIAN_POINT('Ctrl Pts',(-1.97469331186278,4.50441665330644,0.81742863950189));
#22195=CARTESIAN_POINT('Ctrl Pts',(-2.06466235906657,4.46497508085386,0.822992417359629));
#22196=CARTESIAN_POINT('Ctrl Pts',(-2.15344054255843,4.42284101055005,0.828556195217366));
#22197=CARTESIAN_POINT('Ctrl Pts',(-2.24086673186674,4.37809311830081,0.834119973075105));
#22198=CARTESIAN_POINT('Ctrl Pts',(-2.36902428234712,4.31249743918915,0.842275883189753));
#22199=CARTESIAN_POINT('Ctrl Pts',(-2.49432372899232,4.24125833080194,0.850431793304401));
#22200=CARTESIAN_POINT('Ctrl Pts',(-2.61627114275892,4.16464984963525,0.858587703419049));
#22201=CARTESIAN_POINT('Ctrl Pts',(-2.73819360076062,4.08805704590842,0.866741944478412));
#22202=CARTESIAN_POINT('Ctrl Pts',(-2.85676511109277,4.00609723939499,0.874896185537775));
#22203=CARTESIAN_POINT('Ctrl Pts',(-2.97151906855203,3.91908885938194,0.883050426597138));
#22204=CARTESIAN_POINT('Ctrl Pts',(-3.08627700950265,3.83207745901877,0.891204950717317));
#22205=CARTESIAN_POINT('Ctrl Pts',(-3.19721686341115,3.74001733367732,0.899359474837495));
#22206=CARTESIAN_POINT('Ctrl Pts',(-3.30390317391488,3.64326870816512,0.907513998957674));
#22207=CARTESIAN_POINT('Ctrl Pts',(-3.41058317786913,3.54652580175589,0.915668041039345));
#22208=CARTESIAN_POINT('Ctrl Pts',(-3.51300989412653,3.44509517520259,0.923822083121016));
#22209=CARTESIAN_POINT('Ctrl Pts',(-3.61078301066148,3.33937555725894,0.931976125202687));
#22210=CARTESIAN_POINT('Ctrl Pts',(-3.70858022337767,3.23362988471903,0.940132176847752));
#22211=CARTESIAN_POINT('Ctrl Pts',(-3.80172131710608,3.1235933543099,0.948288228492817));
#22212=CARTESIAN_POINT('Ctrl Pts',(-3.88984431783294,3.00970002583693,0.956444280137883));
#22213=CARTESIAN_POINT('Ctrl Pts',(-3.94997448168419,2.93198564427755,0.962009509621126));
#22214=CARTESIAN_POINT('Ctrl Pts',(-4.00776906322076,2.85247629359635,0.96757473910437));
#22215=CARTESIAN_POINT('Ctrl Pts',(-4.06312416161374,2.771318298177,0.973139968587613));
#22216=CARTESIAN_POINT('Ctrl Pts',(-4.14425959693511,2.65236287258256,0.981297072989826));
#22217=CARTESIAN_POINT('Ctrl Pts',(-4.22018261436947,2.52981973419644,0.98945417739204));
#22218=CARTESIAN_POINT('Ctrl Pts',(-4.29059067049875,2.40416612585924,0.997611281794252));
#22219=CARTESIAN_POINT('Ctrl Pts',(-4.36098272190655,2.27854108031892,1.00576653197422));
#22220=CARTESIAN_POINT('Ctrl Pts',(-4.42586215023802,2.14980726757971,1.01392178215418));
#22221=CARTESIAN_POINT('Ctrl Pts',(-4.48497167286734,2.01846777434706,1.02207703233415));
#22222=CARTESIAN_POINT('Ctrl Pts',(-4.54408319317163,1.88712384234366,1.03023255813027));
#22223=CARTESIAN_POINT('Ctrl Pts',(-4.59742427684112,1.75317435724535,1.03838808392639));
#22224=CARTESIAN_POINT('Ctrl Pts',(-4.64478500472299,1.61714418726361,1.04654360972251));
#22225=CARTESIAN_POINT('Ctrl Pts',(-4.69004273227576,1.48715428534852,1.05433699848653));
#22226=CARTESIAN_POINT('Ctrl Pts',(-4.72983964623876,1.35526476022636,1.06213038725054));
#22227=CARTESIAN_POINT('Ctrl Pts',(-4.76403458704967,1.22194824599671,1.06992377601457));
#22228=CARTESIAN_POINT('Origin',(0.,0.,-3.23514056400928));
#22229=CARTESIAN_POINT('',(-4.76403458654079,1.22194824798069,3.16499504358801));
#22230=CARTESIAN_POINT('',(-4.76390408110233,1.22191513442789,2.81993486269365));
#22231=CARTESIAN_POINT('',(-4.76403458704967,1.22194824599672,-3.23514056400928));
#22232=CARTESIAN_POINT('Ctrl Pts',(-4.76403458654079,1.22194824798069,3.16499504358802));
#22233=CARTESIAN_POINT('Ctrl Pts',(-4.74301709350956,1.30388957723802,3.16023305192965));
#22234=CARTESIAN_POINT('Ctrl Pts',(-4.71988804094678,1.38527880975492,3.15548845562783));
#22235=CARTESIAN_POINT('Ctrl Pts',(-4.63323274031351,1.66277434585329,3.13919596261171));
#22236=CARTESIAN_POINT('Ctrl Pts',(-4.55948977731996,1.85545571252533,3.12767309666291));
#22237=CARTESIAN_POINT('Ctrl Pts',(-4.44758466376989,2.10051907133321,3.11248323439081));
#22238=CARTESIAN_POINT('Ctrl Pts',(-4.42018300993925,2.15758470528142,3.10890733213118));
#22239=CARTESIAN_POINT('Ctrl Pts',(-4.3595942934519,2.2777627037162,3.1012864053832));
#22240=CARTESIAN_POINT('Ctrl Pts',(-4.3261207992843,2.34071442323075,3.09724003174466));
#22241=CARTESIAN_POINT('Ctrl Pts',(-4.21449690232407,2.54006000019183,3.08424088263224));
#22242=CARTESIAN_POINT('Ctrl Pts',(-4.13117329665404,2.67344254936908,3.07525509982565));
#22243=CARTESIAN_POINT('Ctrl Pts',(-3.98696109472604,2.88140951109765,3.06076799622857));
#22244=CARTESIAN_POINT('Ctrl Pts',(-3.93002125736954,2.95859976963131,3.05527793768984));
#22245=CARTESIAN_POINT('Ctrl Pts',(-3.84233520324323,3.07046925216586,3.04716206094201));
#22246=CARTESIAN_POINT('Ctrl Pts',(-3.81329739265491,3.10645848015262,3.04452565423422));
#22247=CARTESIAN_POINT('Ctrl Pts',(-3.76265531339808,3.16744360635762,3.04001630630863));
#22248=CARTESIAN_POINT('Ctrl Pts',(-3.74129881898546,3.19264109802267,3.0381405632103));
#22249=CARTESIAN_POINT('Ctrl Pts',(-3.69317444865286,3.24827465476587,3.03397210519915));
#22250=CARTESIAN_POINT('Ctrl Pts',(-3.66628084413627,3.27859887039511,3.03168176438035));
#22251=CARTESIAN_POINT('Ctrl Pts',(-3.57115509424977,3.38322480984051,3.02370705803337));
#22252=CARTESIAN_POINT('Ctrl Pts',(-3.5010139442892,3.45575760080483,3.01804794337373));
#22253=CARTESIAN_POINT('Ctrl Pts',(-3.2782655063435,3.67235366980646,3.00063409780202));
#22254=CARTESIAN_POINT('Ctrl Pts',(-3.11863526189354,3.80884747525298,2.98890623589892));
#22255=CARTESIAN_POINT('Ctrl Pts',(-2.90012562277155,3.97271482868649,2.97350625357134));
#22256=CARTESIAN_POINT('Ctrl Pts',(-2.84874425899097,4.00971916423845,2.96992940156971));
#22257=CARTESIAN_POINT('Ctrl Pts',(-2.73796859246272,4.0862944476954,2.9623038988482));
#22258=CARTESIAN_POINT('Ctrl Pts',(-2.67839847365179,4.12558550823075,2.9582538863873));
#22259=CARTESIAN_POINT('Ctrl Pts',(-2.48593565236306,4.24660357031631,2.94531834486757));
#22260=CARTESIAN_POINT('Ctrl Pts',(-2.35000172649193,4.32330993403215,2.93640050832401));
#22261=CARTESIAN_POINT('Ctrl Pts',(-2.12446260129611,4.43679520551466,2.92194750379035));
#22262=CARTESIAN_POINT('Ctrl Pts',(-2.03701267716492,4.47761906952178,2.91642355302585));
#22263=CARTESIAN_POINT('Ctrl Pts',(-1.90584188975182,4.53421437203681,2.90826640044368));
#22264=CARTESIAN_POINT('Ctrl Pts',(-1.86300749683615,4.55198159030713,2.90562252230479));
#22265=CARTESIAN_POINT('Ctrl Pts',(-1.789210963365,4.58137538532291,2.90110371742155));
#22266=CARTESIAN_POINT('Ctrl Pts',(-1.75837110911383,4.59330026910624,2.89922596806594));
#22267=CARTESIAN_POINT('Ctrl Pts',(-1.68955156410859,4.61911612708915,2.89506067331083));
#22268=CARTESIAN_POINT('Ctrl Pts',(-1.6515161313528,4.63285147510859,2.89277548146293));
#22269=CARTESIAN_POINT('Ctrl Pts',(-1.49684309994213,4.68656006741641,2.88354136197221));
#22270=CARTESIAN_POINT('Ctrl Pts',(-1.3788899561019,4.72261026288304,2.87663262815581));
#22271=CARTESIAN_POINT('Ctrl Pts',(-1.08133037657761,4.8014538781398,2.85938607387253));
#22272=CARTESIAN_POINT('Ctrl Pts',(-0.900438154972333,4.83864079645118,
2.849059325029));
#22273=CARTESIAN_POINT('Ctrl Pts',(-0.655490517643015,4.87478135477,2.83510151755098));
#22274=CARTESIAN_POINT('Ctrl Pts',(-0.592923652246619,4.88278634707422,
2.83153916415954));
#22275=CARTESIAN_POINT('Ctrl Pts',(-0.460320253923246,4.89716569442741,
2.82398821542964));
#22276=CARTESIAN_POINT('Ctrl Pts',(-0.39026597483526,4.90324575079728,2.81999847135481));
#22277=CARTESIAN_POINT('Ctrl Pts',(-0.144186528182758,4.91929594826984,
2.80597134883063));
#22278=CARTESIAN_POINT('Ctrl Pts',(0.0322206753293376,4.92130295271656,
2.79588874217486));
#22279=CARTESIAN_POINT('Ctrl Pts',(0.294936679940447,4.910163528698,2.7808363032379));
#22280=CARTESIAN_POINT('Ctrl Pts',(0.381410029446808,4.90420432353481,2.77587686003766));
#22281=CARTESIAN_POINT('Ctrl Pts',(0.511595013780203,4.89176855960307,2.76841243604769));
#22282=CARTESIAN_POINT('Ctrl Pts',(0.555450862294444,4.88698306576289,2.76589827290617));
#22283=CARTESIAN_POINT('Ctrl Pts',(0.631935092946077,4.87759432519969,2.76151637530628));
#22284=CARTESIAN_POINT('Ctrl Pts',(0.664592636502008,4.87325199652507,2.75964627224388));
#22285=CARTESIAN_POINT('Ctrl Pts',(0.717334627583887,4.86569909000665,2.75662843285732));
#22286=CARTESIAN_POINT('Ctrl Pts',(0.737446953119855,4.86269149755914,2.75547816584134));
#22287=CARTESIAN_POINT('Ctrl Pts',(0.822324901901064,4.84946016344697,2.75062481418638));
#22288=CARTESIAN_POINT('Ctrl Pts',(0.886901865066519,4.83806649000429,2.74693467162407));
#22289=CARTESIAN_POINT('Ctrl Pts',(1.11416335338782,4.79326623990264,2.73392305257977));
#22290=CARTESIAN_POINT('Ctrl Pts',(1.27536359542131,4.75291587480413,2.72464455043326));
#22291=CARTESIAN_POINT('Ctrl Pts',(1.51043444693336,4.68125201074298,2.71085722985321));
#22292=CARTESIAN_POINT('Ctrl Pts',(1.58607870036148,4.65616653542828,2.70638068074325));
#22293=CARTESIAN_POINT('Ctrl Pts',(1.72974064343552,4.60461743233548,2.69778342555605));
#22294=CARTESIAN_POINT('Ctrl Pts',(1.79784452502545,4.5784559944235,2.69366572863656));
#22295=CARTESIAN_POINT('Ctrl Pts',(1.93105867348263,4.5238523325872,2.6855169715415));
#22296=CARTESIAN_POINT('Ctrl Pts',(1.99618483007456,4.49549479986849,2.68148745396551));
#22297=CARTESIAN_POINT('Ctrl Pts',(2.18020214811072,4.41058169327061,2.66996133168117));
#22298=CARTESIAN_POINT('Ctrl Pts',(2.29746691519527,4.35065021975536,2.66244421100876));
#22299=CARTESIAN_POINT('Ctrl Pts',(2.51431108253571,4.22861160825194,2.64820622752174));
#22300=CARTESIAN_POINT('Ctrl Pts',(2.61435069249071,4.16750367848983,2.64149334373158));
#22301=CARTESIAN_POINT('Ctrl Pts',(2.76963977100701,4.06485351755627,2.63085807101604));
#22302=CARTESIAN_POINT('Ctrl Pts',(2.82636187669348,4.02562011270546,2.62692563133518));
#22303=CARTESIAN_POINT('Ctrl Pts',(2.90956359762636,3.96544572155702,2.62109198688894));
#22304=CARTESIAN_POINT('Ctrl Pts',(2.93668276386117,3.9454042232414,2.619180034864));
#22305=CARTESIAN_POINT('Ctrl Pts',(3.00381171141163,3.89471922236461,2.61442135421752));
#22306=CARTESIAN_POINT('Ctrl Pts',(3.0435606852841,3.8637366704063,2.61157948549453));
#22307=CARTESIAN_POINT('Ctrl Pts',(3.20851296260857,3.73103844583217,2.59966497236366));
#22308=CARTESIAN_POINT('Ctrl Pts',(3.32914970354058,3.62380551229913,2.59064915558177));
#22309=CARTESIAN_POINT('Ctrl Pts',(3.51272530632261,3.44370910479892,2.57623487544521));
#22310=CARTESIAN_POINT('Ctrl Pts',(3.57917360483278,3.37459442848034,2.57085690809602));
#22311=CARTESIAN_POINT('Ctrl Pts',(3.69547914704709,3.24631970904161,2.56111239529661));
#22312=CARTESIAN_POINT('Ctrl Pts',(3.74604138963816,3.18784119723681,2.55675309506328));
#22313=CARTESIAN_POINT('Ctrl Pts',(3.83845391152409,3.075724057186,2.54853543458689));
#22314=CARTESIAN_POINT('Ctrl Pts',(3.88061060478513,3.02236134551574,2.54468080638743));
#22315=CARTESIAN_POINT('Ctrl Pts',(3.99483259654115,2.87144595538523,2.53392610208056));
#22316=CARTESIAN_POINT('Ctrl Pts',(4.06441597733861,2.772077107505,2.52700873797852));
#22317=CARTESIAN_POINT('Ctrl Pts',(4.1392598474208,2.65631061448967,2.51912578009965));
#22318=CARTESIAN_POINT('Ctrl Pts',(4.14819439027773,2.64233636479901,2.51817707129355));
#22319=CARTESIAN_POINT('Ctrl Pts',(4.23232773351966,2.50926749725801,2.50917009856783));
#22320=CARTESIAN_POINT('Ctrl Pts',(4.30244881299908,2.38703913574604,2.50109945833231));
#22321=CARTESIAN_POINT('Ctrl Pts',(4.3942314456236,2.20983270358182,2.48970874282804));
#22322=CARTESIAN_POINT('Ctrl Pts',(4.42029994069726,2.1572155959279,2.48636404050036));
#22323=CARTESIAN_POINT('Ctrl Pts',(4.46114803688123,2.07091591345386,2.48094336559317));
#22324=CARTESIAN_POINT('Ctrl Pts',(4.4765027698302,2.0375125808251,2.47886115985932));
#22325=CARTESIAN_POINT('Ctrl Pts',(4.51677639130249,1.94724627757795,2.47327538730181));
#22326=CARTESIAN_POINT('Ctrl Pts',(4.5409955736983,1.89007840409149,2.46978011695905));
#22327=CARTESIAN_POINT('Ctrl Pts',(4.62897814776777,1.67094016382996,2.45651070977139));
#22328=CARTESIAN_POINT('Ctrl Pts',(4.6852098140499,1.50608407077768,2.44678825836016));
#22329=CARTESIAN_POINT('Ctrl Pts',(4.75404268059528,1.2627262848341,2.43259833525474));
#22330=CARTESIAN_POINT('Ctrl Pts',(4.77367402998435,1.18635390185786,2.42816844932864));
#22331=CARTESIAN_POINT('Ctrl Pts',(4.80782650739566,1.03886954455042,2.41964039386002));
#22332=CARTESIAN_POINT('Ctrl Pts',(4.82262638804753,0.967843074402873,2.41554507975477));
#22333=CARTESIAN_POINT('Ctrl Pts',(4.84729339854263,0.834788026932954,2.40788518667186));
#22334=CARTESIAN_POINT('Ctrl Pts',(4.85755405593428,0.77284722098763,2.40432409187291));
#22335=CARTESIAN_POINT('Ctrl Pts',(4.88456636428003,0.58788347840877,2.3936978757305));
#22336=CARTESIAN_POINT('Ctrl Pts',(4.89784874304496,0.464405641996751,2.38661306471273));
#22337=CARTESIAN_POINT('Ctrl Pts',(4.91708768542803,0.187229677655368,2.37072046283848));
#22338=CARTESIAN_POINT('Ctrl Pts',(4.92053708834936,0.0334852921816912,
2.36191159773346));
#22339=CARTESIAN_POINT('Ctrl Pts',(4.91612791451401,-0.146920002736653,
2.35161537595174));
#22340=CARTESIAN_POINT('Ctrl Pts',(4.91525575959535,-0.173666309192137,
2.35009002250873));
#22341=CARTESIAN_POINT('Ctrl Pts',(4.91243195062716,-0.242909670607889,
2.34614465167375));
#22342=CARTESIAN_POINT('Ctrl Pts',(4.91014711883086,-0.285391143376713,
2.34372764056872));
#22343=CARTESIAN_POINT('Ctrl Pts',(4.90456153063559,-0.369000202396119,
2.33897997016327));
#22344=CARTESIAN_POINT('Ctrl Pts',(4.90129383182566,-0.410126539747637,
2.33664919109031));
#22345=CARTESIAN_POINT('Ctrl Pts',(4.8843041383983,-0.594536683360004,2.32620725617069));
#22346=CARTESIAN_POINT('Ctrl Pts',(4.86481343458624,-0.737219074917836,
2.31815132841014));
#22347=CARTESIAN_POINT('Ctrl Pts',(4.81163968367875,-1.0300051071471,2.30148054433339));
#22348=CARTESIAN_POINT('Ctrl Pts',(4.77711888570422,-1.17979716536796,2.29287322705982));
#22349=CARTESIAN_POINT('Ctrl Pts',(4.71627412891487,-1.39681414389121,2.28017403837439));
#22350=CARTESIAN_POINT('Ctrl Pts',(4.69539462386937,-1.46546940659489,2.27612258382524));
#22351=CARTESIAN_POINT('Ctrl Pts',(4.6505359573117,-1.60215409512627,2.26797811397907));
#22352=CARTESIAN_POINT('Ctrl Pts',(4.62654738959398,-1.67016212507325,2.26388597779004));
#22353=CARTESIAN_POINT('Ctrl Pts',(4.54311787112304,-1.89107682197355,2.25045161456738));
#22354=CARTESIAN_POINT('Ctrl Pts',(4.47752269422252,-2.04153884509821,2.24107251947132));
#22355=CARTESIAN_POINT('Ctrl Pts',(4.34644566913616,-2.30534924827536,2.22420933300337));
#22356=CARTESIAN_POINT('Ctrl Pts',(4.28372572544921,-2.41990073701189,2.21673694207674));
#22357=CARTESIAN_POINT('Ctrl Pts',(4.19499847312478,-2.56766802886009,2.20692605885642));
#22358=CARTESIAN_POINT('Ctrl Pts',(4.17301810061789,-2.60323861409947,2.20455086887021));
#22359=CARTESIAN_POINT('Ctrl Pts',(4.13126288140205,-2.66892253452215,2.20014170945751));
#22360=CARTESIAN_POINT('Ctrl Pts',(4.11160560827748,-2.69910723163804,2.19810618492831));
#22361=CARTESIAN_POINT('Ctrl Pts',(4.00080258020134,-2.86523090508467,2.18684227917305));
#22362=CARTESIAN_POINT('Ctrl Pts',(3.903245854618,-2.9967720194161,2.17769022058223));
#22363=CARTESIAN_POINT('Ctrl Pts',(3.7346182800269,-3.20190381884043,2.16281209800813));
#22364=CARTESIAN_POINT('Ctrl Pts',(3.66749544585424,-3.2785726618406,2.15710156045378));
#22365=CARTESIAN_POINT('Ctrl Pts',(3.54126453605472,-3.41402456395137,2.14669108346902));
#22366=CARTESIAN_POINT('Ctrl Pts',(3.48295082773672,-3.47349557987469,2.14199878192741));
#22367=CARTESIAN_POINT('Ctrl Pts',(3.37462703763881,-3.5784973484031,2.13347222010209));
#22368=CARTESIAN_POINT('Ctrl Pts',(3.32513415870264,-3.6245321914051,2.12964384225648));
#22369=CARTESIAN_POINT('Ctrl Pts',(3.1985561824308,-3.73749100751741,2.12001065796144));
#22370=CARTESIAN_POINT('Ctrl Pts',(3.12030739495271,-3.80306219254956,2.11419598515099));
#22371=CARTESIAN_POINT('Ctrl Pts',(2.91665808345992,-3.96319806339806,2.09939842738159));
#22372=CARTESIAN_POINT('Ctrl Pts',(2.78866402178021,-4.05427995477066,2.09040127960862));
#22373=CARTESIAN_POINT('Ctrl Pts',(2.62385733423668,-4.16005569269729,2.07920541802012));
#22374=CARTESIAN_POINT('Ctrl Pts',(2.59093326715756,-4.18064056138376,2.07698745578791));
#22375=CARTESIAN_POINT('Ctrl Pts',(2.53556915187042,-4.21435020671714,2.07328989063368));
#22376=CARTESIAN_POINT('Ctrl Pts',(2.51326263294801,-4.2276908042218,2.07180867508287));
#22377=CARTESIAN_POINT('Ctrl Pts',(2.4548578533147,-4.26199465519438,2.06795325304509));
#22378=CARTESIAN_POINT('Ctrl Pts',(2.41859639468662,-4.28267638924241,2.06558202924274));
#22379=CARTESIAN_POINT('Ctrl Pts',(2.35052290613656,-4.320361770975,2.0611742765807));
#22380=CARTESIAN_POINT('Ctrl Pts',(2.31877863224819,-4.33748192554988,2.05913621807361));
#22381=CARTESIAN_POINT('Ctrl Pts',(2.14291473093149,-4.42984547855592,2.04793129421538));
#22382=CARTESIAN_POINT('Ctrl Pts',(1.99531925365292,-4.49825709304091,2.03883959554162));
#22383=CARTESIAN_POINT('Ctrl Pts',(1.70687352482483,-4.61495841972039,2.02140597009712));
#22384=CARTESIAN_POINT('Ctrl Pts',(1.56668845659874,-4.66441260250427,2.01307618624738));
#22385=CARTESIAN_POINT('Ctrl Pts',(1.35766839859157,-4.72766245922706,2.00076424789439));
#22386=CARTESIAN_POINT('Ctrl Pts',(1.29043298642667,-4.74645534801112,1.99682032972415));
#22387=CARTESIAN_POINT('Ctrl Pts',(1.15032507023243,-4.78241960034736,1.98862664329116));
#22388=CARTESIAN_POINT('Ctrl Pts',(1.07741450888023,-4.79937108350826,1.98437640506048));
#22389=CARTESIAN_POINT('Ctrl Pts',(0.85144200595235,-4.8465000180749,1.97123553793859));
#22390=CARTESIAN_POINT('Ctrl Pts',(0.697310659739751,-4.87106485097146,
1.96231446791112));
#22391=CARTESIAN_POINT('Ctrl Pts',(0.414742367297822,-4.9024112987271,1.94603961614529));
#22392=CARTESIAN_POINT('Ctrl Pts',(0.286703932307502,-4.91156280329857,
1.93869551810289));
#22393=CARTESIAN_POINT('Ctrl Pts',(0.116712562192694,-4.91704233864545,
1.92901450604185));
#22394=CARTESIAN_POINT('Ctrl Pts',(0.0749558047788633,-4.91785612476596,
1.92664214058223));
#22395=CARTESIAN_POINT('Ctrl Pts',(-0.00285776153617473,-4.91838130328029,
1.92223399107222));
#22396=CARTESIAN_POINT('Ctrl Pts',(-0.0389108048909155,-4.91822821714893,
1.92019667001157));
#22397=CARTESIAN_POINT('Ctrl Pts',(-0.239094154068225,-4.91517686468076,
1.90890350944235));
#22398=CARTESIAN_POINT('Ctrl Pts',(-0.403003010553682,-4.90445914633421,
1.89972439242493));
#22399=CARTESIAN_POINT('Ctrl Pts',(-0.66698314074775,-4.87387286348184,
1.88483491075393));
#22400=CARTESIAN_POINT('Ctrl Pts',(-0.767509013794877,-4.85905679071307,
1.87914038210205));
#22401=CARTESIAN_POINT('Ctrl Pts',(-0.949351925815127,-4.82647162024694,
1.86875296343087));
#22402=CARTESIAN_POINT('Ctrl Pts',(-1.03081475002244,-4.80973160439563,
1.86406764314558));
#22403=CARTESIAN_POINT('Ctrl Pts',(-1.17766279317997,-4.77565315806183,
1.85554729392236));
#22404=CARTESIAN_POINT('Ctrl Pts',(-1.2431897163529,-4.75901585769912,1.85171809976792));
#22405=CARTESIAN_POINT('Ctrl Pts',(-1.40700111609575,-4.71380988307916,
1.84206872178752));
#22406=CARTESIAN_POINT('Ctrl Pts',(-1.50477514033721,-4.68351439890763,
1.83623857782591));
#22407=CARTESIAN_POINT('Ctrl Pts',(-1.74963478407155,-4.59918442467976,
1.82144609153528));
#22408=CARTESIAN_POINT('Ctrl Pts',(-1.89521624740806,-4.5411313947083,1.81246978068025));
#22409=CARTESIAN_POINT('Ctrl Pts',(-2.07307948328668,-4.46016019734977,
1.80129706795286));
#22410=CARTESIAN_POINT('Ctrl Pts',(-2.10818977692013,-4.44367228945547,
1.79908143267296));
#22411=CARTESIAN_POINT('Ctrl Pts',(-2.16647951283241,-4.4154528883642,1.79538718523775));
#22412=CARTESIAN_POINT('Ctrl Pts',(-2.18976761399989,-4.40394998780079,
1.79390696352673));
#22413=CARTESIAN_POINT('Ctrl Pts',(-2.25022607114907,-4.37348907042819,
1.79005356745911));
#22414=CARTESIAN_POINT('Ctrl Pts',(-2.28724844388295,-4.35424145299417,
1.7876833752413));
#22415=CARTESIAN_POINT('Ctrl Pts',(-2.35581707396321,-4.31747733564131,
1.78327597814895));
#22416=CARTESIAN_POINT('Ctrl Pts',(-2.38742415044154,-4.30008030054506,
1.78123725029596));
#22417=CARTESIAN_POINT('Ctrl Pts',(-2.56195069180883,-4.20150064974658,
1.76993084478788));
#22418=CARTESIAN_POINT('Ctrl Pts',(-2.70092375277152,-4.11353999126039,
1.76074003648322));
#22419=CARTESIAN_POINT('Ctrl Pts',(-2.91812563713238,-3.96030516646903,
1.74584664913128));
#22420=CARTESIAN_POINT('Ctrl Pts',(-2.99918876353861,-3.89927439259758,
1.74016005178832));
#22421=CARTESIAN_POINT('Ctrl Pts',(-3.14310871835743,-3.78377518228253,
1.72978406090607));
#22422=CARTESIAN_POINT('Ctrl Pts',(-3.20658254161264,-3.73013608663222,
1.72510220339709));
#22423=CARTESIAN_POINT('Ctrl Pts',(-3.31918199949125,-3.62998409654493,
1.71658491825991));
#22424=CARTESIAN_POINT('Ctrl Pts',(-3.36876527755951,-3.58401646978838,
1.71275530171298));
#22425=CARTESIAN_POINT('Ctrl Pts',(-3.49107947195766,-3.46584012182361,
1.70309773334288));
#22426=CARTESIAN_POINT('Ctrl Pts',(-3.56253012367266,-3.39235351037586,
1.69725977399651));
#22427=CARTESIAN_POINT('Ctrl Pts',(-3.73714164171898,-3.20116140870804,
1.68246980303553));
#22428=CARTESIAN_POINT('Ctrl Pts',(-3.83707797472328,-3.08066459589637,
1.6735039705784));
#22429=CARTESIAN_POINT('Ctrl Pts',(-3.95439717399389,-2.92462458050187,
1.66234290045868));
#22430=CARTESIAN_POINT('Ctrl Pts',(-3.97732704932659,-2.89336404739846,
1.66012843706927));
#22431=CARTESIAN_POINT('Ctrl Pts',(-4.01499346437601,-2.84071904928267,
1.65643586047409));
#22432=CARTESIAN_POINT('Ctrl Pts',(-4.029934510683,-2.81948312373489,1.65495613926022));
#22433=CARTESIAN_POINT('Ctrl Pts',(-4.06843999476172,-2.763823307445,1.65110376300936));
#22434=CARTESIAN_POINT('Ctrl Pts',(-4.09173600409548,-2.72921596675235,
1.64873408984005));
#22435=CARTESIAN_POINT('Ctrl Pts',(-4.13761963713916,-2.65914538759537,
1.6439894133055));
#22436=CARTESIAN_POINT('Ctrl Pts',(-4.16019847406307,-2.62368046175027,
1.64161468523822));
#22437=CARTESIAN_POINT('Ctrl Pts',(-4.25014989913843,-2.47831114270315,
1.63197774372176));
#22438=CARTESIAN_POINT('Ctrl Pts',(-4.31364462548109,-2.36606657393467,
1.62475799913469));
#22439=CARTESIAN_POINT('Ctrl Pts',(-4.43714725584738,-2.12620644888387,
1.60964378140722));
#22440=CARTESIAN_POINT('Ctrl Pts',(-4.49622605156831,-1.99824434527271,
1.60175545542597));
#22441=CARTESIAN_POINT('Ctrl Pts',(-4.57985149395893,-1.79455660558094,
1.58936809433175));
#22442=CARTESIAN_POINT('Ctrl Pts',(-4.60819363628214,-1.72047212347358,
1.58489674910551));
#22443=CARTESIAN_POINT('Ctrl Pts',(-4.65756116513055,-1.58144293426877,
1.57655461338746));
#22444=CARTESIAN_POINT('Ctrl Pts',(-4.67905016543438,-1.51668295008528,
1.57268817140172));
#22445=CARTESIAN_POINT('Ctrl Pts',(-4.73266379286164,-1.34311023628735,
1.56236798506226));
#22446=CARTESIAN_POINT('Ctrl Pts',(-4.76238240630405,-1.23359838359574,
1.55590023624027));
#22447=CARTESIAN_POINT('Ctrl Pts',(-4.82635302771853,-0.960876598899115,
1.53988805560355));
#22448=CARTESIAN_POINT('Ctrl Pts',(-4.85614386666074,-0.796764811521365,
1.53033243503737));
#22449=CARTESIAN_POINT('Ctrl Pts',(-4.88525327202945,-0.571916225477431,
1.51738961257693));
#22450=CARTESIAN_POINT('Ctrl Pts',(-4.89187083435975,-0.512237800708074,
1.5139690165124));
#22451=CARTESIAN_POINT('Ctrl Pts',(-4.90077480004421,-0.415860374213651,
1.50847343897031));
#22452=CARTESIAN_POINT('Ctrl Pts',(-4.90374522095142,-0.379231247794851,
1.50639175857398));
#22453=CARTESIAN_POINT('Ctrl Pts',(-4.91052864611597,-0.282079192584326,
1.50088759076744));
#22454=CARTESIAN_POINT('Ctrl Pts',(-4.91363331244746,-0.221513109777117,
1.49747283964233));
#22455=CARTESIAN_POINT('Ctrl Pts',(-4.91716328222741,-0.113672950447315,
1.49140879962172));
#22456=CARTESIAN_POINT('Ctrl Pts',(-4.91802852094442,-0.0664212655845766,
1.48875724195036));
#22457=CARTESIAN_POINT('Ctrl Pts',(-4.91909383189297,0.206973859853138,
1.47342823072295));
#22458=CARTESIAN_POINT('Ctrl Pts',(-4.9043773698152,0.43290146778546,1.46079749396125));
#22459=CARTESIAN_POINT('Ctrl Pts',(-4.86504527327222,0.724694209471723,
1.44419241451101));
#22460=CARTESIAN_POINT('Ctrl Pts',(-4.85451335329151,0.792178751017915,
1.44033263029991));
#22461=CARTESIAN_POINT('Ctrl Pts',(-4.82922543572822,0.934668491773237,
1.43213313249681));
#22462=CARTESIAN_POINT('Ctrl Pts',(-4.81411930489155,1.00959329766838,1.42779205454876));
#22463=CARTESIAN_POINT('Ctrl Pts',(-4.78685401679215,1.13024159751727,1.42074840497709));
#22464=CARTESIAN_POINT('Ctrl Pts',(-4.77577284560566,1.17618406196278,1.41805356987303));
#22465=CARTESIAN_POINT('Ctrl Pts',(-4.76403455895385,1.22194835553447,1.41535621473006));
#22466=CARTESIAN_POINT('',(-4.91824999841653,0.000124803163104314,1.13985943599073));
#22467=CARTESIAN_POINT('Ctrl Pts',(-4.76403458704967,1.22194824599671,1.06992377601457));
#22468=CARTESIAN_POINT('Ctrl Pts',(-4.79982437332077,1.08241387519401,1.07808064693106));
#22469=CARTESIAN_POINT('Ctrl Pts',(-4.82947700993754,0.941316516416591,
1.08623751784756));
#22470=CARTESIAN_POINT('Ctrl Pts',(-4.85288018637509,0.799210209637021,
1.09439438876406));
#22471=CARTESIAN_POINT('Ctrl Pts',(-4.86987080685369,0.69604155077785,1.10031624720942));
#22472=CARTESIAN_POINT('Ctrl Pts',(-4.88356857401184,0.592341382594322,
1.10623810565479));
#22473=CARTESIAN_POINT('Ctrl Pts',(-4.89394752758848,0.488324338642415,
1.11215996410015));
#22474=CARTESIAN_POINT('Ctrl Pts',(-4.9091406584297,0.336059994572651,1.12082861932818));
#22475=CARTESIAN_POINT('Ctrl Pts',(-4.91722391166533,0.183081205296633,
1.12949727455621));
#22476=CARTESIAN_POINT('Ctrl Pts',(-4.91815834240437,0.030026347401424,
1.13816592978423));
#22477=CARTESIAN_POINT('Ctrl Pts',(-4.91821919245222,0.0200594284671798,
1.13873043185307));
#22478=CARTESIAN_POINT('Ctrl Pts',(-4.91824974548893,0.0100921881469089,
1.1392949339219));
#22479=CARTESIAN_POINT('Ctrl Pts',(-4.91824999841653,0.000124803163104037,
1.13985943599073));
#22480=CARTESIAN_POINT('Ctrl Pts',(-4.91833174648596,0.000124732719183029,
1.13985944009773));
#22481=CARTESIAN_POINT('Ctrl Pts',(-4.91765570671746,-0.655079802589096,
1.17696627993604));
#22482=CARTESIAN_POINT('Ctrl Pts',(-4.62138190515468,-2.12911601537738,
1.26041311827852));
#22483=CARTESIAN_POINT('Ctrl Pts',(-3.19184455084248,-4.01249957439954,
1.39019995512517));
#22484=CARTESIAN_POINT('Ctrl Pts',(-0.881775035232405,-5.05079265228957,
1.52921995063769));
#22485=CARTESIAN_POINT('Ctrl Pts',(1.64345394850212,-4.85665391387348,1.66823994615021));
#22486=CARTESIAN_POINT('Ctrl Pts',(3.76766821220293,-3.47745696095566,1.80725994166273));
#22487=CARTESIAN_POINT('Ctrl Pts',(4.97254391099345,-1.24973472203359,1.94627993717524));
#22488=CARTESIAN_POINT('Ctrl Pts',(4.964082610191,1.28293170371797,2.08529993268776));
#22489=CARTESIAN_POINT('Ctrl Pts',(3.74434891334654,3.50255353564616,2.22431992820028));
#22490=CARTESIAN_POINT('Ctrl Pts',(1.61096675357468,4.86752668456681,2.36333992371279));
#22491=CARTESIAN_POINT('Ctrl Pts',(-0.915503054237605,5.04478782126033,
2.50235991922531));
#22492=CARTESIAN_POINT('Ctrl Pts',(-3.21858343365825,3.99108389232243,2.64137991473783));
#22493=CARTESIAN_POINT('Ctrl Pts',(-4.37427005395998,2.44717777195728,2.74723822922728));
#22494=CARTESIAN_POINT('Ctrl Pts',(-4.70630282514833,1.44739632623978,2.80675654521255));
#22495=CARTESIAN_POINT('Ctrl Pts',(-4.76390408110233,1.22191513442789,2.81993486269365));
#22496=CARTESIAN_POINT('Origin',(0.,0.,-3.23514056400928));
#22497=CARTESIAN_POINT('',(-4.76403458685474,1.2219482467567,4.91544887818065));
#22498=CARTESIAN_POINT('',(-4.76403458704967,1.22194824599672,4.56992379268636));
#22499=CARTESIAN_POINT('',(-4.76403458704967,1.22194824599672,-3.23514056400928));
#22500=CARTESIAN_POINT('',(-4.9182499295104,6.30366423602885E-5,3.23536498942701));
#22501=CARTESIAN_POINT('Ctrl Pts',(-4.76403458685474,1.2219482467567,4.91544887818065));
#22502=CARTESIAN_POINT('Ctrl Pts',(-4.75872459594536,1.24265041676701,4.91424056353588));
#22503=CARTESIAN_POINT('Ctrl Pts',(-4.7532796218485,1.2633181343046,4.91303135304027));
#22504=CARTESIAN_POINT('Ctrl Pts',(-4.72876826565284,1.35395449739011,4.90771518220076));
#22505=CARTESIAN_POINT('Ctrl Pts',(-4.70829069555103,1.42353105069983,4.90359920941263));
#22506=CARTESIAN_POINT('Ctrl Pts',(-4.6623696245796,1.56770561514134,4.89499009065993));
#22507=CARTESIAN_POINT('Ctrl Pts',(-4.6366563561763,1.6421964179618,4.89049633022066));
#22508=CARTESIAN_POINT('Ctrl Pts',(-4.54856994431292,1.87879088058015,4.87607157451927));
#22509=CARTESIAN_POINT('Ctrl Pts',(-4.47939718397532,2.03822090576412,4.86611494218855));
#22510=CARTESIAN_POINT('Ctrl Pts',(-4.37409820714046,2.24952076452407,4.85263459154936));
#22511=CARTESIAN_POINT('Ctrl Pts',(-4.34519811752483,2.3048497240378,4.84907763227268));
#22512=CARTESIAN_POINT('Ctrl Pts',(-4.29761244002972,2.39187421693469,4.84344495094849));
#22513=CARTESIAN_POINT('Ctrl Pts',(-4.2796110891683,2.42393562680431,4.84136169040704));
#22514=CARTESIAN_POINT('Ctrl Pts',(-4.23207676064545,2.50641642624834,4.83598038759172));
#22515=CARTESIAN_POINT('Ctrl Pts',(-4.20200178483422,2.55651679646058,4.83268922961721));
#22516=CARTESIAN_POINT('Ctrl Pts',(-4.08767929391668,2.73949109802989,4.82056045222598));
#22517=CARTESIAN_POINT('Ctrl Pts',(-3.99796342003959,2.86883644190503,4.81176760623206));
#22518=CARTESIAN_POINT('Ctrl Pts',(-3.8347620686523,3.08156761558349,4.79673519417109));
#22519=CARTESIAN_POINT('Ctrl Pts',(-3.76437088201348,3.16717074972329,4.7905146411889));
#22520=CARTESIAN_POINT('Ctrl Pts',(-3.64915301124015,3.29801510378949,4.78068783321623));
#22521=CARTESIAN_POINT('Ctrl Pts',(-3.60623642412226,3.34488864815362,4.77709908410771));
#22522=CARTESIAN_POINT('Ctrl Pts',(-3.51319832431968,3.44263245718539,4.76946050996563));
#22523=CARTESIAN_POINT('Ctrl Pts',(-3.46285283556264,3.4932693543772,4.76540937641193));
#22524=CARTESIAN_POINT('Ctrl Pts',(-3.38291046196225,3.57024742224037,4.75909693694634));
#22525=CARTESIAN_POINT('Ctrl Pts',(-3.35406735414445,3.59735764269452,4.75684272799668));
#22526=CARTESIAN_POINT('Ctrl Pts',(-3.2485332245896,3.69417860351414,4.74867715516679));
#22527=CARTESIAN_POINT('Ctrl Pts',(-3.16997127781414,3.76180880463615,4.74275224075534));
#22528=CARTESIAN_POINT('Ctrl Pts',(-2.96966958500406,3.92350560322718,4.72801888073511));
#22529=CARTESIAN_POINT('Ctrl Pts',(-2.84554122766178,4.01444011788983,4.71920885604956));
#22530=CARTESIAN_POINT('Ctrl Pts',(-2.68228811155339,4.12265492714235,4.7080594509058));
#22531=CARTESIAN_POINT('Ctrl Pts',(-2.64692312568772,4.14544945484009,4.70566930382531));
#22532=CARTESIAN_POINT('Ctrl Pts',(-2.57594553464963,4.18991948466762,4.70092420292556));
#22533=CARTESIAN_POINT('Ctrl Pts',(-2.54034108764055,4.21160158325861,4.69856935021158));
#22534=CARTESIAN_POINT('Ctrl Pts',(-2.39717878842673,4.29630734648363,4.68919112793594));
#22535=CARTESIAN_POINT('Ctrl Pts',(-2.28751671115773,4.35568489642668,4.68220753902574));
#22536=CARTESIAN_POINT('Ctrl Pts',(-2.01428863032469,4.49045918857676,4.66513920511973));
#22537=CARTESIAN_POINT('Ctrl Pts',(-1.84861307337425,4.56116334286902,4.65506370180859));
#22538=CARTESIAN_POINT('Ctrl Pts',(-1.62010387772569,4.64418255103284,4.64135803783539));
#22539=CARTESIAN_POINT('Ctrl Pts',(-1.56036172513567,4.66459422901658,4.63779245300159));
#22540=CARTESIAN_POINT('Ctrl Pts',(-1.43169370043139,4.70580677472967,4.63014360619616));
#22541=CARTESIAN_POINT('Ctrl Pts',(-1.36267055697254,4.72625571084432,4.62605876483782));
#22542=CARTESIAN_POINT('Ctrl Pts',(-1.25440772076163,4.75576102763703,4.61967519978006));
#22543=CARTESIAN_POINT('Ctrl Pts',(-1.21546318501877,4.76586308056965,4.61738360773929));
#22544=CARTESIAN_POINT('Ctrl Pts',(-0.988537323067819,4.82176428219472,
4.60405640644271));
#22545=CARTESIAN_POINT('Ctrl Pts',(-0.798108964009134,4.85691650677823,
4.59296669097047));
#22546=CARTESIAN_POINT('Ctrl Pts',(-0.53378563045816,4.88974101300825,4.57774110135792));
#22547=CARTESIAN_POINT('Ctrl Pts',(-0.461271769975431,4.89711372229049,
4.57358226558045));
#22548=CARTESIAN_POINT('Ctrl Pts',(-0.350905677897745,4.90586175915028,
4.5672876304617));
#22549=CARTESIAN_POINT('Ctrl Pts',(-0.313157440626722,4.90841592282859,
4.5651410326665));
#22550=CARTESIAN_POINT('Ctrl Pts',(-0.227774763906893,4.91320418843766,
4.5603012985693));
#22551=CARTESIAN_POINT('Ctrl Pts',(-0.18012976332546,4.91518159204907,4.55761103880365));
#22552=CARTESIAN_POINT('Ctrl Pts',(-0.100548251299887,4.91732573805084,
4.55312851284391));
#22553=CARTESIAN_POINT('Ctrl Pts',(-0.068625578846102,4.91787483677015,
4.5513333916646));
#22554=CARTESIAN_POINT('Ctrl Pts',(0.0696330396414139,4.91890654373806,
4.54356682893646));
#22555=CARTESIAN_POINT('Ctrl Pts',(0.175964038255935,4.91625133711796,4.53761418222368));
#22556=CARTESIAN_POINT('Ctrl Pts',(0.432424076969489,4.90151575348922,4.52322229368798));
#22557=CARTESIAN_POINT('Ctrl Pts',(0.582245202030491,4.88598372858046,4.51478431965105));
#22558=CARTESIAN_POINT('Ctrl Pts',(0.793875437770638,4.85417063662485,4.50272143348942));
#22559=CARTESIAN_POINT('Ctrl Pts',(0.856445676047387,4.84352263083819,4.49913726753732));
#22560=CARTESIAN_POINT('Ctrl Pts',(0.98903877649286,4.81830866884365,4.49149708041534));
#22561=CARTESIAN_POINT('Ctrl Pts',(1.05898542167039,4.80342022390529,4.48743969915181));
#22562=CARTESIAN_POINT('Ctrl Pts',(1.16722617395881,4.77790147430067,4.48111404260705));
#22563=CARTESIAN_POINT('Ctrl Pts',(1.2057584487559,4.76832318308021,4.47885287061183));
#22564=CARTESIAN_POINT('Ctrl Pts',(1.29636491228674,4.74463187222538,4.47351313541038));
#22565=CARTESIAN_POINT('Ctrl Pts',(1.34833114519228,4.73012649551498,4.4704327344894));
#22566=CARTESIAN_POINT('Ctrl Pts',(1.55988243012506,4.66730646384806,4.45781850907384));
#22567=CARTESIAN_POINT('Ctrl Pts',(1.71719981406809,4.61174670253243,4.44826023765811));
#22568=CARTESIAN_POINT('Ctrl Pts',(1.92707851291203,4.52539252908285,4.4353043517684));
#22569=CARTESIAN_POINT('Ctrl Pts',(1.9823409680333,4.50145904659843,4.43187353070182));
#22570=CARTESIAN_POINT('Ctrl Pts',(2.07059769413016,4.4612956247345,4.42636777805977));
#22571=CARTESIAN_POINT('Ctrl Pts',(2.10387336477974,4.44570021112109,4.42428608475689));
#22572=CARTESIAN_POINT('Ctrl Pts',(2.19142474032359,4.40346407723899,4.41879212189009));
#22573=CARTESIAN_POINT('Ctrl Pts',(2.24538939989332,4.37619296257873,4.41538751833949));
#22574=CARTESIAN_POINT('Ctrl Pts',(2.42112530356607,4.28327793584752,4.40421512931147));
#22575=CARTESIAN_POINT('Ctrl Pts',(2.5406311086166,4.21349161532133,4.39647894513423));
#22576=CARTESIAN_POINT('Ctrl Pts',(2.76587536648273,4.06888739876674,4.38147773302931));
#22577=CARTESIAN_POINT('Ctrl Pts',(2.87191445202687,3.99474880295986,4.37422076756146));
#22578=CARTESIAN_POINT('Ctrl Pts',(3.02510246806257,3.87839031171318,4.36337587367283));
#22579=CARTESIAN_POINT('Ctrl Pts',(3.07455997233645,3.83930165809705,4.35981543981702));
#22580=CARTESIAN_POINT('Ctrl Pts',(3.17896670856479,3.75347246871542,4.35216352217035));
#22581=CARTESIAN_POINT('Ctrl Pts',(3.23366658720266,3.70645182724409,4.34807039495645));
#22582=CARTESIAN_POINT('Ctrl Pts',(3.39469505095068,3.56175109452141,4.33575400803965));
#22583=CARTESIAN_POINT('Ctrl Pts',(3.49777597657197,3.46057620717562,4.32750467224476));
#22584=CARTESIAN_POINT('Ctrl Pts',(3.68100057617198,3.26417693829627,4.31213094519123));
#22585=CARTESIAN_POINT('Ctrl Pts',(3.76227353610605,3.17016000416697,4.30501611070408));
#22586=CARTESIAN_POINT('Ctrl Pts',(3.87327501412115,3.03146444890006,4.2948824047719));
#22587=CARTESIAN_POINT('Ctrl Pts',(3.90596900099565,2.98922101838279,4.29184150831157));
#22588=CARTESIAN_POINT('Ctrl Pts',(3.95786830416947,2.91985699975271,4.2869249632931));
#22589=CARTESIAN_POINT('Ctrl Pts',(3.97749799501755,2.89305999545952,4.28504391622395));
#22590=CARTESIAN_POINT('Ctrl Pts',(4.03259562347711,2.81622392818115,4.27970051187964));
#22591=CARTESIAN_POINT('Ctrl Pts',(4.06740118006355,2.76571734853234,4.27624707206658));
#22592=CARTESIAN_POINT('Ctrl Pts',(4.15303689988456,2.6363364744895,4.26752781027166));
#22593=CARTESIAN_POINT('Ctrl Pts',(4.20257151141741,2.55663418841706,4.26227254211923));
#22594=CARTESIAN_POINT('Ctrl Pts',(4.33107060792832,2.33603998398586,4.2479706180758));
#22595=CARTESIAN_POINT('Ctrl Pts',(4.4054239406777,2.19259994381565,4.23892856344424));
#22596=CARTESIAN_POINT('Ctrl Pts',(4.50264309492157,1.98005292636655,4.22576117908536));
#22597=CARTESIAN_POINT('Ctrl Pts',(4.53124746908644,1.91368770871106,4.22168164208227));
#22598=CARTESIAN_POINT('Ctrl Pts',(4.58526700920266,1.78034754263775,4.21353757447278));
#22599=CARTESIAN_POINT('Ctrl Pts',(4.61070203475962,1.71339940042234,4.20947421460826));
#22600=CARTESIAN_POINT('Ctrl Pts',(4.68265471689841,1.51079138660646,4.19724410686154));
#22601=CARTESIAN_POINT('Ctrl Pts',(4.72471015860723,1.37362980795743,4.18905146336735));
#22602=CARTESIAN_POINT('Ctrl Pts',(4.80000625094332,1.0833361021509,4.17188671262462));
#22603=CARTESIAN_POINT('Ctrl Pts',(4.83204710631703,0.930053026692105,4.162921061449));
#22604=CARTESIAN_POINT('Ctrl Pts',(4.86313320006653,0.735370774443273,4.15170256864813));
#22605=CARTESIAN_POINT('Ctrl Pts',(4.86904369420111,0.695160601056541,4.14939464323175));
#22606=CARTESIAN_POINT('Ctrl Pts',(4.88021927933939,0.61197777537219,4.14464130973067));
#22607=CARTESIAN_POINT('Ctrl Pts',(4.88541672773209,0.568999531865461,4.14219676494567));
#22608=CARTESIAN_POINT('Ctrl Pts',(4.89298572745047,0.498627447645299,4.13820796911974));
#22609=CARTESIAN_POINT('Ctrl Pts',(4.89569614480389,0.4712726698626,4.1366608787722));
#22610=CARTESIAN_POINT('Ctrl Pts',(4.90560661652142,0.361915546742582,4.1304868905296));
#22611=CARTESIAN_POINT('Ctrl Pts',(4.91097682293429,0.279760500850208,4.12587283548614));
#22612=CARTESIAN_POINT('Ctrl Pts',(4.92180884448031,0.0102456745276687,
4.11075951620191));
#22613=CARTESIAN_POINT('Ctrl Pts',(4.91862515605703,-0.177292957268644,
4.1002744607054));
#22614=CARTESIAN_POINT('Ctrl Pts',(4.89951080706604,-0.43471631507129,4.08572582500054));
#22615=CARTESIAN_POINT('Ctrl Pts',(4.89275355067037,-0.505120742950989,
4.08173142681248));
#22616=CARTESIAN_POINT('Ctrl Pts',(4.8758993826123,-0.648204475541511,4.07357264459773));
#22617=CARTESIAN_POINT('Ctrl Pts',(4.86568955496173,-0.720852839267989,
4.06940848234307));
#22618=CARTESIAN_POINT('Ctrl Pts',(4.84087089033953,-0.872718008786922,
4.06065140771536));
#22619=CARTESIAN_POINT('Ctrl Pts',(4.82593318999009,-0.951859425678025,
4.05605767065837));
#22620=CARTESIAN_POINT('Ctrl Pts',(4.77271398448199,-1.20019521482268,4.04154347315174));
#22621=CARTESIAN_POINT('Ctrl Pts',(4.72742259732521,-1.36775103513162,4.03159914680417));
#22622=CARTESIAN_POINT('Ctrl Pts',(4.65483336419233,-1.58910351958976,4.01830168312997));
#22623=CARTESIAN_POINT('Ctrl Pts',(4.63526714857286,-1.64530308056132,4.01491182393494));
#22624=CARTESIAN_POINT('Ctrl Pts',(4.6019741903225,-1.73561726265998,4.00944671881719));
#22625=CARTESIAN_POINT('Ctrl Pts',(4.58887641333137,-1.76995678843787,4.00736496267961));
#22626=CARTESIAN_POINT('Ctrl Pts',(4.55294396323284,-1.86108304824452,4.00182903385924));
#22627=CARTESIAN_POINT('Ctrl Pts',(4.52943209988179,-1.91759584691068,3.99838281584693));
#22628=CARTESIAN_POINT('Ctrl Pts',(4.44043422417028,-2.12073361694215,3.98591929696027));
#22629=CARTESIAN_POINT('Ctrl Pts',(4.36883254475307,-2.26456836102405,3.97694600280763));
#22630=CARTESIAN_POINT('Ctrl Pts',(4.23349771611146,-2.50603047032997,3.96142327232429));
#22631=CARTESIAN_POINT('Ctrl Pts',(4.17309654259622,-2.60537068136046,3.95489460859878));
#22632=CARTESIAN_POINT('Ctrl Pts',(4.07165587579385,-2.75961562900759,3.94448005816727));
#22633=CARTESIAN_POINT('Ctrl Pts',(4.03289065707146,-2.81596392026291,3.94061379251168));
#22634=CARTESIAN_POINT('Ctrl Pts',(3.94704970304482,-2.93533064973419,3.93228076635458));
#22635=CARTESIAN_POINT('Ctrl Pts',(3.89961176273528,-2.99806525550416,3.92781202836162));
#22636=CARTESIAN_POINT('Ctrl Pts',(3.79370548613805,-3.13135314884162,3.91811371451174));
#22637=CARTESIAN_POINT('Ctrl Pts',(3.73472840705243,-3.20146487632408,3.91288191374618));
#22638=CARTESIAN_POINT('Ctrl Pts',(3.54903384808436,-3.41009890181161,3.8969050235269));
#22639=CARTESIAN_POINT('Ctrl Pts',(3.41631438007157,-3.54305132670593,3.88614208952505));
#22640=CARTESIAN_POINT('Ctrl Pts',(3.249759756662,-3.69181702036267,3.87343923193496));
#22641=CARTESIAN_POINT('Ctrl Pts',(3.22294161704689,-3.71525217968172,3.87141715764175));
#22642=CARTESIAN_POINT('Ctrl Pts',(3.1635815241555,-3.76599782031712,3.86699363645047));
#22643=CARTESIAN_POINT('Ctrl Pts',(3.13093539749032,-3.79318220438637,3.86459431065765));
#22644=CARTESIAN_POINT('Ctrl Pts',(3.07720222389468,-3.83675937573761,3.86069468497912));
#22645=CARTESIAN_POINT('Ctrl Pts',(3.0563267977331,-3.85340921131592,3.85919155674783));
#22646=CARTESIAN_POINT('Ctrl Pts',(2.91449444688216,-3.96465431163737,3.84905433380022));
#22647=CARTESIAN_POINT('Ctrl Pts',(2.78929963979749,-4.05371062399757,3.84047044368215));
#22648=CARTESIAN_POINT('Ctrl Pts',(2.55548430174767,-4.20406541552771,3.8248886739725));
#22649=CARTESIAN_POINT('Ctrl Pts',(2.44830981143169,-4.26736974701756,3.81790499852495));
#22650=CARTESIAN_POINT('Ctrl Pts',(2.28361493079192,-4.35640087299042,3.80734943345926));
#22651=CARTESIAN_POINT('Ctrl Pts',(2.22781225303845,-4.38519990167338,3.80380240947643));
#22652=CARTESIAN_POINT('Ctrl Pts',(2.10640079285942,-4.44494303554768,3.79614091265941));
#22653=CARTESIAN_POINT('Ctrl Pts',(2.04062794003601,-4.47552011889162,3.7920246219592));
#22654=CARTESIAN_POINT('Ctrl Pts',(1.90202636957154,-4.53626376090469,3.78341452554515));
#22655=CARTESIAN_POINT('Ctrl Pts',(1.8290998713085,-4.56615666707342,3.77892010396938));
#22656=CARTESIAN_POINT('Ctrl Pts',(1.59317665170389,-4.6563035042683,3.76448966422596));
#22657=CARTESIAN_POINT('Ctrl Pts',(1.42769390468811,-4.70967771342347,3.75452798434467));
#22658=CARTESIAN_POINT('Ctrl Pts',(1.19947362647151,-4.77015014843758,3.74104701920025));
#22659=CARTESIAN_POINT('Ctrl Pts',(1.13891390480475,-4.7849707074876,3.7374943714763));
#22660=CARTESIAN_POINT('Ctrl Pts',(1.04271321101288,-4.80658369181909,3.73189501697629));
#22661=CARTESIAN_POINT('Ctrl Pts',(1.00725118997585,-4.81413987218877,3.72984065571702));
#22662=CARTESIAN_POINT('Ctrl Pts',(0.970002510167214,-4.82164714812114,
3.72769261597097));
#22663=CARTESIAN_POINT('Ctrl Pts',(0.968296452116267,-4.82199005303189,
3.72759425257099));
#22664=CARTESIAN_POINT('Ctrl Pts',(0.964872259605189,-4.82267639958138,
3.72739687080567));
#22665=CARTESIAN_POINT('Ctrl Pts',(0.96315412288769,-4.82301982869689,3.7272978525937));
#22666=CARTESIAN_POINT('Ctrl Pts',(0.959683258237725,-4.82371167254044,
3.72709786438853));
#22667=CARTESIAN_POINT('Ctrl Pts',(0.95793052317704,-4.82406005028074,3.72699689481607));
#22668=CARTESIAN_POINT('Ctrl Pts',(0.954370305283553,-4.82476567073531,
3.72679184507216));
#22669=CARTESIAN_POINT('Ctrl Pts',(0.952562810769049,-4.8251228532191,3.72668776556913));
#22670=CARTESIAN_POINT('Ctrl Pts',(0.949983901192228,-4.82563097095457,
3.72653929826264));
#22671=CARTESIAN_POINT('Ctrl Pts',(0.949212650487708,-4.825782736978,3.72649490159276));
#22672=CARTESIAN_POINT('Ctrl Pts',(0.947595669092285,-4.82610052249641,
3.72640182936266));
#22673=CARTESIAN_POINT('Ctrl Pts',(0.946749931063116,-4.82626650459287,
3.72635315420136));
#22674=CARTESIAN_POINT('Ctrl Pts',(0.94496613573125,-4.82661610017683,3.72625050083226));
#22675=CARTESIAN_POINT('Ctrl Pts',(0.944028068413828,-4.82679966253133,
3.72619652316565));
#22676=CARTESIAN_POINT('Ctrl Pts',(0.942037567456653,-4.82718856414173,
3.72608199965397));
#22677=CARTESIAN_POINT('Ctrl Pts',(0.940985120014875,-4.8273938327209,3.72602145455115));
#22678=CARTESIAN_POINT('Ctrl Pts',(0.938738268407798,-4.82783129432263,
3.72589221374912));
#22679=CARTESIAN_POINT('Ctrl Pts',(0.937543844976476,-4.82806338833307,
3.72582351908098));
#22680=CARTESIAN_POINT('Ctrl Pts',(0.934978146894434,-4.82856095314098,
3.725675978963));
#22681=CARTESIAN_POINT('Ctrl Pts',(0.933606844957965,-4.82882628310621,
3.72559713496593));
#22682=CARTESIAN_POINT('Ctrl Pts',(0.930642864549843,-4.82939846688434,
3.72542674564744));
#22683=CARTESIAN_POINT('Ctrl Pts',(0.929050146822228,-4.8297051170827,3.7253352024035));
#22684=CARTESIAN_POINT('Ctrl Pts',(0.925586111278989,-4.8303702801614,3.72513613920447));
#22685=CARTESIAN_POINT('Ctrl Pts',(0.92371473607239,-4.83072849363597,3.72502862226533));
#22686=CARTESIAN_POINT('Ctrl Pts',(0.919619450999208,-4.8315099350758,3.72479338370328));
#22687=CARTESIAN_POINT('Ctrl Pts',(0.917395455888481,-4.83193271527192,
3.72466566652282));
#22688=CARTESIAN_POINT('Ctrl Pts',(0.912499109984687,-4.83286000549962,
3.724384554076));
#22689=CARTESIAN_POINT('Ctrl Pts',(0.909826630682355,-4.83336383490782,
3.7242311654405));
#22690=CARTESIAN_POINT('Ctrl Pts',(0.903909079774386,-4.83447435990249,
3.72389162331597));
#22691=CARTESIAN_POINT('Ctrl Pts',(0.900663811902359,-4.83508000543997,
3.72370547983367));
#22692=CARTESIAN_POINT('Ctrl Pts',(0.893440045184302,-4.83642060999115,
3.7232912803804));
#22693=CARTESIAN_POINT('Ctrl Pts',(0.889461243491172,-4.83715392844322,
3.72306323962401));
#22694=CARTESIAN_POINT('Ctrl Pts',(0.880563966309822,-4.83878240432233,
3.72255351454369));
#22695=CARTESIAN_POINT('Ctrl Pts',(0.87564502048999,-4.83967497393235,3.72227185341808));
#22696=CARTESIAN_POINT('Ctrl Pts',(0.86670625790034,-4.8412828873707,3.7217602719084));
#22697=CARTESIAN_POINT('Ctrl Pts',(0.86268689618551,-4.84200072823426,3.72153033062378));
#22698=CARTESIAN_POINT('Ctrl Pts',(0.798137042833475,-4.85344613072382,
3.71783900884012));
#22699=CARTESIAN_POINT('Ctrl Pts',(0.737411155880095,-4.86304297367625,
3.71438708377863));
#22700=CARTESIAN_POINT('Ctrl Pts',(0.480725322272015,-4.89868977554014,
3.6998515943665));
#22701=CARTESIAN_POINT('Ctrl Pts',(0.283469359160044,-4.91405159390131,
3.68881022822731));
#22702=CARTESIAN_POINT('Ctrl Pts',(0.00839591566748247,-4.91885248625896,
3.6733308756948));
#22703=CARTESIAN_POINT('Ctrl Pts',(-0.0690544227738577,-4.91837489142199,
3.66896449092164));
#22704=CARTESIAN_POINT('Ctrl Pts',(-0.183900738185932,-4.91495336645558,
3.66246769931661));
#22705=CARTESIAN_POINT('Ctrl Pts',(-0.221326823564799,-4.91341027087016,
3.66034706972902));
#22706=CARTESIAN_POINT('Ctrl Pts',(-0.321931021373896,-4.90811050686905,
3.65463581360591));
#22707=CARTESIAN_POINT('Ctrl Pts',(-0.385059977705378,-4.90356166839823,
3.65104043461192));
#22708=CARTESIAN_POINT('Ctrl Pts',(-0.609256774538074,-4.88305064654247,
3.63822399337025));
#22709=CARTESIAN_POINT('Ctrl Pts',(-0.76960278397842,-4.86035882704391,
3.62896620172699));
#22710=CARTESIAN_POINT('Ctrl Pts',(-1.05394210998029,-4.80569423780498,
3.61239131063181));
#22711=CARTESIAN_POINT('Ctrl Pts',(-1.17836301359127,-4.77670935673205,
3.60508399821852));
#22712=CARTESIAN_POINT('Ctrl Pts',(-1.33625636113991,-4.73338143529562,
3.59576934348538));
#22713=CARTESIAN_POINT('Ctrl Pts',(-1.37089167386659,-4.72346662190017,
3.59372359640799));
#22714=CARTESIAN_POINT('Ctrl Pts',(-1.4366942234486,-4.70384503844337,3.58983360870883));
#22715=CARTESIAN_POINT('Ctrl Pts',(-1.46787987238688,-4.69420676407748,
3.587988603152));
#22716=CARTESIAN_POINT('Ctrl Pts',(-1.50319612931055,-4.68290552671892,
3.5858961801963));
#22717=CARTESIAN_POINT('Ctrl Pts',(-1.50742297930052,-4.6815466180397,3.5856456975208));
#22718=CARTESIAN_POINT('Ctrl Pts',(-1.5176041777283,-4.67825820144726,3.58504223382688));
#22719=CARTESIAN_POINT('Ctrl Pts',(-1.52355669728959,-4.67632304593745,
3.58468930915814));
#22720=CARTESIAN_POINT('Ctrl Pts',(-1.53820535320386,-4.67152985056228,
3.58382051190248));
#22721=CARTESIAN_POINT('Ctrl Pts',(-1.54689724169928,-4.6686588842402,3.58330476214194));
#22722=CARTESIAN_POINT('Ctrl Pts',(-1.56833470707311,-4.66151156220546,
3.58203206556754));
#22723=CARTESIAN_POINT('Ctrl Pts',(-1.58107087309591,-4.65720717743159,
3.58127536602299));
#22724=CARTESIAN_POINT('Ctrl Pts',(-1.66297735298287,-4.62915090010136,
3.57640475112087));
#22725=CARTESIAN_POINT('Ctrl Pts',(-1.73162864758464,-4.60391073840025,
3.57230259169348));
#22726=CARTESIAN_POINT('Ctrl Pts',(-1.98613986995693,-4.50383932125865,
3.55697457632233));
#22727=CARTESIAN_POINT('Ctrl Pts',(-2.16793271914314,-4.4192065961505,3.54577534641404));
#22728=CARTESIAN_POINT('Ctrl Pts',(-2.35942627133897,-4.31539064729117,
3.5335010348647));
#22729=CARTESIAN_POINT('Ctrl Pts',(-2.37475260157293,-4.30697560334112,
3.53251526588411));
#22730=CARTESIAN_POINT('Ctrl Pts',(-2.44597846741211,-4.26737270682715,
3.52791790792911));
#22731=CARTESIAN_POINT('Ctrl Pts',(-2.50131021555066,-4.2351773958208,3.52429962307845));
#22732=CARTESIAN_POINT('Ctrl Pts',(-2.60970034299327,-4.16924433607679,
3.51711141238546));
#22733=CARTESIAN_POINT('Ctrl Pts',(-2.66277171809153,-4.13555085622148,
3.51354245357445));
#22734=CARTESIAN_POINT('Ctrl Pts',(-2.78098869205118,-4.05727911630663,
3.50547546513415));
#22735=CARTESIAN_POINT('Ctrl Pts',(-2.84573628082022,-4.01213120185137,
3.50097420268059));
#22736=CARTESIAN_POINT('Ctrl Pts',(-3.0501972384755,-3.86212222932367,3.48648476843722));
#22737=CARTESIAN_POINT('Ctrl Pts',(-3.18542117878974,-3.75137083161058,
3.47647067850075));
#22738=CARTESIAN_POINT('Ctrl Pts',(-3.3599518158474,-3.59217165425268,3.46298303081007));
#22739=CARTESIAN_POINT('Ctrl Pts',(-3.40465464284856,-3.54983102307576,
3.45947483811983));
#22740=CARTESIAN_POINT('Ctrl Pts',(-3.47438135519179,-3.4812597911473,3.45392144346955));
#22741=CARTESIAN_POINT('Ctrl Pts',(-3.4999301834248,-3.45557293175301,3.45186885591697));
#22742=CARTESIAN_POINT('Ctrl Pts',(-3.52760551450541,-3.42712625443474,
3.44962538291886));
#22743=CARTESIAN_POINT('Ctrl Pts',(-3.53001520191382,-3.42464417189484,
3.44942987231861));
#22744=CARTESIAN_POINT('Ctrl Pts',(-3.53756184542947,-3.41685437388873,
3.44881702995062));
#22745=CARTESIAN_POINT('Ctrl Pts',(-3.54268946971256,-3.4115376216713,3.44839983829968));
#22746=CARTESIAN_POINT('Ctrl Pts',(-3.55177159807441,-3.40207795016494,
3.44765946862222));
#22747=CARTESIAN_POINT('Ctrl Pts',(-3.55573087681693,-3.39793963979141,
3.44733622409126));
#22748=CARTESIAN_POINT('Ctrl Pts',(-3.56946438282923,-3.38353484068672,
3.44621327288334));
#22749=CARTESIAN_POINT('Ctrl Pts',(-3.57920146545026,-3.37323299965227,
3.44541406672986));
#22750=CARTESIAN_POINT('Ctrl Pts',(-3.61569469454993,-3.33428722416805,
3.44240691732782));
#22751=CARTESIAN_POINT('Ctrl Pts',(-3.64215274872672,-3.30536575916747,
3.44020254019076));
#22752=CARTESIAN_POINT('Ctrl Pts',(-3.73884428593209,-3.19710087927719,
3.43204860182555));
#22753=CARTESIAN_POINT('Ctrl Pts',(-3.80685411662903,-3.11581009805803,
3.42611687921128));
#22754=CARTESIAN_POINT('Ctrl Pts',(-3.96539681605747,-2.91336003330408,
3.41171056897874));
#22755=CARTESIAN_POINT('Ctrl Pts',(-4.05306975121028,-2.79010096314221,
3.4032372695488));
#22756=CARTESIAN_POINT('Ctrl Pts',(-4.16992940750641,-2.60864930448966,
3.39107185359933));
#22757=CARTESIAN_POINT('Ctrl Pts',(-4.20385808749572,-2.55361303305983,
3.38742067851559));
#22758=CARTESIAN_POINT('Ctrl Pts',(-4.26873482159039,-2.44357658411996,
3.38018919424736));
#22759=CARTESIAN_POINT('Ctrl Pts',(-4.29972893994066,-2.38861768245894,
3.37660997175069));
#22760=CARTESIAN_POINT('Ctrl Pts',(-4.36453759260036,-2.26834771398919,
3.36884244273321));
#22761=CARTESIAN_POINT('Ctrl Pts',(-4.39796195580901,-2.20284367027197,
3.36465228744954));
#22762=CARTESIAN_POINT('Ctrl Pts',(-4.49008613053705,-2.01184002191021,
3.35254486497715));
#22763=CARTESIAN_POINT('Ctrl Pts',(-4.54496847876638,-1.88457817892604,
3.34461111667337));
#22764=CARTESIAN_POINT('Ctrl Pts',(-4.62957081483979,-1.66311969328401,
3.33104556415695));
#22765=CARTESIAN_POINT('Ctrl Pts',(-4.66196237549322,-1.57003191234261,
3.32541395110656));
#22766=CARTESIAN_POINT('Ctrl Pts',(-4.70228757943409,-1.44185923300022,
3.31777033962583));
#22767=CARTESIAN_POINT('Ctrl Pts',(-4.7126656506422,-1.40756848105479,3.31573607428392));
#22768=CARTESIAN_POINT('Ctrl Pts',(-4.73179061504625,-1.34179290536352,
3.31185575524484));
#22769=CARTESIAN_POINT('Ctrl Pts',(-4.74060021149583,-1.3103283126574,3.31000896841078));
#22770=CARTESIAN_POINT('Ctrl Pts',(-4.77333912063673,-1.18874332971476,
3.30290402456549));
#22771=CARTESIAN_POINT('Ctrl Pts',(-4.79501756953323,-1.09803639803183,
3.29766930353714));
#22772=CARTESIAN_POINT('Ctrl Pts',(-4.85988451067937,-0.787859223582681,
3.27990175104639));
#22773=CARTESIAN_POINT('Ctrl Pts',(-4.89067947295103,-0.566085447524859,
3.26741014941425));
#22774=CARTESIAN_POINT('Ctrl Pts',(-4.9104406730498,-0.283411757147819,
3.2514320293728));
#22775=CARTESIAN_POINT('Ctrl Pts',(-4.91352005195395,-0.223764240752992,
3.24805821858464));
#22776=CARTESIAN_POINT('Ctrl Pts',(-4.9173380535753,-0.109381565021347,
3.24157883723314));
#22777=CARTESIAN_POINT('Ctrl Pts',(-4.91825070131855,-0.0546609832033692,
3.23847490589605));
#22778=CARTESIAN_POINT('Ctrl Pts',(-4.91824999959565,6.30663975847573E-5,
3.23536510923081));
#22779=CARTESIAN_POINT('Ctrl Pts',(-4.91824999959594,6.30435251926018E-5,
3.23536511053057));
#22780=CARTESIAN_POINT('Ctrl Pts',(-4.91824924063888,0.0592719879222192,
3.23200045131605));
#22781=CARTESIAN_POINT('Ctrl Pts',(-4.91717929112431,0.118475757485024,
3.22862943975445));
#22782=CARTESIAN_POINT('Ctrl Pts',(-4.91075122842712,0.296325476698879,
3.21847981779956));
#22783=CARTESIAN_POINT('Ctrl Pts',(-4.90216465842163,0.414810448163661,
3.21168634978811));
#22784=CARTESIAN_POINT('Ctrl Pts',(-4.87903381457549,0.627046359997565,
3.19946506954886));
#22785=CARTESIAN_POINT('Ctrl Pts',(-4.86605052775946,0.720909495938399,
3.19404174490195));
#22786=CARTESIAN_POINT('Ctrl Pts',(-4.84275082537018,0.859687092662535,
3.18600725543108));
#22787=CARTESIAN_POINT('Ctrl Pts',(-4.83450163814727,0.904926193268071,
3.1833856758173));
#22788=CARTESIAN_POINT('Ctrl Pts',(-4.81925221365533,0.982383634793772,
3.178895072711));
#22789=CARTESIAN_POINT('Ctrl Pts',(-4.81256020691428,1.01465944351237,3.17702328853145));
#22790=CARTESIAN_POINT('Ctrl Pts',(-4.79687704643086,1.08665159974418,3.17284818000448));
#22791=CARTESIAN_POINT('Ctrl Pts',(-4.78771606600824,1.12632855372567,3.17054728649361));
#22792=CARTESIAN_POINT('Ctrl Pts',(-4.77349677576707,1.18460233696871,3.16716463815977));
#22793=CARTESIAN_POINT('Ctrl Pts',(-4.76882042408035,1.20328960543859,3.1660793840661));
#22794=CARTESIAN_POINT('Ctrl Pts',(-4.76403458654079,1.22194824798069,3.16499504358802));
#22795=CARTESIAN_POINT('',(-4.91824999837926,-0.000126263188378294,2.88985943599073));
#22796=CARTESIAN_POINT('Ctrl Pts',(-4.76390408110233,1.22191513442789,2.81993486269365));
#22797=CARTESIAN_POINT('Ctrl Pts',(-4.86578211211368,0.823111680033963,
2.84324305302354));
#22798=CARTESIAN_POINT('Ctrl Pts',(-4.91787088034465,0.411440562533145,
2.86655124335343));
#22799=CARTESIAN_POINT('Ctrl Pts',(-4.91829688918831,-0.000126223649022064,
2.88985943368333));
#22800=CARTESIAN_POINT('Ctrl Pts',(-4.91824999837926,-0.000126263188378294,
2.88985943599073));
#22801=CARTESIAN_POINT('Ctrl Pts',(-4.91824608066218,-0.152730614993021,
2.89850193437823));
#22802=CARTESIAN_POINT('Ctrl Pts',(-4.91113527331487,-0.305300222186573,
2.90714443276572));
#22803=CARTESIAN_POINT('Ctrl Pts',(-4.89695320922365,-0.457200534967113,
2.91578693115321));
#22804=CARTESIAN_POINT('Ctrl Pts',(-4.89496601075217,-0.47848488874189,
2.91699792268976));
#22805=CARTESIAN_POINT('Ctrl Pts',(-4.89284006026767,-0.499756107960711,
2.91820891422632));
#22806=CARTESIAN_POINT('Ctrl Pts',(-4.89057553724052,-0.521012453828678,
2.91941990576287));
#22807=CARTESIAN_POINT('Ctrl Pts',(-4.87532347766989,-0.664178608266125,
2.92757619953141));
#22808=CARTESIAN_POINT('Ctrl Pts',(-4.85377769937605,-0.806701370795169,
2.93573249329995));
#22809=CARTESIAN_POINT('Ctrl Pts',(-4.82601684941236,-0.9480213244901,2.9438887870685));
#22810=CARTESIAN_POINT('Ctrl Pts',(-4.79826165753946,-1.08931247499177,
2.95204341845816));
#22811=CARTESIAN_POINT('Ctrl Pts',(-4.76429398550897,-1.22940097754245,
2.96019804984783));
#22812=CARTESIAN_POINT('Ctrl Pts',(-4.72424370144954,-1.36773700389158,
2.96835268123749));
#22813=CARTESIAN_POINT('Ctrl Pts',(-4.68419199654067,-1.50607793793789,
2.97650760192607));
#22814=CARTESIAN_POINT('Ctrl Pts',(-4.63805733725252,-1.64266594889159,
2.98466252261464));
#22815=CARTESIAN_POINT('Ctrl Pts',(-4.58601977931309,-1.77696529123365,
2.99281744330322));
#22816=CARTESIAN_POINT('Ctrl Pts',(-4.53398528081815,-1.91125673771359,
3.00097188453949));
#22817=CARTESIAN_POINT('Ctrl Pts',(-4.47604869978663,-2.04325947306684,
3.00912632577575));
#22818=CARTESIAN_POINT('Ctrl Pts',(-4.41243864038556,-2.17245674464014,
3.01728076701202));
#22819=CARTESIAN_POINT('Ctrl Pts',(-4.34881290177494,-2.30168586197986,
3.02543721823215));
#22820=CARTESIAN_POINT('Ctrl Pts',(-4.27951103805168,-2.42810783325788,
3.03359366945228));
#22821=CARTESIAN_POINT('Ctrl Pts',(-4.20480838597866,-2.55122901749402,
3.04175012067241));
#22822=CARTESIAN_POINT('Ctrl Pts',(-4.15385604408756,-2.63520612538982,
3.0473133808734));
#22823=CARTESIAN_POINT('Ctrl Pts',(-4.10039212815736,-2.71764813930332,
3.05287664107439));
#22824=CARTESIAN_POINT('Ctrl Pts',(-4.04451583520027,-2.79840574636958,
3.05843990127538));
#22825=CARTESIAN_POINT('Ctrl Pts',(-3.96259562287657,-2.91680444405521,
3.06659619498704));
#22826=CARTESIAN_POINT('Ctrl Pts',(-3.87545751923364,-3.03162564854714,
3.07475248869871));
#22827=CARTESIAN_POINT('Ctrl Pts',(-3.78343835069359,-3.14241583960509,
3.08290878241037));
#22828=CARTESIAN_POINT('Ctrl Pts',(-3.69143793709251,-3.25318344989748,
3.09106341374241));
#22829=CARTESIAN_POINT('Ctrl Pts',(-3.59455865692401,-3.35992142848364,
3.09921804507445));
#22830=CARTESIAN_POINT('Ctrl Pts',(-3.49317771874209,-3.46220919179992,
3.10737267640649));
#22831=CARTESIAN_POINT('Ctrl Pts',(-3.39179318391245,-3.56450058393495,
3.11552759703686));
#22832=CARTESIAN_POINT('Ctrl Pts',(-3.28590690439984,-3.66234120456008,
3.12368251766722));
#22833=CARTESIAN_POINT('Ctrl Pts',(-3.17593341234408,-3.75534685786234,
3.13183743829759));
#22834=CARTESIAN_POINT('Ctrl Pts',(-3.06596638596307,-3.84834704308047,
3.13999187947547));
#22835=CARTESIAN_POINT('Ctrl Pts',(-2.95191288393539,-3.93651261429531,
3.14814632065335));
#22836=CARTESIAN_POINT('Ctrl Pts',(-2.83422097248897,-4.01949928991207,
3.15630076183123));
#22837=CARTESIAN_POINT('Ctrl Pts',(-2.71650005122249,-4.10250642087277,
3.16445721299322));
#22838=CARTESIAN_POINT('Ctrl Pts',(-2.59513920195962,-4.18033191228843,
3.1726136641552));
#22839=CARTESIAN_POINT('Ctrl Pts',(-2.47061645917429,-4.25267414389547,
3.18077011531719));
#22840=CARTESIAN_POINT('Ctrl Pts',(-2.38568338701886,-4.30201651975012,
3.18633337580742));
#22841=CARTESIAN_POINT('Ctrl Pts',(-2.29927996119546,-4.34880887999953,
3.19189663629766));
#22842=CARTESIAN_POINT('Ctrl Pts',(-2.21156474753462,-4.39296761084829,
3.19745989678789));
#22843=CARTESIAN_POINT('Ctrl Pts',(-2.08296551174435,-4.45770870653298,
3.20561619052175));
#22844=CARTESIAN_POINT('Ctrl Pts',(-1.9514974155078,-4.51681114213254,3.21377248425562));
#22845=CARTESIAN_POINT('Ctrl Pts',(-1.81767327651818,-4.57003795633381,
3.22192877798948));
#22846=CARTESIAN_POINT('Ctrl Pts',(-1.68387641296691,-4.62325392208351,
3.23008340934398));
#22847=CARTESIAN_POINT('Ctrl Pts',(-1.54772477539994,-4.67059653185506,
3.23823804069848));
#22848=CARTESIAN_POINT('Ctrl Pts',(-1.40975087116384,-4.71187707222427,
3.24639267205298));
#22849=CARTESIAN_POINT('Ctrl Pts',(-1.27177207208402,-4.75315907708632,
3.254547592706));
#22850=CARTESIAN_POINT('Ctrl Pts',(-1.13197119649336,-4.78837848268315,
3.26270251335902));
#22851=CARTESIAN_POINT('Ctrl Pts',(-0.990896104083167,-4.81739638948393,
3.27085743401204));
#22852=CARTESIAN_POINT('Ctrl Pts',(-0.849829305904202,-4.84641259023423,
3.27901187521262));
#22853=CARTESIAN_POINT('Ctrl Pts',(-0.707488768775562,-4.86922795512995,
3.28716631641319));
#22854=CARTESIAN_POINT('Ctrl Pts',(-0.56443268956342,-4.88575468085046,
3.29532075761377));
#22855=CARTESIAN_POINT('Ctrl Pts',(-0.421341348532618,-4.90228548023501,
3.30347720879832));
#22856=CARTESIAN_POINT('Ctrl Pts',(-0.277534445550442,-4.91252450437559,
3.31163365998288));
#22857=CARTESIAN_POINT('Ctrl Pts',(-0.133576068908297,-4.91643575126483,
3.31979011116743));
#22858=CARTESIAN_POINT('Ctrl Pts',(-0.0353865604216701,-4.91910349050017,
3.32535337154509));
#22859=CARTESIAN_POINT('Ctrl Pts',(0.0628733040636802,-4.91882851520191,
3.33091663192276));
#22860=CARTESIAN_POINT('Ctrl Pts',(0.161024281146841,-4.91561331304458,
3.33647989230043));
#22861=CARTESIAN_POINT('Ctrl Pts',(0.304923387878341,-4.91089950649726,
3.34463618602925));
#22862=CARTESIAN_POINT('Ctrl Pts',(0.44864230126929,-4.89986174722436,3.35279247975807));
#22863=CARTESIAN_POINT('Ctrl Pts',(0.591617343619236,-4.8825374531312,3.36094877348689));
#22864=CARTESIAN_POINT('Ctrl Pts',(0.734563245433805,-4.86521668999838,
3.3691034048363));
#22865=CARTESIAN_POINT('Ctrl Pts',(0.876765246643208,-4.84161198837913,
3.37725803618572));
#22866=CARTESIAN_POINT('Ctrl Pts',(1.01766547679114,-4.81181255244294,3.38541266753513));
#22867=CARTESIAN_POINT('Ctrl Pts',(1.15857070559862,-4.78201205932441,3.39356758818305));
#22868=CARTESIAN_POINT('Ctrl Pts',(1.29817374275832,-4.74601645769387,3.40172250883096));
#22869=CARTESIAN_POINT('Ctrl Pts',(1.43592708279439,-4.70396603680315,3.40987742947888));
#22870=CARTESIAN_POINT('Ctrl Pts',(1.57367232389534,-4.66191808818376,3.41803187067437));
#22871=CARTESIAN_POINT('Ctrl Pts',(1.70956776563309,-4.61381613110507,3.42618631186987));
#22872=CARTESIAN_POINT('Ctrl Pts',(1.84308128461627,-4.55985026517288,3.43434075306536));
#22873=CARTESIAN_POINT('Ctrl Pts',(1.97662771327811,-4.50587109722215,3.44249720424486));
#22874=CARTESIAN_POINT('Ctrl Pts',(2.10779073549564,-4.44602525745084,3.45065365542437));
#22875=CARTESIAN_POINT('Ctrl Pts',(2.23605785082372,-4.3805511468615,3.45881010660388));
#22876=CARTESIAN_POINT('Ctrl Pts',(2.32354484093858,-4.33589330255544,3.4643733670069));
#22877=CARTESIAN_POINT('Ctrl Pts',(2.40968502205557,-4.28861808848679,3.46993662740992));
#22878=CARTESIAN_POINT('Ctrl Pts',(2.49432220988917,-4.23881348678538,3.47549988781293));
#22879=CARTESIAN_POINT('Ctrl Pts',(2.61840875523016,-4.16579498126317,3.48365618154046));
#22880=CARTESIAN_POINT('Ctrl Pts',(2.7393100219383,-4.08731032099381,3.49181247526798));
#22881=CARTESIAN_POINT('Ctrl Pts',(2.85654901377855,-4.00366217285884,3.49996876899551));
#22882=CARTESIAN_POINT('Ctrl Pts',(2.97376411049001,-3.92003107351662,3.5081234003436));
#22883=CARTESIAN_POINT('Ctrl Pts',(3.08731814915654,-3.83123878003184,3.51627803169169));
#22884=CARTESIAN_POINT('Ctrl Pts',(3.19676402067485,-3.73763064769899,3.52443266303979));
#22885=CARTESIAN_POINT('Ctrl Pts',(3.3062137749589,-3.64401919446929,3.53258758368635));
#22886=CARTESIAN_POINT('Ctrl Pts',(3.41155481370656,-3.54559177517056,3.54074250433291));
#22887=CARTESIAN_POINT('Ctrl Pts',(3.51237358098929,-3.44273363623567,3.54889742497948));
#22888=CARTESIAN_POINT('Ctrl Pts',(3.61318642083169,-3.33988154464193,3.55705186617359));
#22889=CARTESIAN_POINT('Ctrl Pts',(3.70947728754711,-3.23259949423101,3.56520630736769));
#22890=CARTESIAN_POINT('Ctrl Pts',(3.80086997320993,-3.12130910184351,3.5733607485618));
#22891=CARTESIAN_POINT('Ctrl Pts',(3.89228518620883,-3.00999127754444,3.58151719973992));
#22892=CARTESIAN_POINT('Ctrl Pts',(3.9787995929389,-2.89466339558759,3.58967365091805));
#22893=CARTESIAN_POINT('Ctrl Pts',(4.06007733465013,-2.77578008840043,3.59783010209617));
#22894=CARTESIAN_POINT('Ctrl Pts',(4.11551434184627,-2.69469350039641,3.60339336250593));
#22895=CARTESIAN_POINT('Ctrl Pts',(4.16851600626716,-2.61195354475019,3.60895662291568));
#22896=CARTESIAN_POINT('Ctrl Pts',(4.21898731285054,-2.52771222976552,3.61451988332544));
#22897=CARTESIAN_POINT('Ctrl Pts',(4.29298327405157,-2.40420607355315,3.62267617705545));
#22898=CARTESIAN_POINT('Ctrl Pts',(4.36156610255951,-2.27742534222545,3.63083247078547));
#22899=CARTESIAN_POINT('Ctrl Pts',(4.42446187416758,-2.14786409871237,3.63898876451548));
#22900=CARTESIAN_POINT('Ctrl Pts',(4.48734482664008,-2.01832926179393,3.6471433958661));
#22901=CARTESIAN_POINT('Ctrl Pts',(4.54454288850908,-1.88601534411718,3.65529802721671));
#22902=CARTESIAN_POINT('Ctrl Pts',(4.59582880990886,-1.75143958288938,3.66345265856733));
#22903=CARTESIAN_POINT('Ctrl Pts',(4.64711655075822,-1.61685904737255,3.67160757921645));
#22904=CARTESIAN_POINT('Ctrl Pts',(4.69249160875898,-1.48001681910063,3.67976249986557));
#22905=CARTESIAN_POINT('Ctrl Pts',(4.73177528819497,-1.34144909874636,3.68791742051469));
#22906=CARTESIAN_POINT('Ctrl Pts',(4.77105665802468,-1.20288952520729,3.69607186171138));
#22907=CARTESIAN_POINT('Ctrl Pts',(4.8042472754084,-1.06260498477754,3.70422630290806));
#22908=CARTESIAN_POINT('Ctrl Pts',(4.83121864536603,-0.92114573394641,3.71238074410475));
#22909=CARTESIAN_POINT('Ctrl Pts',(4.85819666348274,-0.779651614897389,
3.72053719528544));
#22910=CARTESIAN_POINT('Ctrl Pts',(4.87895230800256,-0.636982535690397,
3.72869364646614));
#22911=CARTESIAN_POINT('Ctrl Pts',(4.89340831385697,-0.493698426547547,
3.73685009764683));
#22912=CARTESIAN_POINT('Ctrl Pts',(4.90326830358628,-0.395968814457495,
3.74241335804388));
#22913=CARTESIAN_POINT('Ctrl Pts',(4.91019865819268,-0.297953270626755,
3.74797661844093));
#22914=CARTESIAN_POINT('Ctrl Pts',(4.91418871620659,-0.19983073839571,3.75353987883798));
#22915=CARTESIAN_POINT('Ctrl Pts',(4.92003853858251,-0.0559733351636417,
3.7616961725661));
#22916=CARTESIAN_POINT('Ctrl Pts',(4.91956821809947,0.0881680433193258,
3.76985246629422));
#22917=CARTESIAN_POINT('Ctrl Pts',(4.91277374208493,0.232028493036589,3.77800876002234));
#22918=CARTESIAN_POINT('Ctrl Pts',(4.9059806508902,0.375859621758297,3.78616339137103));
#22919=CARTESIAN_POINT('Ctrl Pts',(4.89286599134167,0.519409601861859,3.79431802271972));
#22920=CARTESIAN_POINT('Ctrl Pts',(4.87347782343726,0.662115523881759,3.80247265406841));
#22921=CARTESIAN_POINT('Ctrl Pts',(4.85408896770682,0.804826508620698,3.81062757471558));
#22922=CARTESIAN_POINT('Ctrl Pts',(4.82842619959451,0.9466930432584,3.81878249536277));
#22923=CARTESIAN_POINT('Ctrl Pts',(4.79658928665563,1.08715880976077,3.82693741600994));
#22924=CARTESIAN_POINT('Ctrl Pts',(4.76475424550513,1.22761631785595,3.83509185720468));
#22925=CARTESIAN_POINT('Ctrl Pts',(4.72674586065017,1.36667289640204,3.84324629839941));
#22926=CARTESIAN_POINT('Ctrl Pts',(4.68271470376923,1.5037839158614,3.85140073959414));
#22927=CARTESIAN_POINT('Ctrl Pts',(4.63867269367109,1.6409287317454,3.85955719077288));
#22928=CARTESIAN_POINT('Ctrl Pts',(4.58860504723008,1.77612671143222,3.86771364195163));
#22929=CARTESIAN_POINT('Ctrl Pts',(4.53271194629992,1.90884925396689,3.87587009313038));
#22930=CARTESIAN_POINT('Ctrl Pts',(4.49458900917956,1.99937515178435,3.88143335353708));
#22931=CARTESIAN_POINT('Ctrl Pts',(4.4537569969221,2.08874977601324,3.88699661394379));
#22932=CARTESIAN_POINT('Ctrl Pts',(4.4102922031268,2.17681091175577,3.89255987435049));
#22933=CARTESIAN_POINT('Ctrl Pts',(4.34656848732789,2.3059173056205,3.90071616807966));
#22934=CARTESIAN_POINT('Ctrl Pts',(4.27715977948955,2.4322477828378,3.90887246180882));
#22935=CARTESIAN_POINT('Ctrl Pts',(4.20233295759496,2.55530443900746,3.91702875553799));
#22936=CARTESIAN_POINT('Ctrl Pts',(4.12752138656948,2.67833601431827,3.92518338688774));
#22937=CARTESIAN_POINT('Ctrl Pts',(4.0472940782565,2.7980948139492,3.9333380182375));
#22938=CARTESIAN_POINT('Ctrl Pts',(3.96196267552736,2.91410961019452,3.94149264958725));
#22939=CARTESIAN_POINT('Ctrl Pts',(3.87662824553121,3.03012852224896,3.9496475702355));
#22940=CARTESIAN_POINT('Ctrl Pts',(3.78618955403156,3.14240289333373,3.95780249088375));
#22941=CARTESIAN_POINT('Ctrl Pts',(3.69100048784357,3.25049203371405,3.965957411532));
#22942=CARTESIAN_POINT('Ctrl Pts',(3.59581701810863,3.35857481920695,3.97411185272781));
#22943=CARTESIAN_POINT('Ctrl Pts',(3.49588395433114,3.46247261574569,3.98226629392362));
#22944=CARTESIAN_POINT('Ctrl Pts',(3.39159419425969,3.56177931432647,3.99042073511942));
#22945=CARTESIAN_POINT('Ctrl Pts',(3.28727872785898,3.66111049096425,3.99857718629924));
#22946=CARTESIAN_POINT('Ctrl Pts',(3.17860466161559,3.75584807729086,4.00673363747906));
#22947=CARTESIAN_POINT('Ctrl Pts',(3.06600077847207,3.8456237841095,4.01489008865887));
#22948=CARTESIAN_POINT('Ctrl Pts',(2.98919718946959,3.9068569875872,4.02045334906025));
#22949=CARTESIAN_POINT('Ctrl Pts',(2.9105661194372,3.9657826313092,4.02601660946162));
#22950=CARTESIAN_POINT('Ctrl Pts',(2.83025220084745,4.02229481044069,4.031579869863));
#22951=CARTESIAN_POINT('Ctrl Pts',(2.71250399866715,4.10514729243719,4.03973616359172));
#22952=CARTESIAN_POINT('Ctrl Pts',(2.59109313482248,4.18284130981275,4.04789245732045));
#22953=CARTESIAN_POINT('Ctrl Pts',(2.46649225777634,4.25506745009164,4.05604875104917));
#22954=CARTESIAN_POINT('Ctrl Pts',(2.34191677632543,4.32727886956063,4.06420338239847));
#22955=CARTESIAN_POINT('Ctrl Pts',(2.21415286808394,4.39402446744359,4.07235801374778));
#22956=CARTESIAN_POINT('Ctrl Pts',(2.08369971566118,4.4550396807945,4.08051264509708));
#22957=CARTESIAN_POINT('Ctrl Pts',(1.95324193520567,4.51605705875699,4.08866756574487));
#22958=CARTESIAN_POINT('Ctrl Pts',(1.82009502119072,4.57134350021133,4.09682248639267));
#22959=CARTESIAN_POINT('Ctrl Pts',(1.68478062872527,4.62068147523415,4.10497740704047));
#22960=CARTESIAN_POINT('Ctrl Pts',(1.54947419180213,4.67001654952823,4.11313184823582));
#22961=CARTESIAN_POINT('Ctrl Pts',(1.41200084611465,4.71340374331629,4.12128628943118));
#22962=CARTESIAN_POINT('Ctrl Pts',(1.27289994556292,4.75067456168973,4.12944073062653));
#22963=CARTESIAN_POINT('Ctrl Pts',(1.1337647581018,4.78795456692801,4.1375971818059));
#22964=CARTESIAN_POINT('Ctrl Pts',(0.993001537475622,4.81911509730807,4.14575363298527));
#22965=CARTESIAN_POINT('Ctrl Pts',(0.851163041547939,4.84403804064366,4.15391008416463));
#22966=CARTESIAN_POINT('Ctrl Pts',(0.75441943691503,4.86103720127757,4.15947334456826));
#22967=CARTESIAN_POINT('Ctrl Pts',(0.657175864064126,4.87513557740796,4.16503660497188));
#22968=CARTESIAN_POINT('Ctrl Pts',(0.559610002962579,4.88630941581519,4.17059986537551));
#22969=CARTESIAN_POINT('Ctrl Pts',(0.416568735195624,4.90269137558625,4.17875615910436));
#22970=CARTESIAN_POINT('Ctrl Pts',(0.272780852319435,4.91279102578247,4.18691245283321));
#22971=CARTESIAN_POINT('Ctrl Pts',(0.128809443601766,4.91656294475511,4.19506874656206));
#22972=CARTESIAN_POINT('Ctrl Pts',(-0.015132621505391,4.92033409495204,
4.20322337791149));
#22973=CARTESIAN_POINT('Ctrl Pts',(-0.159257803496844,4.91778007801928,
4.21137800926093));
#22974=CARTESIAN_POINT('Ctrl Pts',(-0.303001184225554,4.90890755106041,
4.21953264061036));
#22975=CARTESIAN_POINT('Ctrl Pts',(-0.44674966447892,4.90003470933456,4.22768756125829));
#22976=CARTESIAN_POINT('Ctrl Pts',(-0.590115982131058,4.88484292590067,
4.23584248190621));
#22977=CARTESIAN_POINT('Ctrl Pts',(-0.732538001433465,4.86339090953584,
4.24399740255414));
#22978=CARTESIAN_POINT('Ctrl Pts',(-0.874951647314697,4.84194015439993,
4.25215184374962));
#22979=CARTESIAN_POINT('Ctrl Pts',(-1.01642077512721,4.81422995346369,4.26030628494511));
#22980=CARTESIAN_POINT('Ctrl Pts',(-1.15639118110785,4.78037053990127,4.26846072614059));
#22981=CARTESIAN_POINT('Ctrl Pts',(-1.29639608832175,4.74650278034945,4.27661717732008));
#22982=CARTESIAN_POINT('Ctrl Pts',(-1.43490121004777,4.70648285792434,4.28477362849958));
#22983=CARTESIAN_POINT('Ctrl Pts',(-1.5713646904547,4.66047165768575,4.29293007967907));
#22984=CARTESIAN_POINT('Ctrl Pts',(-1.66444216499551,4.62908885617704,4.29849334008206));
#22985=CARTESIAN_POINT('Ctrl Pts',(-1.75657009904651,4.59491985801175,4.30405660048505));
#22986=CARTESIAN_POINT('Ctrl Pts',(-1.84758112035478,4.55802885754452,4.30961986088805));
#22987=CARTESIAN_POINT('Ctrl Pts',(-1.98101234028353,4.50394297732938,4.3177761546169));
#22988=CARTESIAN_POINT('Ctrl Pts',(-2.11209194922994,4.44398387197782,4.32593244834574));
#22989=CARTESIAN_POINT('Ctrl Pts',(-2.24030381501284,4.37838119388193,4.33408874207459));
#22990=CARTESIAN_POINT('Ctrl Pts',(-2.36848954922497,4.31279188663135,4.34224337342402));
#22991=CARTESIAN_POINT('Ctrl Pts',(-2.49380840855865,4.24156145365597,4.35039800477345));
#22992=CARTESIAN_POINT('Ctrl Pts',(-2.61576758348047,4.1649661477271,4.35855263612289));
#22993=CARTESIAN_POINT('Ctrl Pts',(-2.73773108509767,4.08836812445814,4.36670755677081));
#22994=CARTESIAN_POINT('Ctrl Pts',(-2.85633437841711,4.00640502218146,4.37486247741874));
#22995=CARTESIAN_POINT('Ctrl Pts',(-2.9711120122765,3.91939746300452,4.38301739806667));
#22996=CARTESIAN_POINT('Ctrl Pts',(-3.08588289801159,3.83239501926519,4.39117183926214));
#22997=CARTESIAN_POINT('Ctrl Pts',(-3.19682830814788,3.74034891489571,4.39932628045761));
#22998=CARTESIAN_POINT('Ctrl Pts',(-3.30351441882262,3.64362121345387,4.40748072165309));
#22999=CARTESIAN_POINT('Ctrl Pts',(-3.41022682650205,3.54686966965053,4.41563717283259));
#23000=CARTESIAN_POINT('Ctrl Pts',(-3.51267758864691,3.44543444760598,4.42379362401209));
#23001=CARTESIAN_POINT('Ctrl Pts',(-3.6104679682363,3.33971617249724,4.43195007519159));
#23002=CARTESIAN_POINT('Ctrl Pts',(-3.67716772951608,3.2676090414863,4.43751333559458));
#23003=CARTESIAN_POINT('Ctrl Pts',(-3.74170013640878,3.19351015398629,4.44307659599756));
#23004=CARTESIAN_POINT('Ctrl Pts',(-3.80394896442723,3.11755598803502,4.44863985640055));
#23005=CARTESIAN_POINT('Ctrl Pts',(-3.89521127194652,3.00620043852392,4.45679608998549));
#23006=CARTESIAN_POINT('Ctrl Pts',(-3.98159762459806,2.89081391760571,4.46495232357044));
#23007=CARTESIAN_POINT('Ctrl Pts',(-4.06276479474703,2.7718451048109,4.47310855715538));
#23008=CARTESIAN_POINT('Ctrl Pts',(-4.14392472648238,2.65288690154543,4.48126406337491));
#23009=CARTESIAN_POINT('Ctrl Pts',(-4.21986621201662,2.53034731756149,4.48941956959444));
#23010=CARTESIAN_POINT('Ctrl Pts',(-4.29028870489178,2.40470494888209,4.49757507581397));
#23011=CARTESIAN_POINT('Ctrl Pts',(-4.36070101043729,2.27908075564884,4.5057294022566));
#23012=CARTESIAN_POINT('Ctrl Pts',(-4.42559575425122,2.15035496606688,4.51388372869923));
#23013=CARTESIAN_POINT('Ctrl Pts',(-4.48471780196106,2.01903177272512,4.52203805514186));
#23014=CARTESIAN_POINT('Ctrl Pts',(-4.54384996796169,1.88768610441323,4.53019377713572));
#23015=CARTESIAN_POINT('Ctrl Pts',(-4.59720732361368,1.75374244818986,4.53834949912957));
#23016=CARTESIAN_POINT('Ctrl Pts',(-4.64458218845451,1.61772660149702,4.54650522112343));
#23017=CARTESIAN_POINT('Ctrl Pts',(-4.6899266988647,1.48754001422048,4.55431141164441));
#23018=CARTESIAN_POINT('Ctrl Pts',(-4.72979074132213,1.3554554268238,4.56211760216538));
#23019=CARTESIAN_POINT('Ctrl Pts',(-4.76403458704967,1.22194824599672,4.56992379268636));
#23020=CARTESIAN_POINT('Origin',(0.,0.,-3.23514056400928));
#23021=CARTESIAN_POINT('',(-4.76403458034885,1.22194827212136,6.66505438904205));
#23022=CARTESIAN_POINT('',(-4.76403458747083,1.22194824435476,6.31969203503535));
#23023=CARTESIAN_POINT('',(-4.76403458704967,1.22194824599672,-3.23514056400928));
#23024=CARTESIAN_POINT('Ctrl Pts',(-4.76403458034885,1.22194827212136,6.66505438904205));
#23025=CARTESIAN_POINT('Ctrl Pts',(-4.75505291261507,1.25696528278306,6.66298850631862));
#23026=CARTESIAN_POINT('Ctrl Pts',(-4.74568433605323,1.29188650858914,6.66092426077554));
#23027=CARTESIAN_POINT('Ctrl Pts',(-4.72449276544513,1.36753389112058,6.65644513873832));
#23028=CARTESIAN_POINT('Ctrl Pts',(-4.71252769295444,1.40821291880656,6.6540317517054));
#23029=CARTESIAN_POINT('Ctrl Pts',(-4.68968816954983,1.48230985312338,6.64962908124611));
#23030=CARTESIAN_POINT('Ctrl Pts',(-4.67897876636642,1.51577550090678,6.64763839000519));
#23031=CARTESIAN_POINT('Ctrl Pts',(-4.65012316235656,1.60272490653033,6.64245950934314));
#23032=CARTESIAN_POINT('Ctrl Pts',(-4.63141271811348,1.6560159708516,6.6392778831609));
#23033=CARTESIAN_POINT('Ctrl Pts',(-4.55420902715638,1.86435572332271,6.62678545022193));
#23034=CARTESIAN_POINT('Ctrl Pts',(-4.48881326221942,2.01672959488548,6.61752663069273));
#23035=CARTESIAN_POINT('Ctrl Pts',(-4.37846410109284,2.24175049097104,6.6034728686409));
#23036=CARTESIAN_POINT('Ctrl Pts',(-4.33910929904637,2.31700743735292,6.5987057137598));
#23037=CARTESIAN_POINT('Ctrl Pts',(-4.26698211854503,2.44664491726981,6.5903540301376));
#23038=CARTESIAN_POINT('Ctrl Pts',(-4.23506843588337,2.50148015991019,6.58677612860693));
#23039=CARTESIAN_POINT('Ctrl Pts',(-4.19016792796188,2.57530645830695,6.58189167470789));
#23040=CARTESIAN_POINT('Ctrl Pts',(-4.17809541004328,2.59484669257407,6.58059231133437));
#23041=CARTESIAN_POINT('Ctrl Pts',(-4.12745358626396,2.67554437873976,6.5751982836492));
#23042=CARTESIAN_POINT('Ctrl Pts',(-4.08767517773607,2.73593170727836,6.57109478331718));
#23043=CARTESIAN_POINT('Ctrl Pts',(-3.95523792012639,2.92764460434511,6.55783802478645));
#23044=CARTESIAN_POINT('Ctrl Pts',(-3.85747061087693,3.05531165048024,6.54864997535199));
#23045=CARTESIAN_POINT('Ctrl Pts',(-3.69277304997032,3.24984320941998,6.5340590108467));
#23046=CARTESIAN_POINT('Ctrl Pts',(-3.62986294409184,3.31996217299349,6.52866743971978));
#23047=CARTESIAN_POINT('Ctrl Pts',(-3.54417482744182,3.41012019448496,6.52156590829522));
#23048=CARTESIAN_POINT('Ctrl Pts',(-3.52317027865099,3.43181674178445,6.51984344301824));
#23049=CARTESIAN_POINT('Ctrl Pts',(-3.47075695006869,3.48496844323916,6.5155910619581));
#23050=CARTESIAN_POINT('Ctrl Pts',(-3.43911884753746,3.5161940318753,6.51306391684743));
#23051=CARTESIAN_POINT('Ctrl Pts',(-3.40480624655665,3.54915303496321,6.5103665230686));
#23052=CARTESIAN_POINT('Ctrl Pts',(-3.40254884346799,3.55131724998179,6.5101892614159));
#23053=CARTESIAN_POINT('Ctrl Pts',(-3.3711902837044,3.58132394715409,6.50772959715056));
#23054=CARTESIAN_POINT('Ctrl Pts',(-3.34175020300759,3.60881015874752,6.50545349185294));
#23055=CARTESIAN_POINT('Ctrl Pts',(-3.21999529407643,3.71971687890301,6.49616462279559));
#23056=CARTESIAN_POINT('Ctrl Pts',(-3.12486774972677,3.79998231490071,6.48919307074476));
#23057=CARTESIAN_POINT('Ctrl Pts',(-2.93079217792192,3.95151573038195,6.47539790114408));
#23058=CARTESIAN_POINT('Ctrl Pts',(-2.83203510991717,4.02288407463644,6.46857903313706));
#23059=CARTESIAN_POINT('Ctrl Pts',(-2.67210110888603,4.12965230280731,6.45777664631409));
#23060=CARTESIAN_POINT('Ctrl Pts',(-2.61263679817657,4.16752700209775,6.45381027575064));
#23061=CARTESIAN_POINT('Ctrl Pts',(-2.49930083493202,4.23633499212036,6.44633190318421));
#23062=CARTESIAN_POINT('Ctrl Pts',(-2.44561716792784,4.2675514517855,6.44282276636853));
#23063=CARTESIAN_POINT('Ctrl Pts',(-2.3368380924093,4.32807848562137,6.43577180011353));
#23064=CARTESIAN_POINT('Ctrl Pts',(-2.28174705272022,4.35737374228495,6.43223053360669));
#23065=CARTESIAN_POINT('Ctrl Pts',(-2.04752053710706,4.47626589059256,6.41728968137762));
#23066=CARTESIAN_POINT('Ctrl Pts',(-1.8635582535988,4.55592420511864,6.40582588817387));
#23067=CARTESIAN_POINT('Ctrl Pts',(-1.60647653706328,4.64906094520833,6.39017784295997));
#23068=CARTESIAN_POINT('Ctrl Pts',(-1.53714954813042,4.67244110882362,6.3859946935986));
#23069=CARTESIAN_POINT('Ctrl Pts',(-1.45744423016982,4.69735527515177,6.3812316035804));
#23070=CARTESIAN_POINT('Ctrl Pts',(-1.44755214990964,4.70041307109342,6.38064127473213));
#23071=CARTESIAN_POINT('Ctrl Pts',(-1.43142391771011,4.70534281668329,6.37968013307018));
#23072=CARTESIAN_POINT('Ctrl Pts',(-1.4251935818189,4.707233657808,6.37930916943893));
#23073=CARTESIAN_POINT('Ctrl Pts',(-1.41493713736025,4.71032415108176,6.37869902655022));
#23074=CARTESIAN_POINT('Ctrl Pts',(-1.41091321697408,4.71153102559629,6.3784597855265));
#23075=CARTESIAN_POINT('Ctrl Pts',(-1.40421970740588,4.71352923282481,6.37806205416633));
#23076=CARTESIAN_POINT('Ctrl Pts',(-1.40155098502394,4.71432345642007,6.37790353803809));
#23077=CARTESIAN_POINT('Ctrl Pts',(-1.39706969128375,4.71565296773759,6.37763746140108));
#23078=CARTESIAN_POINT('Ctrl Pts',(-1.39525748384109,4.71618947755765,6.37752988968853));
#23079=CARTESIAN_POINT('Ctrl Pts',(-1.38940424563578,4.7179186785217,6.37718253527371));
#23080=CARTESIAN_POINT('Ctrl Pts',(-1.38536198918495,4.71910722212408,6.37694279147449));
#23081=CARTESIAN_POINT('Ctrl Pts',(-1.37775302904576,4.72133386368881,6.3764917735986));
#23082=CARTESIAN_POINT('Ctrl Pts',(-1.37418666733051,4.72237311791691,6.37628048844328));
#23083=CARTESIAN_POINT('Ctrl Pts',(-1.36739265981452,4.72434457496952,6.37587819476449));
#23084=CARTESIAN_POINT('Ctrl Pts',(-1.36416522986907,4.72527751299334,6.37568717897338));
#23085=CARTESIAN_POINT('Ctrl Pts',(-1.35792813542062,4.72707351798856,6.37531821094751));
#23086=CARTESIAN_POINT('Ctrl Pts',(-1.35491859785934,4.7279370193174,6.37514025431216));
#23087=CARTESIAN_POINT('Ctrl Pts',(-1.34899897616601,4.7296293702954,6.37479037744119));
#23088=CARTESIAN_POINT('Ctrl Pts',(-1.34608894767503,4.73045840939594,6.37461845526892));
#23089=CARTESIAN_POINT('Ctrl Pts',(-1.34023266555534,4.732120966313,6.37427262028375));
#23090=CARTESIAN_POINT('Ctrl Pts',(-1.33728639481368,4.73295441937781,6.37409870824192));
#23091=CARTESIAN_POINT('Ctrl Pts',(-1.33116322699456,4.73468039204758,6.37373742975056));
#23092=CARTESIAN_POINT('Ctrl Pts',(-1.32798620575799,4.73557246688148,6.37355006832861));
#23093=CARTESIAN_POINT('Ctrl Pts',(-1.28986941822881,4.74623389369983,6.37130324390293));
#23094=CARTESIAN_POINT('Ctrl Pts',(-1.25482350222769,4.75561954983394,6.36924857836905));
#23095=CARTESIAN_POINT('Ctrl Pts',(-1.15875382208113,4.78021206934293,6.36364480665791));
#23096=CARTESIAN_POINT('Ctrl Pts',(-1.09753708320753,4.79463766543657,6.36010444669954));
#23097=CARTESIAN_POINT('Ctrl Pts',(-0.871528752343353,4.8433406150259,6.34711399386901));
#23098=CARTESIAN_POINT('Ctrl Pts',(-0.705285391828655,4.87032685390479,
6.33771099634563));
#23099=CARTESIAN_POINT('Ctrl Pts',(-0.458089588479042,4.89752975584298,
6.32375995828713));
#23100=CARTESIAN_POINT('Ctrl Pts',(-0.377990319456553,4.90436203183482,
6.3192448107855));
#23101=CARTESIAN_POINT('Ctrl Pts',(-0.235976477483957,4.91297561879717,
6.31123149464127));
#23102=CARTESIAN_POINT('Ctrl Pts',(-0.174127975481252,4.91555629390999,
6.3077389642151));
#23103=CARTESIAN_POINT('Ctrl Pts',(-0.0906651904439789,4.91746163501598,
6.30301775753363));
#23104=CARTESIAN_POINT('Ctrl Pts',(-0.0690797546309547,4.91781222615031,
6.30179601839482));
#23105=CARTESIAN_POINT('Ctrl Pts',(-0.0375893330700961,4.91811632554639,
6.30001243295995));
#23106=CARTESIAN_POINT('Ctrl Pts',(-0.0276856480126512,4.91818204767071,
6.29945132216187));
#23107=CARTESIAN_POINT('Ctrl Pts',(0.060659982620095,4.91850146177112,6.29444428451768));
#23108=CARTESIAN_POINT('Ctrl Pts',(0.139096678902155,4.91690839582929,6.28998694593467));
#23109=CARTESIAN_POINT('Ctrl Pts',(0.415322610096975,4.9046830776884,6.27423594043361));
#23110=CARTESIAN_POINT('Ctrl Pts',(0.612473311370285,4.88398239220987,6.2628888263114));
#23111=CARTESIAN_POINT('Ctrl Pts',(0.868519580157669,4.84134707518105,6.24804302721082));
#23112=CARTESIAN_POINT('Ctrl Pts',(0.929009381230061,4.83010449364666,6.24452846921355));
#23113=CARTESIAN_POINT('Ctrl Pts',(0.99272249287965,4.81702164391451,6.24082178848324));
#23114=CARTESIAN_POINT('Ctrl Pts',(0.996171586210946,4.81630954535316,6.24062111343635));
#23115=CARTESIAN_POINT('Ctrl Pts',(1.00231462985883,4.81503437367392,6.2402636737355));
#23116=CARTESIAN_POINT('Ctrl Pts',(1.00500887742851,4.81447274301061,6.24010689731957));
#23117=CARTESIAN_POINT('Ctrl Pts',(1.00982492309684,4.81346459305426,6.23982663993378));
#23118=CARTESIAN_POINT('Ctrl Pts',(1.01194689963991,4.81301893162801,6.23970315176186));
#23119=CARTESIAN_POINT('Ctrl Pts',(1.01575287342502,4.81221696574699,6.23948165449011));
#23120=CARTESIAN_POINT('Ctrl Pts',(1.01743697940885,4.81186118027409,6.23938364093418));
#23121=CARTESIAN_POINT('Ctrl Pts',(1.02046693005426,4.81121940886602,6.23920729473771));
#23122=CARTESIAN_POINT('Ctrl Pts',(1.02181284199485,4.81093374216684,6.23912895930726));
#23123=CARTESIAN_POINT('Ctrl Pts',(1.02424101873759,4.81041730233331,6.23898762984015));
#23124=CARTESIAN_POINT('Ctrl Pts',(1.02532332577159,4.81018672867091,6.23892463403583));
#23125=CARTESIAN_POINT('Ctrl Pts',(1.02728067224731,4.80976904680777,6.23881070420938));
#23126=CARTESIAN_POINT('Ctrl Pts',(1.02815573855833,4.80958206505233,6.23875976905424));
#23127=CARTESIAN_POINT('Ctrl Pts',(1.0312575981321,4.80891838303017,6.23857921566115));
#23128=CARTESIAN_POINT('Ctrl Pts',(1.03348411195619,4.80844037487127,6.23844960928702));
#23129=CARTESIAN_POINT('Ctrl Pts',(1.03776957209151,4.80751721943354,6.2382001410315));
#23130=CARTESIAN_POINT('Ctrl Pts',(1.03982856589221,4.80707229542779,6.23808027711206));
#23131=CARTESIAN_POINT('Ctrl Pts',(1.04380143369296,4.80621113411409,6.23784898934926));
#23132=CARTESIAN_POINT('Ctrl Pts',(1.0457153460761,4.80579507611878,6.23773756383627));
#23133=CARTESIAN_POINT('Ctrl Pts',(1.04941790323329,4.80498787502239,6.23752199897226));
#23134=CARTESIAN_POINT('Ctrl Pts',(1.05120657906983,4.80459687620753,6.23741785825338));
#23135=CARTESIAN_POINT('Ctrl Pts',(1.05467635076287,4.80383636485059,6.23721583462095));
#23136=CARTESIAN_POINT('Ctrl Pts',(1.05635747175302,4.80346696845043,6.2371179505881));
#23137=CARTESIAN_POINT('Ctrl Pts',(1.05962803824502,4.80274651971525,6.23692751542934));
#23138=CARTESIAN_POINT('Ctrl Pts',(1.06121750402719,4.80239556067814,6.23683496339089));
#23139=CARTESIAN_POINT('Ctrl Pts',(1.06431922715129,4.80170907539325,6.23665435073376));
#23140=CARTESIAN_POINT('Ctrl Pts',(1.06583150075843,4.8013736236614,6.23656628937612));
#23141=CARTESIAN_POINT('Ctrl Pts',(1.06879219197714,4.80071541699266,6.23639388126694));
#23142=CARTESIAN_POINT('Ctrl Pts',(1.07024062246942,4.800392720872,6.23630953392497));
#23143=CARTESIAN_POINT('Ctrl Pts',(1.07308617863345,4.79975740693362,6.23614382350653));
#23144=CARTESIAN_POINT('Ctrl Pts',(1.07448331426839,4.79944483451463,6.23606245996961));
#23145=CARTESIAN_POINT('Ctrl Pts',(1.07723834989331,4.79882720432505,6.23590201473469));
#23146=CARTESIAN_POINT('Ctrl Pts',(1.07859625726497,4.79852218013702,6.23582293269291));
#23147=CARTESIAN_POINT('Ctrl Pts',(1.08128476850906,4.79791706602453,6.2356663558697));
#23148=CARTESIAN_POINT('Ctrl Pts',(1.0826153773714,4.79761699885891,6.23558886085435));
#23149=CARTESIAN_POINT('Ctrl Pts',(1.08526148481792,4.7970191151694,6.23543474818395));
#23150=CARTESIAN_POINT('Ctrl Pts',(1.08657698606536,4.79672131096697,6.23535813040358));
#23151=CARTESIAN_POINT('Ctrl Pts',(1.08920582483537,4.79612505545591,6.23520501832044));
#23152=CARTESIAN_POINT('Ctrl Pts',(1.09051916260437,4.79582660575023,6.23512852400704));
#23153=CARTESIAN_POINT('Ctrl Pts',(1.09315802586402,4.79522579670934,6.23497482304469));
#23154=CARTESIAN_POINT('Ctrl Pts',(1.09448354891775,4.79492342713498,6.23489761651428));
#23155=CARTESIAN_POINT('Ctrl Pts',(1.13163389226899,4.78643272832944,6.23273372039523));
#23156=CARTESIAN_POINT('Ctrl Pts',(1.167365992197,4.7778436778543,6.23065186505073));
#23157=CARTESIAN_POINT('Ctrl Pts',(1.26108226973158,4.75420265967878,6.22518900332407));
#23158=CARTESIAN_POINT('Ctrl Pts',(1.3188935781906,4.73849040072027,6.2218154483081));
#23159=CARTESIAN_POINT('Ctrl Pts',(1.54600360218853,4.67228682817117,6.20851912784474));
#23160=CARTESIAN_POINT('Ctrl Pts',(1.71281707632494,4.61374572264444,6.19865240601285));
#23161=CARTESIAN_POINT('Ctrl Pts',(1.949312425594,4.51615252936203,6.18429830060129));
#23162=CARTESIAN_POINT('Ctrl Pts',(2.02176505733343,4.48418537735761,6.17984973597581));
#23163=CARTESIAN_POINT('Ctrl Pts',(2.15920419261345,4.41953689463318,6.17129398964628));
#23164=CARTESIAN_POINT('Ctrl Pts',(2.2242996883834,4.38713572201046,6.16718972478682));
#23165=CARTESIAN_POINT('Ctrl Pts',(2.34414037810097,4.32413214865336,6.15952609099346));
#23166=CARTESIAN_POINT('Ctrl Pts',(2.39906509548357,4.29390259684177,6.15597027785549));
#23167=CARTESIAN_POINT('Ctrl Pts',(2.57346388113466,4.19352578333136,6.14453177441374));
#23168=CARTESIAN_POINT('Ctrl Pts',(2.69055640005642,4.11937862322729,6.13662254651122));
#23169=CARTESIAN_POINT('Ctrl Pts',(2.90104761213393,3.973280459457,6.12196146902832));
#23170=CARTESIAN_POINT('Ctrl Pts',(2.99529419151232,3.90272310855013,6.11521961735173));
#23171=CARTESIAN_POINT('Ctrl Pts',(3.12632222687714,3.79708496361556,6.10560355625454));
#23172=CARTESIAN_POINT('Ctrl Pts',(3.16523304397283,3.76471044376927,6.10271574716572));
#23173=CARTESIAN_POINT('Ctrl Pts',(3.23541406174684,3.70446120902258,6.09745073254636));
#23174=CARTESIAN_POINT('Ctrl Pts',(3.26684121389002,3.67677651442494,6.09507163172042));
#23175=CARTESIAN_POINT('Ctrl Pts',(3.32897585484533,3.6206154474906,6.09032693093945));
#23176=CARTESIAN_POINT('Ctrl Pts',(3.35968094526277,3.59214148680241,6.08796152479812));
#23177=CARTESIAN_POINT('Ctrl Pts',(3.48553005266798,3.47241162842158,6.07816883169562));
#23178=CARTESIAN_POINT('Ctrl Pts',(3.57735020373068,3.37774015181016,6.07078637853904));
#23179=CARTESIAN_POINT('Ctrl Pts',(3.74907740499654,3.18581287119434,6.05635853620959));
#23180=CARTESIAN_POINT('Ctrl Pts',(3.82927533135065,3.08895373242096,6.04931881081417));
#23181=CARTESIAN_POINT('Ctrl Pts',(3.92977793066721,2.95763442778058,6.04002203543174));
#23182=CARTESIAN_POINT('Ctrl Pts',(3.95349998667428,2.92584924857875,6.03779009309128));
#23183=CARTESIAN_POINT('Ctrl Pts',(4.01888434562909,2.83599351169465,6.03152822775744));
#23184=CARTESIAN_POINT('Ctrl Pts',(4.05966887959046,2.77729707007067,6.02749255185915));
#23185=CARTESIAN_POINT('Ctrl Pts',(4.13917549979702,2.65737716083884,6.01934613489417));
#23186=CARTESIAN_POINT('Ctrl Pts',(4.17785319833812,2.59614515805817,6.01523610089585));
#23187=CARTESIAN_POINT('Ctrl Pts',(4.2969355736181,2.39806482897949,6.00208646252366));
#23188=CARTESIAN_POINT('Ctrl Pts',(4.37207426185078,2.25817089607497,5.99301328546572));
#23189=CARTESIAN_POINT('Ctrl Pts',(4.48123260798426,2.02898765791976,5.9784817257964));
#23190=CARTESIAN_POINT('Ctrl Pts',(4.51964665389634,1.9419142271221,5.97303465029629));
#23191=CARTESIAN_POINT('Ctrl Pts',(4.57880891142312,1.79652796864221,5.96407262707049));
#23192=CARTESIAN_POINT('Ctrl Pts',(4.60102584087305,1.73884016898957,5.96055030402325));
#23193=CARTESIAN_POINT('Ctrl Pts',(4.63350930777968,1.64950887009522,5.95515245527998));
#23194=CARTESIAN_POINT('Ctrl Pts',(4.64455198390078,1.6181547890226,5.95326866549175));
#23195=CARTESIAN_POINT('Ctrl Pts',(4.67240361893244,1.53643940268731,5.94838669246539));
#23196=CARTESIAN_POINT('Ctrl Pts',(4.68871652131276,1.48591355539177,5.94539436083786));
#23197=CARTESIAN_POINT('Ctrl Pts',(4.75811188040225,1.25844321002308,5.93201661840089));
#23198=CARTESIAN_POINT('Ctrl Pts',(4.80201823956137,1.07885572934138,5.92170206957395));
#23199=CARTESIAN_POINT('Ctrl Pts',(4.85034696894252,0.818381051162789,5.90684014254788));
#23200=CARTESIAN_POINT('Ctrl Pts',(4.86304506213647,0.739192687172608,5.90233555704712));
#23201=CARTESIAN_POINT('Ctrl Pts',(4.88361905482338,0.587200844381081,5.89369669429945));
#23202=CARTESIAN_POINT('Ctrl Pts',(4.89181645729435,0.514462329409633,5.88956551909227));
#23203=CARTESIAN_POINT('Ctrl Pts',(4.90399320985336,0.379383758089831,5.88188943061856));
#23204=CARTESIAN_POINT('Ctrl Pts',(4.90841420571629,0.317098276177648,5.87834828382102));
#23205=CARTESIAN_POINT('Ctrl Pts',(4.92332524789386,0.0296048401421414,
5.86198551973232));
#23206=CARTESIAN_POINT('Ctrl Pts',(4.91950826643874,-0.196070324342683,
5.8490768039767));
#23207=CARTESIAN_POINT('Ctrl Pts',(4.89460045066212,-0.486203970079088,
5.83241752508645));
#23208=CARTESIAN_POINT('Ctrl Pts',(4.8876617575062,-0.551607208692117,5.82865910047377));
#23209=CARTESIAN_POINT('Ctrl Pts',(4.87319008772243,-0.666080810443444,
5.82208120485445));
#23210=CARTESIAN_POINT('Ctrl Pts',(4.8662218998351,-0.715213099881239,5.8192581089666));
#23211=CARTESIAN_POINT('Ctrl Pts',(4.85271582207133,-0.801076347845169,
5.81432797416755));
#23212=CARTESIAN_POINT('Ctrl Pts',(4.84650137656249,-0.837853565599088,
5.81221781562353));
#23213=CARTESIAN_POINT('Ctrl Pts',(4.82626970415786,-0.949817277586713,
5.80579408290496));
#23214=CARTESIAN_POINT('Ctrl Pts',(4.81091654357623,-1.02475087476453,5.80149472781692));
#23215=CARTESIAN_POINT('Ctrl Pts',(4.7506690329984,-1.28747874373157,5.78636774469862));
#23216=CARTESIAN_POINT('Ctrl Pts',(4.69647287657621,-1.47295629382967,5.7755862874365));
#23217=CARTESIAN_POINT('Ctrl Pts',(4.61802032372933,-1.69253655714347,5.76247879942884));
#23218=CARTESIAN_POINT('Ctrl Pts',(4.60406438065428,-1.73013955019648,5.76022192687771));
#23219=CARTESIAN_POINT('Ctrl Pts',(4.56382132221355,-1.83463431979489,5.75391289574751));
#23220=CARTESIAN_POINT('Ctrl Pts',(4.53652580362779,-1.90112640945508,5.74985498900001));
#23221=CARTESIAN_POINT('Ctrl Pts',(4.48250597255629,-2.02492416873906,5.74220820755223));
#23222=CARTESIAN_POINT('Ctrl Pts',(4.4561145790334,-2.0823593425554,5.73862250780528));
#23223=CARTESIAN_POINT('Ctrl Pts',(4.34369670265896,-2.31508199843801,5.72392774161848));
#23224=CARTESIAN_POINT('Ctrl Pts',(4.2483765231206,-2.48567911650042,5.71275747209068));
#23225=CARTESIAN_POINT('Ctrl Pts',(4.10032533005141,-2.71713776285327,5.69703075605458));
#23226=CARTESIAN_POINT('Ctrl Pts',(4.05586199582944,-2.78307186925759,5.69248214360016));
#23227=CARTESIAN_POINT('Ctrl Pts',(3.99423885287356,-2.86983676563528,5.68640996191761));
#23228=CARTESIAN_POINT('Ctrl Pts',(3.97847832544998,-2.89164612277454,5.68487614336304));
#23229=CARTESIAN_POINT('Ctrl Pts',(3.93725040500319,-2.94772200147618,5.68091357106846));
#23230=CARTESIAN_POINT('Ctrl Pts',(3.91151424203479,-2.98178841304458,5.67848782793685));
#23231=CARTESIAN_POINT('Ctrl Pts',(3.86357452505938,-3.04355628505292,5.67405768486157));
#23232=CARTESIAN_POINT('Ctrl Pts',(3.8415083913864,-3.07136065605109,5.6720514163767));
#23233=CARTESIAN_POINT('Ctrl Pts',(3.70744762645759,-3.2365784101876,5.66004738376139));
#23234=CARTESIAN_POINT('Ctrl Pts',(3.58839016664414,-3.36809520616232,5.65014111709629));
#23235=CARTESIAN_POINT('Ctrl Pts',(3.38561070118491,-3.56910942128526,5.63414062683164));
#23236=CARTESIAN_POINT('Ctrl Pts',(3.30623536207469,-3.64276121982292,5.62806939701597));
#23237=CARTESIAN_POINT('Ctrl Pts',(3.16657322201732,-3.76402460780622,5.61765921094442));
#23238=CARTESIAN_POINT('Ctrl Pts',(3.10748324938472,-3.81295356501981,5.6133326164611));
#23239=CARTESIAN_POINT('Ctrl Pts',(2.99374741149748,-3.90273105610842,5.60513657746522));
#23240=CARTESIAN_POINT('Ctrl Pts',(2.93934869717951,-3.94386388677907,5.60127062206718));
#23241=CARTESIAN_POINT('Ctrl Pts',(2.69841940681127,-4.11828483397017,5.58436774804399));
#23242=CARTESIAN_POINT('Ctrl Pts',(2.50355613317588,-4.23956849098936,5.57124124977485));
#23243=CARTESIAN_POINT('Ctrl Pts',(2.26012341648045,-4.36842752941848,5.55548437682585));
#23244=CARTESIAN_POINT('Ctrl Pts',(2.21899404375236,-4.38946265511874,5.55284364332822));
#23245=CARTESIAN_POINT('Ctrl Pts',(2.12391509053258,-4.43641173976063,5.54679044063224));
#23246=CARTESIAN_POINT('Ctrl Pts',(2.06977624111165,-4.46192681147799,5.5433809760215));
#23247=CARTESIAN_POINT('Ctrl Pts',(1.98166225238367,-4.50150511145434,5.53789645488314));
#23248=CARTESIAN_POINT('Ctrl Pts',(1.94797193671454,-4.51618632522818,5.53581476779011));
#23249=CARTESIAN_POINT('Ctrl Pts',(1.85807588661132,-4.55416717389434,5.53029929125383));
#23250=CARTESIAN_POINT('Ctrl Pts',(1.80159692573019,-4.57680382999001,5.52687331592428));
#23251=CARTESIAN_POINT('Ctrl Pts',(1.58448687803319,-4.65917935072152,5.5138229035384));
#23252=CARTESIAN_POINT('Ctrl Pts',(1.42119322624803,-4.71155613805953,5.50424980576285));
#23253=CARTESIAN_POINT('Ctrl Pts',(1.17769164561383,-4.77584562496961,5.49012177751472));
#23254=CARTESIAN_POINT('Ctrl Pts',(1.09939237966458,-4.79447549596105,5.48560135584779));
#23255=CARTESIAN_POINT('Ctrl Pts',(0.948940420264369,-4.826393281715,5.47693898370612));
#23256=CARTESIAN_POINT('Ctrl Pts',(0.876878241277379,-4.84000458844437,
5.47280018791893));
#23257=CARTESIAN_POINT('Ctrl Pts',(0.734753277355558,-4.86357118520218,
5.46464667886968));
#23258=CARTESIAN_POINT('Ctrl Pts',(0.664726309320707,-4.87363579183947,
5.4606337039462));
#23259=CARTESIAN_POINT('Ctrl Pts',(0.407986319430107,-4.90489919755143,
5.44592554294287));
#23260=CARTESIAN_POINT('Ctrl Pts',(0.220319240221392,-4.91690417492387,
5.43517694418905));
#23261=CARTESIAN_POINT('Ctrl Pts',(-0.0495503678360604,-4.91868364291584,
5.4197290236926));
#23262=CARTESIAN_POINT('Ctrl Pts',(-0.131531119113077,-4.91717436244273,
5.41503858489698));
#23263=CARTESIAN_POINT('Ctrl Pts',(-0.270156107836289,-4.9111528147168,
5.40712050533713));
#23264=CARTESIAN_POINT('Ctrl Pts',(-0.32682969755795,-4.90770707659288,
5.40388719174384));
#23265=CARTESIAN_POINT('Ctrl Pts',(-0.420143768930545,-4.90041001544262,
5.3985741293536));
#23266=CARTESIAN_POINT('Ctrl Pts',(-0.456822753742693,-4.89712692427873,
5.3964888308824));
#23267=CARTESIAN_POINT('Ctrl Pts',(-0.557681358024918,-4.88695617358912,
5.39076123885311));
#23268=CARTESIAN_POINT('Ctrl Pts',(-0.621767717142504,-4.87921655581746,
5.38712821212504));
#23269=CARTESIAN_POINT('Ctrl Pts',(-0.852372888648902,-4.84674938224515,
5.3740453911183));
#23270=CARTESIAN_POINT('Ctrl Pts',(-1.01774780099616,-4.81473872079946,
5.36464096454729));
#23271=CARTESIAN_POINT('Ctrl Pts',(-1.25828433468656,-4.75523043837684,
5.35073905539647));
#23272=CARTESIAN_POINT('Ctrl Pts',(-1.33493872436339,-4.73428288495452,
5.34627529266875));
#23273=CARTESIAN_POINT('Ctrl Pts',(-1.48082615357229,-4.69059081057421,
5.33769700630783));
#23274=CARTESIAN_POINT('Ctrl Pts',(-1.5501274412763,-4.66814663470203,5.33358544960583));
#23275=CARTESIAN_POINT('Ctrl Pts',(-1.67803223408347,-4.62356051569849,
5.32591861432572));
#23276=CARTESIAN_POINT('Ctrl Pts',(-1.73676087486603,-4.60182198450657,
5.32236694929157));
#23277=CARTESIAN_POINT('Ctrl Pts',(-1.98973951303468,-4.50264869695589,
5.30692128446282));
#23278=CARTESIAN_POINT('Ctrl Pts',(-2.1793533330118,-4.41399199375302,5.29495455365991));
#23279=CARTESIAN_POINT('Ctrl Pts',(-2.45571894078246,-4.26261249228675,
5.27692106358769));
#23280=CARTESIAN_POINT('Ctrl Pts',(-2.54702315555395,-4.20869269993568,
5.27086110702291));
#23281=CARTESIAN_POINT('Ctrl Pts',(-2.66962319805726,-4.13083929628305,
5.26260058795375));
#23282=CARTESIAN_POINT('Ctrl Pts',(-2.70247982285064,-4.10941895908117,
5.26037432882795));
#23283=CARTESIAN_POINT('Ctrl Pts',(-2.77294206864005,-4.06227165751999,
5.25557470930506));
#23284=CARTESIAN_POINT('Ctrl Pts',(-2.81045351558883,-4.03641051414627,
5.25300320723842));
#23285=CARTESIAN_POINT('Ctrl Pts',(-3.01141774141955,-3.89370195954318,
5.23911927566544));
#23286=CARTESIAN_POINT('Ctrl Pts',(-3.1679540036146,-3.76744219490056,5.22790741264078));
#23287=CARTESIAN_POINT('Ctrl Pts',(-3.37559018148979,-3.57785045328687,
5.21213385307693));
#23288=CARTESIAN_POINT('Ctrl Pts',(-3.43351761384499,-3.52229748541702,
5.20762591614298));
#23289=CARTESIAN_POINT('Ctrl Pts',(-3.54164927052531,-3.41339487964103,
5.19898207847478));
#23290=CARTESIAN_POINT('Ctrl Pts',(-3.59207193289128,-3.36029213380412,
5.1948492909109));
#23291=CARTESIAN_POINT('Ctrl Pts',(-3.68889407500936,-3.25365313396146,
5.18669727590681));
#23292=CARTESIAN_POINT('Ctrl Pts',(-3.73535990842118,-3.20020068316858,
5.18267973170018));
#23293=CARTESIAN_POINT('Ctrl Pts',(-3.90128992947281,-3.00078198566881,
5.16792644371664));
#23294=CARTESIAN_POINT('Ctrl Pts',(-4.01348390176428,-2.84898242511502,
5.15713686155798));
#23295=CARTESIAN_POINT('Ctrl Pts',(-4.17698230674647,-2.5988741862028,5.14003303230848));
#23296=CARTESIAN_POINT('Ctrl Pts',(-4.23416626724637,-2.50462864429724,
5.133729251485));
#23297=CARTESIAN_POINT('Ctrl Pts',(-4.30892413618677,-2.37153067945724,
5.12503858646369));
#23298=CARTESIAN_POINT('Ctrl Pts',(-4.32923216383696,-2.33425232183811,
5.12262684278592));
#23299=CARTESIAN_POINT('Ctrl Pts',(-4.36835795724081,-2.2601638083154,5.11787984671498));
#23300=CARTESIAN_POINT('Ctrl Pts',(-4.38719929067779,-2.22336999060224,
5.11554451737087));
#23301=CARTESIAN_POINT('Ctrl Pts',(-4.46893765753467,-2.05866366845608,
5.10517712080673));
#23302=CARTESIAN_POINT('Ctrl Pts',(-4.52672095034548,-1.92828893970501,
5.09719900934306));
#23303=CARTESIAN_POINT('Ctrl Pts',(-4.63577440227729,-1.65020191606282,
5.08046496221209));
#23304=CARTESIAN_POINT('Ctrl Pts',(-4.68583090679651,-1.50218460391411,
5.07171637600747));
#23305=CARTESIAN_POINT('Ctrl Pts',(-4.7484018406608,-1.28334248875194,5.05889066980605));
#23306=CARTESIAN_POINT('Ctrl Pts',(-4.7665438287729,-1.21422722656571,5.05485599977968));
#23307=CARTESIAN_POINT('Ctrl Pts',(-4.79795523529087,-1.08297823763899,
5.04721496956757));
#23308=CARTESIAN_POINT('Ctrl Pts',(-4.81153912878306,-1.02093457364158,
5.04361158263338));
#23309=CARTESIAN_POINT('Ctrl Pts',(-4.85218229897371,-0.816417616264684,
5.0317546831821));
#23310=CARTESIAN_POINT('Ctrl Pts',(-4.87414263729166,-0.673010697956814,
5.02347185655213));
#23311=CARTESIAN_POINT('Ctrl Pts',(-4.90155054759469,-0.419595530929521,
5.00888389166927));
#23312=CARTESIAN_POINT('Ctrl Pts',(-4.90970167726523,-0.309980230833086,
5.00259032852891));
#23313=CARTESIAN_POINT('Ctrl Pts',(-4.91689127836406,-0.133487742381665,
4.99250027109077));
#23314=CARTESIAN_POINT('Ctrl Pts',(-4.91825013655806,-0.0667425821893914,
4.9886945698553));
#23315=CARTESIAN_POINT('Ctrl Pts',(-4.91824992449483,0.0369214290317507,
4.98280585634637));
#23316=CARTESIAN_POINT('Ctrl Pts',(-4.91783432300853,0.0738317761361386,
4.98071375598035));
#23317=CARTESIAN_POINT('Ctrl Pts',(-4.91575794422724,0.166030384660693,
4.9754991923389));
#23318=CARTESIAN_POINT('Ctrl Pts',(-4.91357994119894,0.221301879863546,
4.97238242118607));
#23319=CARTESIAN_POINT('Ctrl Pts',(-4.90183918475955,0.429791417210259,
4.96063870870852));
#23320=CARTESIAN_POINT('Ctrl Pts',(-4.88603729618649,0.58257034637313,4.9520572789805));
#23321=CARTESIAN_POINT('Ctrl Pts',(-4.84452369037121,0.857483701056971,
4.93647307377018));
#23322=CARTESIAN_POINT('Ctrl Pts',(-4.82126240423902,0.979855279510011,
4.92948446112467));
#23323=CARTESIAN_POINT('Ctrl Pts',(-4.78410853719335,1.14157970064753,4.92012878523927));
#23324=CARTESIAN_POINT('Ctrl Pts',(-4.77432503429674,1.18182866914119,4.91779052029596));
#23325=CARTESIAN_POINT('Ctrl Pts',(-4.76403458685474,1.2219482467567,4.91544887818065));
#23326=CARTESIAN_POINT('',(-4.91824999923043,8.70047197037183E-5,4.63985943599073));
#23327=CARTESIAN_POINT('Ctrl Pts',(-4.76403458704967,1.22194824599672,4.56992379268636));
#23328=CARTESIAN_POINT('Ctrl Pts',(-4.7899691695387,1.12083655948854,4.5758358124286));
#23329=CARTESIAN_POINT('Ctrl Pts',(-4.81268096566489,1.01890921653989,4.58174783217083));
#23330=CARTESIAN_POINT('Ctrl Pts',(-4.83212549536711,0.916376701757057,
4.58765985191307));
#23331=CARTESIAN_POINT('Ctrl Pts',(-4.86073941546255,0.765493279524208,
4.59635978259268));
#23332=CARTESIAN_POINT('Ctrl Pts',(-4.88228416449266,0.613254030957627,
4.60505971327229));
#23333=CARTESIAN_POINT('Ctrl Pts',(-4.89666114209985,0.460318066068917,
4.6137596439519));
#23334=CARTESIAN_POINT('Ctrl Pts',(-4.91103811970703,0.307382101180202,
4.62245957463151));
#23335=CARTESIAN_POINT('Ctrl Pts',(-4.91824728090875,0.153749768058952,
4.63115950531112));
#23336=CARTESIAN_POINT('Ctrl Pts',(-4.91824999923044,8.70047197037183E-5,
4.63985943599073));
#23337=CARTESIAN_POINT('Ctrl Pts',(-4.91824999940249,7.66643645414756E-5,
4.6396755826554));
#23338=CARTESIAN_POINT('Ctrl Pts',(-4.91825071781255,-0.0460115057582501,
4.64226769254208));
#23339=CARTESIAN_POINT('Ctrl Pts',(-4.91760360853023,-0.0920972119024113,
4.64486297114107));
#23340=CARTESIAN_POINT('Ctrl Pts',(-4.91513167264574,-0.180054659700487,
4.64982563246288));
#23341=CARTESIAN_POINT('Ctrl Pts',(-4.91341918181897,-0.221925555652266,
4.6521921095278));
#23342=CARTESIAN_POINT('Ctrl Pts',(-4.90752604377101,-0.331651055084946,
4.65840690394181));
#23343=CARTESIAN_POINT('Ctrl Pts',(-4.90247328448707,-0.399449432917536,
4.66226038693857));
#23344=CARTESIAN_POINT('Ctrl Pts',(-4.88504433863517,-0.582126852888477,
4.67268765266898));
#23345=CARTESIAN_POINT('Ctrl Pts',(-4.87002313522901,-0.696709393471204,
4.67927629797717));
#23346=CARTESIAN_POINT('Ctrl Pts',(-4.82207872142587,-0.983609958476236,
4.69590673758689));
#23347=CARTESIAN_POINT('Ctrl Pts',(-4.7839469969302,-1.1548952765937,4.70596106603709));
#23348=CARTESIAN_POINT('Ctrl Pts',(-4.7246500966436,-1.3670717952216,4.71852538957432));
#23349=CARTESIAN_POINT('Ctrl Pts',(-4.71195765278293,-1.4101981998542,4.72108466930329));
#23350=CARTESIAN_POINT('Ctrl Pts',(-4.68834946590333,-1.4865341664381,4.7256221620174));
#23351=CARTESIAN_POINT('Ctrl Pts',(-4.67766761054332,-1.5198125891021,4.7276025475386));
#23352=CARTESIAN_POINT('Ctrl Pts',(-4.64903737890213,-1.60584537822008,
4.73272887479813));
#23353=CARTESIAN_POINT('Ctrl Pts',(-4.63054556330881,-1.65841364638349,
4.73586845427189));
#23354=CARTESIAN_POINT('Ctrl Pts',(-4.55355196671715,-1.86595389466506,
4.74831616700343));
#23355=CARTESIAN_POINT('Ctrl Pts',(-4.4881308045679,-2.01824230508286,4.75757113487215));
#23356=CARTESIAN_POINT('Ctrl Pts',(-4.37723969986203,-2.24418348030965,
4.77168352834208));
#23357=CARTESIAN_POINT('Ctrl Pts',(-4.33730848835138,-2.32041844946865,
4.77651383217334));
#23358=CARTESIAN_POINT('Ctrl Pts',(-4.26419444525155,-2.45151645150938,
4.78496384469718));
#23359=CARTESIAN_POINT('Ctrl Pts',(-4.23190066204659,-2.5068513833749,4.78857669519219));
#23360=CARTESIAN_POINT('Ctrl Pts',(-4.18390422587973,-2.58552077411517,
4.79378586781187));
#23361=CARTESIAN_POINT('Ctrl Pts',(-4.16906790196309,-2.6093763744932,4.79537532196427));
#23362=CARTESIAN_POINT('Ctrl Pts',(-4.11403149678931,-2.69620272713746,
4.80119750447677));
#23363=CARTESIAN_POINT('Ctrl Pts',(-4.07260276090377,-2.75838193053204,
4.80543921980069));
#23364=CARTESIAN_POINT('Ctrl Pts',(-3.9387313186842,-2.9497115712902,4.8187307104834));
#23365=CARTESIAN_POINT('Ctrl Pts',(-3.84144067351982,-3.07534311320507,
4.82781280115858));
#23366=CARTESIAN_POINT('Ctrl Pts',(-3.67901062875269,-3.26532886799321,
4.84212180059315));
#23367=CARTESIAN_POINT('Ctrl Pts',(-3.61786181878908,-3.33295181803246,
4.8473392476154));
#23368=CARTESIAN_POINT('Ctrl Pts',(-3.53468664292533,-3.41994536603993,
4.85421019418093));
#23369=CARTESIAN_POINT('Ctrl Pts',(-3.51431664932619,-3.4408740852958,4.85587583997594));
#23370=CARTESIAN_POINT('Ctrl Pts',(-3.46263853165682,-3.4930320349338,4.86005815932614));
#23371=CARTESIAN_POINT('Ctrl Pts',(-3.43109321637514,-3.5240229565949,4.86257193940952));
#23372=CARTESIAN_POINT('Ctrl Pts',(-3.39690004892525,-3.55672077546072,
4.86525391644256));
#23373=CARTESIAN_POINT('Ctrl Pts',(-3.39466404110137,-3.55885496544315,
4.86542910701477));
#23374=CARTESIAN_POINT('Ctrl Pts',(-3.36263357931177,-3.58936924999506,
4.86793591686767));
#23375=CARTESIAN_POINT('Ctrl Pts',(-3.33248593662625,-3.61737663601108,
4.8702609802002));
#23376=CARTESIAN_POINT('Ctrl Pts',(-3.22957562173448,-3.71060259262217,
4.87809127466346));
#23377=CARTESIAN_POINT('Ctrl Pts',(-3.1552214855713,-3.77403074327478,4.88357339091479));
#23378=CARTESIAN_POINT('Ctrl Pts',(-2.97216872199697,-3.92099152762595,
4.8967310516798));
#23379=CARTESIAN_POINT('Ctrl Pts',(-2.86177226081297,-4.00227695857349,
4.90439661345062));
#23380=CARTESIAN_POINT('Ctrl Pts',(-2.68708794782346,-4.11997066981224,
4.91622341307867));
#23381=CARTESIAN_POINT('Ctrl Pts',(-2.62513469412078,-4.15971966118694,
4.92036232552669));
#23382=CARTESIAN_POINT('Ctrl Pts',(-2.50716278720296,-4.23172452798077,
4.9281542972376));
#23383=CARTESIAN_POINT('Ctrl Pts',(-2.45135479397978,-4.26429563712494,
4.93180417842555));
#23384=CARTESIAN_POINT('Ctrl Pts',(-2.3410197219222,-4.32580838709126,4.93895711942695));
#23385=CARTESIAN_POINT('Ctrl Pts',(-2.28655727348435,-4.35484181949582,
4.94245877855016));
#23386=CARTESIAN_POINT('Ctrl Pts',(-2.0378694492351,-4.48146344043974,4.95832699843909));
#23387=CARTESIAN_POINT('Ctrl Pts',(-1.83785299614449,-4.56713481157362,
4.97077268987212));
#23388=CARTESIAN_POINT('Ctrl Pts',(-1.56955648417159,-4.66156359033867,
4.98704581548869));
#23389=CARTESIAN_POINT('Ctrl Pts',(-1.50583270558919,-4.68253677257851,
4.99087984154093));
#23390=CARTESIAN_POINT('Ctrl Pts',(-1.43368427021741,-4.70465756038691,
4.99518223531445));
#23391=CARTESIAN_POINT('Ctrl Pts',(-1.42566267161582,-4.70709457035336,
4.99566005051411));
#23392=CARTESIAN_POINT('Ctrl Pts',(-1.41249136114473,-4.71105933629108,
4.99644372672864));
#23393=CARTESIAN_POINT('Ctrl Pts',(-1.4073453130967,-4.71259918571027,4.99674968823818));
#23394=CARTESIAN_POINT('Ctrl Pts',(-1.39879911059558,-4.71514121485024,
4.9972574364198));
#23395=CARTESIAN_POINT('Ctrl Pts',(-1.395400378983,-4.71614815396453,4.99745926488267));
#23396=CARTESIAN_POINT('Ctrl Pts',(-1.38969267172222,-4.71783246108092,
4.99779804368089));
#23397=CARTESIAN_POINT('Ctrl Pts',(-1.38738428315576,-4.7185118102563,4.99793501203151));
#23398=CARTESIAN_POINT('Ctrl Pts',(-1.38089203534353,-4.72041727575545,
4.99832010230251));
#23399=CARTESIAN_POINT('Ctrl Pts',(-1.37670704092632,-4.72163952394104,
4.99856818800653));
#23400=CARTESIAN_POINT('Ctrl Pts',(-1.3688244946898,-4.72393028936543,4.99903518132851));
#23401=CARTESIAN_POINT('Ctrl Pts',(-1.3651273035362,-4.72500003399201,4.99925410068527));
#23402=CARTESIAN_POINT('Ctrl Pts',(-1.35807678337894,-4.72703106418668,
4.9996713540575));
#23403=CARTESIAN_POINT('Ctrl Pts',(-1.35472368022259,-4.72799312410791,
4.99986969572102));
#23404=CARTESIAN_POINT('Ctrl Pts',(-1.34823293533339,-4.72984795277611,
5.00025344583448));
#23405=CARTESIAN_POINT('Ctrl Pts',(-1.34509542348376,-4.73074116878585,
5.000438858813));
#23406=CARTESIAN_POINT('Ctrl Pts',(-1.33890756389329,-4.73249613259774,
5.0008043650079));
#23407=CARTESIAN_POINT('Ctrl Pts',(-1.33585726716918,-4.73335805443423,
5.00098445999174));
#23408=CARTESIAN_POINT('Ctrl Pts',(-1.32969142877049,-4.73509389949874,
5.00134833791924));
#23409=CARTESIAN_POINT('Ctrl Pts',(-1.32657585346998,-4.73596769814061,
5.00153211942631));
#23410=CARTESIAN_POINT('Ctrl Pts',(-1.28961658288973,-4.74629401504445,
5.00371126213087));
#23411=CARTESIAN_POINT('Ctrl Pts',(-1.25567331122557,-4.75538667006777,
5.00570228083981));
#23412=CARTESIAN_POINT('Ctrl Pts',(-1.16715127983303,-4.77808587448706,
5.0108687434756));
#23413=CARTESIAN_POINT('Ctrl Pts',(-1.11243134855468,-4.79112130282467,
5.01403768488064));
#23414=CARTESIAN_POINT('Ctrl Pts',(-0.895501291952956,-4.8388816873854,
5.02652748216524));
#23415=CARTESIAN_POINT('Ctrl Pts',(-0.73180162460796,-4.86632978590451,
5.03579563421216));
#23416=CARTESIAN_POINT('Ctrl Pts',(-0.482008635444411,-4.89532188683373,
5.04989636080355));
#23417=CARTESIAN_POINT('Ctrl Pts',(-0.396746889515972,-4.902968532215,5.05470134201408));
#23418=CARTESIAN_POINT('Ctrl Pts',(-0.247456298998478,-4.91243775123713,
5.06312259905793));
#23419=CARTESIAN_POINT('Ctrl Pts',(-0.183510403218548,-4.91524191719394,
5.06673213793642));
#23420=CARTESIAN_POINT('Ctrl Pts',(-0.0938489923399746,-4.91742160620816,
5.07180208835004));
#23421=CARTESIAN_POINT('Ctrl Pts',(-0.0681651160506288,-4.91784469011154,
5.07325540017648));
#23422=CARTESIAN_POINT('Ctrl Pts',(-0.0323896412794005,-4.9181536962559,
5.07528141278941));
#23423=CARTESIAN_POINT('Ctrl Pts',(-0.0222998710602266,-4.91820979464608,
5.07585299470894));
#23424=CARTESIAN_POINT('Ctrl Pts',(-0.00261464561696009,-4.91825866519176,
5.07696853707053));
#23425=CARTESIAN_POINT('Ctrl Pts',(0.00698075873364639,-4.91825440605936,
5.07751247593772));
#23426=CARTESIAN_POINT('Ctrl Pts',(0.0986877221735663,-4.91794532244331,
5.08271287886767));
#23427=CARTESIAN_POINT('Ctrl Pts',(0.180778817291399,-4.9156122966194,5.08738183166554));
#23428=CARTESIAN_POINT('Ctrl Pts',(0.4513360896731,-4.90113628722826,5.10282702063363));
#23429=CARTESIAN_POINT('Ctrl Pts',(0.639161405255672,-4.88019598024818,
5.11364713404883));
#23430=CARTESIAN_POINT('Ctrl Pts',(0.885087952496398,-4.83833429676218,
5.12791391497391));
#23431=CARTESIAN_POINT('Ctrl Pts',(0.944668490681234,-4.82705510415669,
5.13137747692948));
#23432=CARTESIAN_POINT('Ctrl Pts',(1.00726319369671,-4.81400195880645,5.13502102479273));
#23433=CARTESIAN_POINT('Ctrl Pts',(1.01050017046645,-4.81332353018949,5.13520945784415));
#23434=CARTESIAN_POINT('Ctrl Pts',(1.01628031092397,-4.81210599949933,5.13554595805206));
#23435=CARTESIAN_POINT('Ctrl Pts',(1.01882373561556,-4.81156814526674,5.13569403552057));
#23436=CARTESIAN_POINT('Ctrl Pts',(1.02338269366746,-4.81060029227805,5.13595947048108));
#23437=CARTESIAN_POINT('Ctrl Pts',(1.02539838513513,-4.81017104285608,5.13607683433701));
#23438=CARTESIAN_POINT('Ctrl Pts',(1.02902418418433,-4.80939653205173,5.13628795530469));
#23439=CARTESIAN_POINT('Ctrl Pts',(1.0306343890886,-4.80905172879,5.13638171639048));
#23440=CARTESIAN_POINT('Ctrl Pts',(1.03354011673042,-4.80842798072262,5.13655092012238));
#23441=CARTESIAN_POINT('Ctrl Pts',(1.03483570033424,-4.80814932089286,5.13662636528204));
#23442=CARTESIAN_POINT('Ctrl Pts',(1.03718039063906,-4.80764402298699,5.13676290598655));
#23443=CARTESIAN_POINT('Ctrl Pts',(1.0382295359943,-4.80741756508404,5.13682400314211));
#23444=CARTESIAN_POINT('Ctrl Pts',(1.04013304765276,-4.80700604013264,5.13693485664496));
#23445=CARTESIAN_POINT('Ctrl Pts',(1.04098743884944,-4.80682108870813,5.13698461403702));
#23446=CARTESIAN_POINT('Ctrl Pts',(1.04405923631298,-4.80615527440475,5.13716350990187));
#23447=CARTESIAN_POINT('Ctrl Pts',(1.04627635974414,-4.80567310474473,5.13729263642487));
#23448=CARTESIAN_POINT('Ctrl Pts',(1.0505489610052,-4.80474082241846,5.13754148504364));
#23449=CARTESIAN_POINT('Ctrl Pts',(1.05260448511337,-4.80429092458072,5.13766120911544));
#23450=CARTESIAN_POINT('Ctrl Pts',(1.05657597640264,-4.80341900292049,5.13789253703513));
#23451=CARTESIAN_POINT('Ctrl Pts',(1.05849198095969,-4.80299715154796,5.13800414250044));
#23452=CARTESIAN_POINT('Ctrl Pts',(1.06220404748173,-4.80217752775453,5.1382203738823));
#23453=CARTESIAN_POINT('Ctrl Pts',(1.06400013964827,-4.80177989389245,5.13832500112196));
#23454=CARTESIAN_POINT('Ctrl Pts',(1.06748995303853,-4.80100523572899,5.13852829820184));
#23455=CARTESIAN_POINT('Ctrl Pts',(1.06918369862117,-4.80062832262004,5.13862696912131));
#23456=CARTESIAN_POINT('Ctrl Pts',(1.07248473522235,-4.79989190168304,5.13881927964687));
#23457=CARTESIAN_POINT('Ctrl Pts',(1.07409204577864,-4.79953248268261,5.13891292012755));
#23458=CARTESIAN_POINT('Ctrl Pts',(1.07723483160756,-4.79882805034599,5.13909602058514));
#23459=CARTESIAN_POINT('Ctrl Pts',(1.07877032239213,-4.79848310726887,5.13918548126315));
#23460=CARTESIAN_POINT('Ctrl Pts',(1.08178313477067,-4.79780476941849,5.13936101762581));
#23461=CARTESIAN_POINT('Ctrl Pts',(1.08326046843861,-4.79747142916449,5.13944709386107));
#23462=CARTESIAN_POINT('Ctrl Pts',(1.08617002588369,-4.79681351461398,5.13961662168773));
#23463=CARTESIAN_POINT('Ctrl Pts',(1.08760225871064,-4.79648898111538,5.13970007369524));
#23464=CARTESIAN_POINT('Ctrl Pts',(1.09043443677156,-4.79584589649442,5.13986509976984));
#23465=CARTESIAN_POINT('Ctrl Pts',(1.0918343882915,-4.79552737374796,5.13994667412805));
#23466=CARTESIAN_POINT('Ctrl Pts',(1.09461501092848,-4.79489343427869,5.1401087025234));
#23467=CARTESIAN_POINT('Ctrl Pts',(1.09599568567718,-4.79457803411498,5.14018915672955));
#23468=CARTESIAN_POINT('Ctrl Pts',(1.13367760426103,-4.78595288154341,5.14238498530579));
#23469=CARTESIAN_POINT('Ctrl Pts',(1.16988357743715,-4.77723166266297,5.14449556909737));
#23470=CARTESIAN_POINT('Ctrl Pts',(1.25974105184251,-4.7545041629124,5.14973599144898));
#23471=CARTESIAN_POINT('Ctrl Pts',(1.31326132928385,-4.74000022571797,5.1528601936069));
#23472=CARTESIAN_POINT('Ctrl Pts',(1.54146534651177,-4.67399528431897,5.16621915149373));
#23473=CARTESIAN_POINT('Ctrl Pts',(1.71346086340778,-4.61371867093199,5.17638821372312));
#23474=CARTESIAN_POINT('Ctrl Pts',(1.95580633422812,-4.51336184161958,5.19110366824187));
#23475=CARTESIAN_POINT('Ctrl Pts',(2.02913328782687,-4.48087396279234,5.19560854448105));
#23476=CARTESIAN_POINT('Ctrl Pts',(2.16806216442214,-4.41521099962841,5.20426403964951));
#23477=CARTESIAN_POINT('Ctrl Pts',(2.23377922410107,-4.38232950968985,5.20841161548671));
#23478=CARTESIAN_POINT('Ctrl Pts',(2.35468420283209,-4.31840835530656,5.21615269141199));
#23479=CARTESIAN_POINT('Ctrl Pts',(2.41005740370888,-4.28775134751623,5.21974253088625));
#23480=CARTESIAN_POINT('Ctrl Pts',(2.57395707292246,-4.19283113526673,5.23050946215255));
#23481=CARTESIAN_POINT('Ctrl Pts',(2.68061839692196,-4.12545419101313,5.23770702656021));
#23482=CARTESIAN_POINT('Ctrl Pts',(2.91265791253478,-3.96607530909511,5.25381004483454));
#23483=CARTESIAN_POINT('Ctrl Pts',(3.03650381417749,-3.87207623235681,5.26271618314803));
#23484=CARTESIAN_POINT('Ctrl Pts',(3.17561059536704,-3.75570962719337,5.27306148475141));
#23485=CARTESIAN_POINT('Ctrl Pts',(3.19539708421455,-3.73888953312831,5.27454140320438));
#23486=CARTESIAN_POINT('Ctrl Pts',(3.24670150437148,-3.69457193901863,5.27840014716026));
#23487=CARTESIAN_POINT('Ctrl Pts',(3.2780037186468,-3.66682753208075,5.28077594915888));
#23488=CARTESIAN_POINT('Ctrl Pts',(3.34068355524541,-3.6098277546292,5.28557491134537));
#23489=CARTESIAN_POINT('Ctrl Pts',(3.37203999243243,-3.58055434001805,5.2879976011686));
#23490=CARTESIAN_POINT('Ctrl Pts',(3.48130004655076,-3.47584406399227,5.29652756602882));
#23491=CARTESIAN_POINT('Ctrl Pts',(3.55708834601077,-3.39824438951752,5.30260671780489));
#23492=CARTESIAN_POINT('Ctrl Pts',(3.73884696280387,-3.19939297347475,5.31770203876384));
#23493=CARTESIAN_POINT('Ctrl Pts',(3.84154508238719,-3.07532483653806,5.32670753791862));
#23494=CARTESIAN_POINT('Ctrl Pts',(3.98561326815726,-2.88277528455182,5.34023716497286));
#23495=CARTESIAN_POINT('Ctrl Pts',(4.03170075523626,-2.81795941812591,5.34472059484519));
#23496=CARTESIAN_POINT('Ctrl Pts',(4.1148306763227,-2.69483185219806,5.35312150052658));
#23497=CARTESIAN_POINT('Ctrl Pts',(4.15225562799454,-2.6368017106891,5.35703475806465));
#23498=CARTESIAN_POINT('Ctrl Pts',(4.25046600992333,-2.47724067152091,5.36768004891839));
#23499=CARTESIAN_POINT('Ctrl Pts',(4.308828819861,-2.37427383837306,5.3744278731477));
#23500=CARTESIAN_POINT('Ctrl Pts',(4.42712611589811,-2.14681161624436,5.38908681390839));
#23501=CARTESIAN_POINT('Ctrl Pts',(4.48564489804156,-2.02169126567489,5.39699818174306));
#23502=CARTESIAN_POINT('Ctrl Pts',(4.55968528609232,-1.84428507603931,5.40798574030637));
#23503=CARTESIAN_POINT('Ctrl Pts',(4.57972144943016,-1.79395341777754,5.41107777825666));
#23504=CARTESIAN_POINT('Ctrl Pts',(4.6144770087273,-1.70226636429126,5.41666142455238));
#23505=CARTESIAN_POINT('Ctrl Pts',(4.62948204368616,-1.66102525762501,5.41915530481924));
#23506=CARTESIAN_POINT('Ctrl Pts',(4.65743884866577,-1.580863209721,5.42396619766399));
#23507=CARTESIAN_POINT('Ctrl Pts',(4.67045962077837,-1.54197019729098,5.42628372901171));
#23508=CARTESIAN_POINT('Ctrl Pts',(4.71568777733272,-1.4010423317161,5.4346302823018));
#23509=CARTESIAN_POINT('Ctrl Pts',(4.74505030614714,-1.29812514640594,5.44063049662655));
#23510=CARTESIAN_POINT('Ctrl Pts',(4.7963620268681,-1.09314861159687,5.45247161324059));
#23511=CARTESIAN_POINT('Ctrl Pts',(4.81846585141105,-0.99118583831548,5.45830969925278));
#23512=CARTESIAN_POINT('Ctrl Pts',(4.85198060683616,-0.808739615205265,
5.46871529811053));
#23513=CARTESIAN_POINT('Ctrl Pts',(4.86467038157827,-0.728531048966778,
5.47327596689699));
#23514=CARTESIAN_POINT('Ctrl Pts',(4.88511342376834,-0.574734224607493,
5.48201409882638));
#23515=CARTESIAN_POINT('Ctrl Pts',(4.89320325069664,-0.50121289902779,5.48618833122787));
#23516=CARTESIAN_POINT('Ctrl Pts',(4.9058501854067,-0.356277557477541,5.49442239896876));
#23517=CARTESIAN_POINT('Ctrl Pts',(4.9105128869947,-0.284890797760436,5.49848050589524));
#23518=CARTESIAN_POINT('Ctrl Pts',(4.9229129325575,0.000587095606161998,
5.51473161378684));
#23519=CARTESIAN_POINT('Ctrl Pts',(4.91821652440404,0.214979093078194,5.5269979173557));
#23520=CARTESIAN_POINT('Ctrl Pts',(4.89370727608886,0.495303515500945,5.54309748253594));
#23521=CARTESIAN_POINT('Ctrl Pts',(4.88648504658181,0.562103608129633,5.54693742137544));
#23522=CARTESIAN_POINT('Ctrl Pts',(4.87145426625354,0.678716462703673,5.5536409194428));
#23523=CARTESIAN_POINT('Ctrl Pts',(4.86424405457737,0.728596297980341,5.55650827510348));
#23524=CARTESIAN_POINT('Ctrl Pts',(4.85030985991866,0.815533526851358,5.56150253721946));
#23525=CARTESIAN_POINT('Ctrl Pts',(4.84392455036782,0.852640397463089,5.56363271592947));
#23526=CARTESIAN_POINT('Ctrl Pts',(4.82614043672559,0.949332100474078,5.56918331031746));
#23527=CARTESIAN_POINT('Ctrl Pts',(4.81406420978863,1.00878583318358,5.57259652492391));
#23528=CARTESIAN_POINT('Ctrl Pts',(4.76411064517863,1.23333762715918,5.5855173980748));
#23529=CARTESIAN_POINT('Ctrl Pts',(4.7188136608917,1.39666386279084,5.59497979383111));
#23530=CARTESIAN_POINT('Ctrl Pts',(4.64031036490253,1.63183090218435,5.608891116679));
#23531=CARTESIAN_POINT('Ctrl Pts',(4.61365867496534,1.70572736751597,5.61330459176182));
#23532=CARTESIAN_POINT('Ctrl Pts',(4.55895610372849,1.84672314208421,5.62182493991813));
#23533=CARTESIAN_POINT('Ctrl Pts',(4.53116424692069,1.91390112715617,5.62592907411136));
#23534=CARTESIAN_POINT('Ctrl Pts',(4.47265493035265,2.04690339705705,5.63415495995136));
#23535=CARTESIAN_POINT('Ctrl Pts',(4.44194784495269,2.11271266842417,5.63827567657888));
#23536=CARTESIAN_POINT('Ctrl Pts',(4.33713186559064,2.32495131161454,5.65174215485226));
#23537=CARTESIAN_POINT('Ctrl Pts',(4.25715104676581,2.46835475091049,5.66112474415458));
#23538=CARTESIAN_POINT('Ctrl Pts',(4.10067057170046,2.71861367363788,5.67802108823279));
#23539=CARTESIAN_POINT('Ctrl Pts',(4.02677312587739,2.82691673024172,5.68552307983263));
#23540=CARTESIAN_POINT('Ctrl Pts',(3.92357405645862,2.96589229976798,5.69537615993432));
#23541=CARTESIAN_POINT('Ctrl Pts',(3.89807827817353,2.99932264100133,5.69776430892468));
#23542=CARTESIAN_POINT('Ctrl Pts',(3.84585334320688,3.06600963986201,5.70256244686095));
#23543=CARTESIAN_POINT('Ctrl Pts',(3.81911375722526,3.09925365464379,5.70497207875724));
#23544=CARTESIAN_POINT('Ctrl Pts',(3.71223769261212,3.22864358931082,5.71443192605509));
#23545=CARTESIAN_POINT('Ctrl Pts',(3.62887521221341,3.32206463822661,5.72144275414572));
#23546=CARTESIAN_POINT('Ctrl Pts',(3.4301198367567,3.52838266886259,5.73749204838565));
#23547=CARTESIAN_POINT('Ctrl Pts',(3.31255324410316,3.63898291012171,5.74652306265818));
#23548=CARTESIAN_POINT('Ctrl Pts',(3.13313603445137,3.79185664243156,5.75979728255143));
#23549=CARTESIAN_POINT('Ctrl Pts',(3.07541928292658,3.83881677989051,5.76399605292956));
#23550=CARTESIAN_POINT('Ctrl Pts',(2.9604104713672,3.92813252631501,5.77223683623686));
#23551=CARTESIAN_POINT('Ctrl Pts',(2.90321920843041,3.97058854243853,5.77627689576103));
#23552=CARTESIAN_POINT('Ctrl Pts',(2.69198906046289,4.12039123091393,5.79100296671283));
#23553=CARTESIAN_POINT('Ctrl Pts',(2.53276042401556,4.22013647686359,5.8017422662152));
#23554=CARTESIAN_POINT('Ctrl Pts',(2.29582635435419,4.35030892832668,5.81721703804273));
#23555=CARTESIAN_POINT('Ctrl Pts',(2.22243860698376,4.38825400235455,5.8219432578573));
#23556=CARTESIAN_POINT('Ctrl Pts',(2.12330064633558,4.43638808505068,5.82823226240219));
#23557=CARTESIAN_POINT('Ctrl Pts',(2.09837038633469,4.44823410001496,5.82980583840515));
#23558=CARTESIAN_POINT('Ctrl Pts',(2.03388954079763,4.47821049672092,5.83385475101351));
#23559=CARTESIAN_POINT('Ctrl Pts',(1.99419549028122,4.4960271710339,5.83632701749922));
#23560=CARTESIAN_POINT('Ctrl Pts',(1.92150771139633,4.52750105349003,5.84081527783571));
#23561=CARTESIAN_POINT('Ctrl Pts',(1.88859175906055,4.54133007726786,5.84283330581411));
#23562=CARTESIAN_POINT('Ctrl Pts',(1.69094306188053,4.62184793158595,5.8548745658535));
#23563=CARTESIAN_POINT('Ctrl Pts',(1.52284290624634,4.67992711911205,5.86480554975824));
#23564=CARTESIAN_POINT('Ctrl Pts',(1.24742190864058,4.75867047507026,5.88085779967603));
#23565=CARTESIAN_POINT('Ctrl Pts',(1.14191522597249,4.78508468191166,5.88695590495483));
#23566=CARTESIAN_POINT('Ctrl Pts',(0.960260456342191,4.82421242982289,5.89741471569399));
#23567=CARTESIAN_POINT('Ctrl Pts',(0.884529656508206,4.83867056237916,5.90176291363321));
#23568=CARTESIAN_POINT('Ctrl Pts',(0.740416114672127,4.86268752164608,5.91002737442573));
#23569=CARTESIAN_POINT('Ctrl Pts',(0.672110545568175,4.87259820078722,5.91394022762721));
#23570=CARTESIAN_POINT('Ctrl Pts',(0.384347508419882,4.90818455296475,5.93041967681783));
#23571=CARTESIAN_POINT('Ctrl Pts',(0.163499881675224,4.92049425296194,5.9430678768831));
#23572=CARTESIAN_POINT('Ctrl Pts',(-0.106809308814562,4.91733813536378,
5.95853572053028));
#23573=CARTESIAN_POINT('Ctrl Pts',(-0.15618595415305,4.91601754945549,5.96135998741251));
#23574=CARTESIAN_POINT('Ctrl Pts',(-0.267807488811053,4.91134878875579,
5.96773899379231));
#23575=CARTESIAN_POINT('Ctrl Pts',(-0.330025932074981,4.90756057482039,
5.97129078963232));
#23576=CARTESIAN_POINT('Ctrl Pts',(-0.4291627244893,4.8996306672596,5.97693843781409));
#23577=CARTESIAN_POINT('Ctrl Pts',(-0.466134766404531,4.89625160118804,
5.97904172325503));
#23578=CARTESIAN_POINT('Ctrl Pts',(-0.56298322292073,4.88629318028304,5.98454466314392));
#23579=CARTESIAN_POINT('Ctrl Pts',(-0.622783252270197,4.87903190233572,
5.98793681733293));
#23580=CARTESIAN_POINT('Ctrl Pts',(-0.856468986073093,4.84628994653024,
6.00119949172932));
#23581=CARTESIAN_POINT('Ctrl Pts',(-1.02907137683812,4.81259577104911,6.01101467141172));
#23582=CARTESIAN_POINT('Ctrl Pts',(-1.27697363917176,4.75025295472467,6.02535573714729));
#23583=CARTESIAN_POINT('Ctrl Pts',(-1.35396049165321,4.72888524251669,6.02984370265032));
#23584=CARTESIAN_POINT('Ctrl Pts',(-1.50055251039084,4.68432519472137,6.03847416766882));
#23585=CARTESIAN_POINT('Ctrl Pts',(-1.5702265023191,4.66143206880253,6.04261368065903));
#23586=CARTESIAN_POINT('Ctrl Pts',(-1.70726982245865,4.61298175562244,6.05084141680459));
#23587=CARTESIAN_POINT('Ctrl Pts',(-1.77464148875063,4.5874849697979,6.05492824434737));
#23588=CARTESIAN_POINT('Ctrl Pts',(-2.03190448665103,4.48360831109142,6.07070942973382));
#23589=CARTESIAN_POINT('Ctrl Pts',(-2.21737322889601,4.39484166271974,6.08246941738451));
#23590=CARTESIAN_POINT('Ctrl Pts',(-2.48480885623965,4.24559520460927,6.09999460791644));
#23591=CARTESIAN_POINT('Ctrl Pts',(-2.57134166005497,4.19375203665733,6.10575812723543));
#23592=CARTESIAN_POINT('Ctrl Pts',(-2.68924137135573,4.11809462524778,6.11372526748306));
#23593=CARTESIAN_POINT('Ctrl Pts',(-2.72200831559824,4.09650989141345,6.11595208378754));
#23594=CARTESIAN_POINT('Ctrl Pts',(-2.79342048699943,4.04823301884738,6.12083133500346));
#23595=CARTESIAN_POINT('Ctrl Pts',(-2.83194874426976,4.02137476166968,6.12348148806722));
#23596=CARTESIAN_POINT('Ctrl Pts',(-3.09993907534417,3.82879550972027,6.14206623140382));
#23597=CARTESIAN_POINT('Ctrl Pts',(-3.31510475331593,3.64408834780691,6.15780892499917));
#23598=CARTESIAN_POINT('Ctrl Pts',(-3.5641127845189,3.38992304519,6.17785458421856));
#23599=CARTESIAN_POINT('Ctrl Pts',(-3.61387695694162,3.33682054815876,6.1819629344182));
#23600=CARTESIAN_POINT('Ctrl Pts',(-3.7049673719628,3.23519070744461,6.18968905856347));
#23601=CARTESIAN_POINT('Ctrl Pts',(-3.74656434335059,3.18692605013148,6.19330349523909));
#23602=CARTESIAN_POINT('Ctrl Pts',(-3.91241054430925,2.98675994809304,6.20808313574593));
#23603=CARTESIAN_POINT('Ctrl Pts',(-4.02845213660913,2.82829677702066,6.21931023561548));
#23604=CARTESIAN_POINT('Ctrl Pts',(-4.17763573896722,2.59669500594495,6.23507898491558));
#23605=CARTESIAN_POINT('Ctrl Pts',(-4.21894014309601,2.52903331629471,6.23961309832852));
#23606=CARTESIAN_POINT('Ctrl Pts',(-4.27205226486006,2.43710412728897,6.24567073837196));
#23607=CARTESIAN_POINT('Ctrl Pts',(-4.28532167382844,2.41369535009285,6.24720451947806));
#23608=CARTESIAN_POINT('Ctrl Pts',(-4.31919595224799,2.35277725310244,6.25117276906155));
#23609=CARTESIAN_POINT('Ctrl Pts',(-4.33950466325037,2.3151055723415,6.25360418693083));
#23610=CARTESIAN_POINT('Ctrl Pts',(-4.37872693927959,2.24002019399494,6.25840360754624));
#23611=CARTESIAN_POINT('Ctrl Pts',(-4.39765898921972,2.20262015427534,6.26077162518407));
#23612=CARTESIAN_POINT('Ctrl Pts',(-4.47597181659911,2.0428783860973,6.27080172231748));
#23613=CARTESIAN_POINT('Ctrl Pts',(-4.53074358810137,1.91834281447384,6.2784154865502));
#23614=CARTESIAN_POINT('Ctrl Pts',(-4.62286227527088,1.68285105610479,6.29258130479891));
#23615=CARTESIAN_POINT('Ctrl Pts',(-4.66154638638726,1.57252291758111,6.2991273701076));
#23616=CARTESIAN_POINT('Ctrl Pts',(-4.70844494961317,1.42176335221978,6.30800104716982));
#23617=CARTESIAN_POINT('Ctrl Pts',(-4.72013626914036,1.38245377839685,6.31030826681332));
#23618=CARTESIAN_POINT('Ctrl Pts',(-4.74274893536813,1.3027904344289,6.314973309344));
#23619=CARTESIAN_POINT('Ctrl Pts',(-4.75364979408675,1.2624356505064,6.31733098714234));
#23620=CARTESIAN_POINT('Ctrl Pts',(-4.76403458747083,1.22194824435476,6.31969203503535));
#23621=CARTESIAN_POINT('Origin',(0.,0.,-3.23514056400928));
#23622=CARTESIAN_POINT('',(-4.76403458704967,1.22194824599671,8.41520471722259));
#23623=CARTESIAN_POINT('',(-4.76403458713635,1.22194824565879,8.07015829796832));
#23624=CARTESIAN_POINT('',(-4.76403458704967,1.22194824599672,-3.23514056400928));
#23625=CARTESIAN_POINT('',(-4.91824999926051,-8.5287480579431E-5,6.73514056400926));
#23626=CARTESIAN_POINT('Ctrl Pts',(-4.91824999926051,-8.5287480579431E-5,
6.73514056400926));
#23627=CARTESIAN_POINT('Ctrl Pts',(-4.9182473175325,-0.154731769320271,
6.74389616606202));
#23628=CARTESIAN_POINT('Ctrl Pts',(-4.91094555559967,-0.309347709470215,
6.75265176811478));
#23629=CARTESIAN_POINT('Ctrl Pts',(-4.89638425253901,-0.463254049078936,
6.76140737016754));
#23630=CARTESIAN_POINT('Ctrl Pts',(-4.88182294947835,-0.617160388687658,
6.7701629722203));
#23631=CARTESIAN_POINT('Ctrl Pts',(-4.86000215205804,-0.770356766869605,
6.77891857427307));
#23632=CARTESIAN_POINT('Ctrl Pts',(-4.83102301718729,-0.922171171695713,
6.78767417632583));
#23633=CARTESIAN_POINT('Ctrl Pts',(-4.80402699906593,-1.06359652624984,
6.79583061000592));
#23634=CARTESIAN_POINT('Ctrl Pts',(-4.77081145334733,-1.20386205789481,
6.80398704368602));
#23635=CARTESIAN_POINT('Ctrl Pts',(-4.73150086408182,-1.34241671462069,
6.81214347736611));
#23636=CARTESIAN_POINT('Ctrl Pts',(-4.69219827562945,-1.48094317156785,
6.820298250982));
#23637=CARTESIAN_POINT('Ctrl Pts',(-4.64680320966298,-1.61775912652929,
6.8284530245979));
#23638=CARTESIAN_POINT('Ctrl Pts',(-4.59549040688103,-1.75232730469067,
6.83660779821379));
#23639=CARTESIAN_POINT('Ctrl Pts',(-4.54417578438562,-1.88690025506309,
6.84476286102362));
#23640=CARTESIAN_POINT('Ctrl Pts',(-4.48694312085571,-2.01922495513687,
6.85291792383345));
#23641=CARTESIAN_POINT('Ctrl Pts',(-4.42401601323758,-2.14878230100619,
6.86107298664328));
#23642=CARTESIAN_POINT('Ctrl Pts',(-4.36109259628959,-2.27833204834689,
6.86922757115928));
#23643=CARTESIAN_POINT('Ctrl Pts',(-4.29247555048242,-2.40511446560006,
6.87738215567528));
#23644=CARTESIAN_POINT('Ctrl Pts',(-4.21843529101728,-2.52863337753814,
6.88553674019129));
#23645=CARTESIAN_POINT('Ctrl Pts',(-4.14437682765308,-2.65218265843794,
6.89369332963319));
#23646=CARTESIAN_POINT('Ctrl Pts',(-4.06489265817825,-2.7724665434294,6.90184991907509));
#23647=CARTESIAN_POINT('Ctrl Pts',(-3.98029786645074,-2.88901574187951,
6.91000650851699));
#23648=CARTESIAN_POINT('Ctrl Pts',(-3.92286118202748,-2.9681482675878,6.91554452621498));
#23649=CARTESIAN_POINT('Ctrl Pts',(-3.86306947491248,-3.04555970926984,
6.92108254391297));
#23650=CARTESIAN_POINT('Ctrl Pts',(-3.80103237900352,-3.12111132711841,
6.92662056161096));
#23651=CARTESIAN_POINT('Ctrl Pts',(-3.70966368246236,-3.23238431214869,
6.93477699529105));
#23652=CARTESIAN_POINT('Ctrl Pts',(-3.61338837694744,-3.33966318888148,
6.94293342897114));
#23653=CARTESIAN_POINT('Ctrl Pts',(-3.51257941745858,-3.4425236235277,6.95108986265124));
#23654=CARTESIAN_POINT('Ctrl Pts',(-3.41179097543487,-3.54536312317576,
6.95924463626714));
#23655=CARTESIAN_POINT('Ctrl Pts',(-3.30647095430475,-3.64378573589915,
6.96739940988304));
#23656=CARTESIAN_POINT('Ctrl Pts',(-3.19702984908185,-3.73740327053152,
6.97555418349894));
#23657=CARTESIAN_POINT('Ctrl Pts',(-3.08758486273307,-3.83102412513618,
6.98370924630877));
#23658=CARTESIAN_POINT('Ctrl Pts',(-2.97401875168829,-3.91983934031082,
6.9918643091186));
#23659=CARTESIAN_POINT('Ctrl Pts',(-2.85677621914406,-4.00350005573036,
7.00001937192843));
#23660=CARTESIAN_POINT('Ctrl Pts',(-2.73954056286551,-4.08715586445526,
7.00817395644444));
#23661=CARTESIAN_POINT('Ctrl Pts',(-2.61862918942034,-4.16565758463701,
7.01632854096045));
#23662=CARTESIAN_POINT('Ctrl Pts',(-2.49451694429524,-4.23869888965045,
7.02448312547646));
#23663=CARTESIAN_POINT('Ctrl Pts',(-2.37037418432866,-4.31175815295512,
7.03263971491836));
#23664=CARTESIAN_POINT('Ctrl Pts',(-2.24302926852906,-4.37935414844116,
7.04079630436027));
#23665=CARTESIAN_POINT('Ctrl Pts',(-2.11298340441212,-4.44122552852014,
7.04895289380217));
#23666=CARTESIAN_POINT('Ctrl Pts',(-2.02468714993508,-4.48323387040317,
7.05449091150014));
#23667=CARTESIAN_POINT('Ctrl Pts',(-1.9351463235655,-4.52260416321385,7.0600289291981));
#23668=CARTESIAN_POINT('Ctrl Pts',(-1.84452357534784,-4.55926702908329,
7.06556694689607));
#23669=CARTESIAN_POINT('Ctrl Pts',(-1.71105371734862,-4.61326437078482,
7.07372338057616));
#23670=CARTESIAN_POINT('Ctrl Pts',(-1.5751861762655,-4.66140690006042,7.08187981425625));
#23671=CARTESIAN_POINT('Ctrl Pts',(-1.43745146864538,-4.70350043454758,
7.09003624793634));
#23672=CARTESIAN_POINT('Ctrl Pts',(-1.29974479392128,-4.74558540181376,
7.09819102155223));
#23673=CARTESIAN_POINT('Ctrl Pts',(-1.16017203060442,-4.78162373260446,
7.10634579516812));
#23674=CARTESIAN_POINT('Ctrl Pts',(-1.01927936807949,-4.81147094268556,
7.11450056878401));
#23675=CARTESIAN_POINT('Ctrl Pts',(-0.878381709057261,-4.84131921124268,
7.12265563159384));
#23676=CARTESIAN_POINT('Ctrl Pts',(-0.736164383736719,-4.86497584673957,
7.13081069440368));
#23677=CARTESIAN_POINT('Ctrl Pts',(-0.593184803227397,-4.88234726865266,
7.13896575721351));
#23678=CARTESIAN_POINT('Ctrl Pts',(-0.450213608459839,-4.89971767173314,
7.14712034172952));
#23679=CARTESIAN_POINT('Ctrl Pts',(-0.306480580255943,-4.91080355930208,
7.15527492624552));
#23680=CARTESIAN_POINT('Ctrl Pts',(-0.16254924873632,-4.91556312178323,
7.16342951076152));
#23681=CARTESIAN_POINT('Ctrl Pts',(-0.0185825295579952,-4.9203238544736,
7.17158610020342));
#23682=CARTESIAN_POINT('Ctrl Pts',(0.125582255771689,-4.91875514271468,
7.17974268964532));
#23683=CARTESIAN_POINT('Ctrl Pts',(0.26937994759,-4.91086728657336,7.18789927908722));
#23684=CARTESIAN_POINT('Ctrl Pts',(0.367013176268963,-4.90551172868718,
7.19343729678522));
#23685=CARTESIAN_POINT('Ctrl Pts',(0.464477156232307,-4.89724419261147,
7.19897531448322));
#23686=CARTESIAN_POINT('Ctrl Pts',(0.561595867944282,-4.88608157357283,
7.20451333218122));
#23687=CARTESIAN_POINT('Ctrl Pts',(0.704633029320816,-4.86964118517939,
7.21266976586132));
#23688=CARTESIAN_POINT('Ctrl Pts',(0.846974502216946,-4.84691241621129,
7.22082619954141));
#23689=CARTESIAN_POINT('Ctrl Pts',(0.988061524253188,-4.81797856852752,
7.2289826332215));
#23690=CARTESIAN_POINT('Ctrl Pts',(1.12911983110287,-4.78905060969746,7.23713740683739));
#23691=CARTESIAN_POINT('Ctrl Pts',(1.26892386882529,-4.7539201587667,7.24529218045329));
#23692=CARTESIAN_POINT('Ctrl Pts',(1.40692488970152,-4.71272165709353,7.25344695406918));
#23693=CARTESIAN_POINT('Ctrl Pts',(1.54493080452828,-4.67152169439182,7.261602016879));
#23694=CARTESIAN_POINT('Ctrl Pts',(1.68113325285886,-4.62425334247315,7.26975707968883));
#23695=CARTESIAN_POINT('Ctrl Pts',(1.81499798705176,-4.57110111127484,7.27791214249866));
#23696=CARTESIAN_POINT('Ctrl Pts',(1.948854870088,-4.51795199745092,7.28606672701467));
#23697=CARTESIAN_POINT('Ctrl Pts',(2.0803740026185,-4.45891981912179,7.29422131153067));
#23698=CARTESIAN_POINT('Ctrl Pts',(2.20904053280529,-4.39423747502605,7.30237589604668));
#23699=CARTESIAN_POINT('Ctrl Pts',(2.33773869757232,-4.32953922781392,7.31053248548858));
#23700=CARTESIAN_POINT('Ctrl Pts',(2.46358255932365,-4.25918818912044,7.31868907493048));
#23701=CARTESIAN_POINT('Ctrl Pts',(2.58608076637406,-4.18346379598177,7.32684566437237));
#23702=CARTESIAN_POINT('Ctrl Pts',(2.66925244535202,-4.13204977884158,7.33238368207036));
#23703=CARTESIAN_POINT('Ctrl Pts',(2.75088231011637,-4.07815966173679,7.33792169976835));
#23704=CARTESIAN_POINT('Ctrl Pts',(2.83082387716705,-4.02189249470456,7.34345971746633));
#23705=CARTESIAN_POINT('Ctrl Pts',(2.94856241205253,-3.93902179235354,7.35161615114642));
#23706=CARTESIAN_POINT('Ctrl Pts',(3.06268146398457,-3.8509619613798,7.3597725848265));
#23707=CARTESIAN_POINT('Ctrl Pts',(3.17273022551003,-3.75805348267358,7.36792901850659));
#23708=CARTESIAN_POINT('Ctrl Pts',(3.28275658901019,-3.66516391346193,7.37608379212248));
#23709=CARTESIAN_POINT('Ctrl Pts',(3.38871405921516,-3.56742788093614,7.38423856573838));
#23710=CARTESIAN_POINT('Ctrl Pts',(3.49018508971363,-3.4652259813814,7.39239333935427));
#23711=CARTESIAN_POINT('Ctrl Pts',(3.59165971869407,-3.36302045742576,7.4005484021641));
#23712=CARTESIAN_POINT('Ctrl Pts',(3.68864735118197,-3.25634898434736,7.40870346497392));
#23713=CARTESIAN_POINT('Ctrl Pts',(3.78076712818884,-3.14562918744513,7.41685852778374));
#23714=CARTESIAN_POINT('Ctrl Pts',(3.8728815023777,-3.03491588425068,7.42501311229975));
#23715=CARTESIAN_POINT('Ctrl Pts',(3.96012837896673,-2.92015499010418,7.43316769681575));
#23716=CARTESIAN_POINT('Ctrl Pts',(4.04216708177416,-2.80179734197915,7.44132228133175));
#23717=CARTESIAN_POINT('Ctrl Pts',(4.12422595501689,-2.6834105938659,7.44947887077365));
#23718=CARTESIAN_POINT('Ctrl Pts',(4.2010739048446,-2.56142559973553,7.45763546021554));
#23719=CARTESIAN_POINT('Ctrl Pts',(4.27241315665875,-2.43632281960114,7.46579204965743));
#23720=CARTESIAN_POINT('Ctrl Pts',(4.32084982763793,-2.35138273338132,7.47133006735544));
#23721=CARTESIAN_POINT('Ctrl Pts',(4.36674794282232,-2.2650059855518,7.47686808505345));
#23722=CARTESIAN_POINT('Ctrl Pts',(4.41002626073745,-2.17734963708314,7.48240610275146));
#23723=CARTESIAN_POINT('Ctrl Pts',(4.47376688944432,-2.04824871471139,7.49056253643155));
#23724=CARTESIAN_POINT('Ctrl Pts',(4.5318465054285,-1.91632278832777,7.49871897011165));
#23725=CARTESIAN_POINT('Ctrl Pts',(4.58403214243955,-1.78208652415674,7.50687540379174));
#23726=CARTESIAN_POINT('Ctrl Pts',(4.63620715820228,-1.64787758084979,7.51503017740764));
#23727=CARTESIAN_POINT('Ctrl Pts',(4.68249046693005,-1.51135954951569,7.52318495102354));
#23728=CARTESIAN_POINT('Ctrl Pts',(4.72269750227204,-1.37306640936752,7.53133972463944));
#23729=CARTESIAN_POINT('Ctrl Pts',(4.76290596348202,-1.23476836490948,7.53949478744927));
#23730=CARTESIAN_POINT('Ctrl Pts',(4.7970376231031,-1.09469540593501,7.5476498502591));
#23731=CARTESIAN_POINT('Ctrl Pts',(4.82495784683387,-0.953396475122647,
7.55580491306893));
#23732=CARTESIAN_POINT('Ctrl Pts',(4.8528764330456,-0.812105831481982,7.56395949758493));
#23733=CARTESIAN_POINT('Ctrl Pts',(4.87458424826237,-0.669589688331877,
7.57211408210094));
#23734=CARTESIAN_POINT('Ctrl Pts',(4.88999783325884,-0.526406927408665,
7.58026866661694));
#23735=CARTESIAN_POINT('Ctrl Pts',(4.90541520791444,-0.383188962873989,
7.58842525605885));
#23736=CARTESIAN_POINT('Ctrl Pts',(4.91453522398999,-0.239304385894645,
7.59658184550075));
#23737=CARTESIAN_POINT('Ctrl Pts',(4.91732626782645,-0.0953175652439695,
7.60473843494265));
#23738=CARTESIAN_POINT('Ctrl Pts',(4.91922128170108,0.00244407480408897,
7.61027645264062));
#23739=CARTESIAN_POINT('Ctrl Pts',(4.91819978220986,0.100252745594403,7.6158144703386));
#23740=CARTESIAN_POINT('Ctrl Pts',(4.91426557286648,0.197931659517309,7.62135248803658));
#23741=CARTESIAN_POINT('Ctrl Pts',(4.90847124006675,0.341793890879735,7.62950892171667));
#23742=CARTESIAN_POINT('Ctrl Pts',(4.89635426123467,0.485428394634977,7.63766535539676));
#23743=CARTESIAN_POINT('Ctrl Pts',(4.87795629785876,0.628271771353843,7.64582178907685));
#23744=CARTESIAN_POINT('Ctrl Pts',(4.85956207898706,0.771086075418557,7.65397656269274));
#23745=CARTESIAN_POINT('Ctrl Pts',(4.83488946854167,0.913109241979222,7.66213133630864));
#23746=CARTESIAN_POINT('Ctrl Pts',(4.80403186908258,1.05378406864922,7.67028610992454));
#23747=CARTESIAN_POINT('Ctrl Pts',(4.77317317531592,1.19446388409125,7.67844117273436));
#23748=CARTESIAN_POINT('Ctrl Pts',(4.73612912166717,1.33379493631443,7.6865962355442));
#23749=CARTESIAN_POINT('Ctrl Pts',(4.69304411621821,1.47123077242479,7.69475129835402));
#23750=CARTESIAN_POINT('Ctrl Pts',(4.64996163770159,1.60865854793365,7.70290588287003));
#23751=CARTESIAN_POINT('Ctrl Pts',(4.60083901722313,1.74419101067667,7.71106046738603));
#23752=CARTESIAN_POINT('Ctrl Pts',(4.5458703560629,1.87729746400739,7.71921505190204));
#23753=CARTESIAN_POINT('Ctrl Pts',(4.49088818003972,2.01043664353947,7.72737164134394));
#23754=CARTESIAN_POINT('Ctrl Pts',(4.43005721879998,2.1411483122626,7.73552823078584));
#23755=CARTESIAN_POINT('Ctrl Pts',(4.36361972559094,2.26892175998504,7.74368482022774));
#23756=CARTESIAN_POINT('Ctrl Pts',(4.31851116449161,2.35567512913047,7.74922283792573));
#23757=CARTESIAN_POINT('Ctrl Pts',(4.27081904526634,2.44107443420284,7.75476085562373));
#23758=CARTESIAN_POINT('Ctrl Pts',(4.22063128929397,2.52496625370176,7.76029887332172));
#23759=CARTESIAN_POINT('Ctrl Pts',(4.14671438879556,2.6485227497911,7.76845530700181));
#23760=CARTESIAN_POINT('Ctrl Pts',(4.06735438141007,2.76885429624838,7.77661174068191));
#23761=CARTESIAN_POINT('Ctrl Pts',(3.98285740119603,2.88548609149966,7.784768174362));
#23762=CARTESIAN_POINT('Ctrl Pts',(3.89837761849953,3.00209414889262,7.79292294797789));
#23763=CARTESIAN_POINT('Ctrl Pts',(3.80876314492887,3.11500368645602,7.80107772159379));
#23764=CARTESIAN_POINT('Ctrl Pts',(3.7143625846748,3.22377009913361,7.80923249520969));
#23765=CARTESIAN_POINT('Ctrl Pts',(3.61995867667985,3.33254036901041,7.81738755801952));
#23766=CARTESIAN_POINT('Ctrl Pts',(3.52076855886865,3.43716696483075,7.82554262082935));
#23767=CARTESIAN_POINT('Ctrl Pts',(3.41718048160865,3.53723912375356,7.83369768363918));
#23768=CARTESIAN_POINT('Ctrl Pts',(3.31359847978159,3.63730541345177,7.84185226815519));
#23769=CARTESIAN_POINT('Ctrl Pts',(3.20561927588551,3.73281756883447,7.85000685267119));
#23770=CARTESIAN_POINT('Ctrl Pts',(3.0936672186751,3.82340243795955,7.8581614371872));
#23771=CARTESIAN_POINT('Ctrl Pts',(2.98168763638626,3.91400957872206,7.86631802662911));
#23772=CARTESIAN_POINT('Ctrl Pts',(2.86573350906554,3.99968680173407,7.87447461607101));
#23773=CARTESIAN_POINT('Ctrl Pts',(2.74626190658445,4.08010154321472,7.88263120551291));
#23774=CARTESIAN_POINT('Ctrl Pts',(2.66514517836632,4.13470013061083,7.88816922321089));
#23775=CARTESIAN_POINT('Ctrl Pts',(2.58240760078612,4.18687361812252,7.89370724090886));
#23776=CARTESIAN_POINT('Ctrl Pts',(2.49819978186957,4.23652934751629,7.89924525860684));
#23777=CARTESIAN_POINT('Ctrl Pts',(2.3741778794859,4.30966267531056,7.90740169228692));
#23778=CARTESIAN_POINT('Ctrl Pts',(2.24691919032533,4.37735992693958,7.915558125967));
#23779=CARTESIAN_POINT('Ctrl Pts',(2.1169196995089,4.43935063363226,7.92371455964709));
#23780=CARTESIAN_POINT('Ctrl Pts',(1.98694666725375,4.5013287234685,7.93186933326297));
#23781=CARTESIAN_POINT('Ctrl Pts',(1.85423424804504,4.55760244143561,7.94002410687886));
#23782=CARTESIAN_POINT('Ctrl Pts',(1.71930127391744,4.60794815422286,7.94817888049475));
#23783=CARTESIAN_POINT('Ctrl Pts',(1.58436351464194,4.65829565242753,7.95633394330457));
#23784=CARTESIAN_POINT('Ctrl Pts',(1.44720535506439,4.70271460430195,7.9644890061144));
#23785=CARTESIAN_POINT('Ctrl Pts',(1.30836425012304,4.74103006228604,7.97264406892422));
#23786=CARTESIAN_POINT('Ctrl Pts',(1.16953128820214,4.77934327307138,7.98079865344022));
#23787=CARTESIAN_POINT('Ctrl Pts',(1.02901590122402,4.81155361802777,7.98895323795622));
#23788=CARTESIAN_POINT('Ctrl Pts',(0.887369248564386,4.83753644732546,7.99710782247221));
#23789=CARTESIAN_POINT('Ctrl Pts',(0.745687769968309,4.86352566488822,8.00526441191411));
#23790=CARTESIAN_POINT('Ctrl Pts',(0.60287479915392,4.88328424664097,8.01342100135601));
#23791=CARTESIAN_POINT('Ctrl Pts',(0.459490809848882,4.89673883908101,8.0215775907979));
#23792=CARTESIAN_POINT('Ctrl Pts',(0.362138469628618,4.90587400171036,8.02711560849592));
#23793=CARTESIAN_POINT('Ctrl Pts',(0.264523077887973,4.91210415728261,8.03265362619394));
#23794=CARTESIAN_POINT('Ctrl Pts',(0.16682121793857,4.91541999667836,8.03819164389196));
#23795=CARTESIAN_POINT('Ctrl Pts',(0.0229251914986702,4.9203035896172,8.04634807757206));
#23796=CARTESIAN_POINT('Ctrl Pts',(-0.121212320760765,4.9188650470535,8.05450451125216));
#23797=CARTESIAN_POINT('Ctrl Pts',(-0.265026381185507,4.91110416095767,
8.06266094493225));
#23798=CARTESIAN_POINT('Ctrl Pts',(-0.40881117139462,4.90334485442095,8.07081571854815));
#23799=CARTESIAN_POINT('Ctrl Pts',(-0.552272307158635,4.88926578941549,
8.07897049216404));
#23800=CARTESIAN_POINT('Ctrl Pts',(-0.694847196162797,4.86891881596774,
8.08712526577994));
#23801=CARTESIAN_POINT('Ctrl Pts',(-0.837427141321202,4.84857112095228,
8.09528032858977));
#23802=CARTESIAN_POINT('Ctrl Pts',(-0.979120445041749,4.82195511627215,
8.10343539139961));
#23803=CARTESIAN_POINT('Ctrl Pts',(-1.1193714547929,4.78917431387654,8.11159045420944));
#23804=CARTESIAN_POINT('Ctrl Pts',(-1.25961423883288,4.75639543407252,8.11974503872545));
#23805=CARTESIAN_POINT('Ctrl Pts',(-1.39841457249709,4.71745255700106,8.12789962324147));
#23806=CARTESIAN_POINT('Ctrl Pts',(-1.53522883328251,4.67249991888261,8.13605420775748));
#23807=CARTESIAN_POINT('Ctrl Pts',(-1.6720767318888,4.6275362284895,8.14421079719938));
#23808=CARTESIAN_POINT('Ctrl Pts',(-1.80693726375302,4.57655992879013,8.15236738664128));
#23809=CARTESIAN_POINT('Ctrl Pts',(-1.93928316919885,4.51977475679508,8.16052397608318));
#23810=CARTESIAN_POINT('Ctrl Pts',(-2.02914106530028,4.48121975905606,8.16606199378115));
#23811=CARTESIAN_POINT('Ctrl Pts',(-2.11784009512883,4.43998795518557,8.17160001147911));
#23812=CARTESIAN_POINT('Ctrl Pts',(-2.20522074303678,4.39615565431665,8.17713802917708));
#23813=CARTESIAN_POINT('Ctrl Pts',(-2.33391561157184,4.33159911539219,8.18529446285716));
#23814=CARTESIAN_POINT('Ctrl Pts',(-2.4597978017508,4.26137542963897,8.19345089653725));
#23815=CARTESIAN_POINT('Ctrl Pts',(-2.58237112939528,4.18575470047705,8.20160733021734));
#23816=CARTESIAN_POINT('Ctrl Pts',(-2.70491950991187,4.11014936226549,8.20976210383322));
#23817=CARTESIAN_POINT('Ctrl Pts',(-2.82416008676265,4.02914934758439,8.21791687744911));
#23818=CARTESIAN_POINT('Ctrl Pts',(-2.93962364167508,3.943069351128,8.22607165106499));
#23819=CARTESIAN_POINT('Ctrl Pts',(-3.05509129128864,3.85698630200394,8.23422671387482));
#23820=CARTESIAN_POINT('Ctrl Pts',(-3.16678138042917,3.76582310760995,8.24238177668464));
#23821=CARTESIAN_POINT('Ctrl Pts',(-3.2742555016918,3.66993650791686,8.25053683949447));
#23822=CARTESIAN_POINT('Ctrl Pts',(-3.38172331960527,3.57405553196566,8.25869142401047));
#23823=CARTESIAN_POINT('Ctrl Pts',(-3.48497541525943,3.47345192843738,8.26684600852648));
#23824=CARTESIAN_POINT('Ctrl Pts',(-3.58360821337217,3.3685212238535,8.27500059304248));
#23825=CARTESIAN_POINT('Ctrl Pts',(-3.68226526182543,3.26356472049513,8.28315718248438));
#23826=CARTESIAN_POINT('Ctrl Pts',(-3.77630051385871,3.15427923398948,8.29131377192628));
#23827=CARTESIAN_POINT('Ctrl Pts',(-3.86534844568513,3.04109593007843,8.29947036136818));
#23828=CARTESIAN_POINT('Ctrl Pts',(-3.92580864488223,2.96424872026801,8.3050083790662));
#23829=CARTESIAN_POINT('Ctrl Pts',(-3.98397053870476,2.8856053883823,8.31054639676421));
#23830=CARTESIAN_POINT('Ctrl Pts',(-4.03973056180145,2.80530926112387,8.31608441446223));
#23831=CARTESIAN_POINT('Ctrl Pts',(-4.12289735951155,2.68554654579954,8.32434443969226));
#23832=CARTESIAN_POINT('Ctrl Pts',(-4.20075037613452,2.56206019082026,8.33260446492229));
#23833=CARTESIAN_POINT('Ctrl Pts',(-4.27297159049031,2.43534327136087,8.34086449015232));
#23834=CARTESIAN_POINT('Ctrl Pts',(-4.34427488904071,2.31023689617466,8.34901953227206));
#23835=CARTESIAN_POINT('Ctrl Pts',(-4.41008855441688,2.18198190344048,8.35717457439181));
#23836=CARTESIAN_POINT('Ctrl Pts',(-4.47015167695163,2.05107948347852,8.36532961651156));
#23837=CARTESIAN_POINT('Ctrl Pts',(-4.53137462429007,1.91764932491212,8.37364213329673));
#23838=CARTESIAN_POINT('Ctrl Pts',(-4.5866224854162,1.78146875710113,8.3819546500819));
#23839=CARTESIAN_POINT('Ctrl Pts',(-4.63566945407151,1.64309213834414,8.39026716686708));
#23840=CARTESIAN_POINT('Ctrl Pts',(-4.68471642272683,1.50471551958715,8.39857968365225));
#23841=CARTESIAN_POINT('Ctrl Pts',(-4.72756237674539,1.36414319731729,8.40689220043742));
#23842=CARTESIAN_POINT('Ctrl Pts',(-4.76403458704967,1.22194824599671,8.41520471722259));
#23843=CARTESIAN_POINT('Ctrl Pts',(-4.91824999943065,-7.48357700250612E-5,
6.73532637328698));
#23844=CARTESIAN_POINT('Ctrl Pts',(-4.91825068197842,0.044782597342662,
6.73280315748358));
#23845=CARTESIAN_POINT('Ctrl Pts',(-4.91763767400033,0.0896377529279913,
6.73027690885947));
#23846=CARTESIAN_POINT('Ctrl Pts',(-4.91529202496372,0.175392823737547,
6.72543828609909));
#23847=CARTESIAN_POINT('Ctrl Pts',(-4.91366219255074,0.216291843413273,
6.72312674364904));
#23848=CARTESIAN_POINT('Ctrl Pts',(-4.90800307853509,0.324373432807522,
6.71700549422386));
#23849=CARTESIAN_POINT('Ctrl Pts',(-4.9031050174068,0.391501465204401,6.713190634307));
#23850=CARTESIAN_POINT('Ctrl Pts',(-4.88631051071312,0.570865805284201,
6.70295469375948));
#23851=CARTESIAN_POINT('Ctrl Pts',(-4.87192610393772,0.682827722773605,
6.69651966464271));
#23852=CARTESIAN_POINT('Ctrl Pts',(-4.83016420314059,0.938054762448882,
6.68173546027204));
#23853=CARTESIAN_POINT('Ctrl Pts',(-4.80024346688583,1.08077994976788,6.67338283263945));
#23854=CARTESIAN_POINT('Ctrl Pts',(-4.76403458034885,1.22194827212136,6.66505438904205));
#23855=CARTESIAN_POINT('Ctrl Pts',(-4.76403458747083,1.22194824435476,6.31969203503535));
#23856=CARTESIAN_POINT('Ctrl Pts',(-4.77178283058391,1.1917400106154,6.32145364669194));
#23857=CARTESIAN_POINT('Ctrl Pts',(-4.77924378711755,1.16145794762219,6.32321713004904));
#23858=CARTESIAN_POINT('Ctrl Pts',(-4.80103637042951,1.06923991961347,6.32858121421732));
#23859=CARTESIAN_POINT('Ctrl Pts',(-4.81445539466772,1.00709650795569,6.33218747631128));
#23860=CARTESIAN_POINT('Ctrl Pts',(-4.87091265910445,0.718648100760694,
6.34889799567108));
#23861=CARTESIAN_POINT('Ctrl Pts',(-4.89922231388978,0.489758247256351,
6.36209293286357));
#23862=CARTESIAN_POINT('Ctrl Pts',(-4.91596178877969,0.173225970591947,
6.38022198480445));
#23863=CARTESIAN_POINT('Ctrl Pts',(-4.91825032080293,0.0866118245555618,
6.38516859458936));
#23864=CARTESIAN_POINT('Ctrl Pts',(-4.91824985906285,-0.0380692441522994,
6.39225712131835));
#23865=CARTESIAN_POINT('Ctrl Pts',(-4.91780813497978,-0.076119322468207,
6.39441593126176));
#23866=CARTESIAN_POINT('Ctrl Pts',(-4.91579114373851,-0.162991404124876,
6.39933325600049));
#23867=CARTESIAN_POINT('Ctrl Pts',(-4.91393004110767,-0.211802730676662,
6.40208857352072));
#23868=CARTESIAN_POINT('Ctrl Pts',(-4.90795465352176,-0.324425840632596,
6.40843776971936));
#23869=CARTESIAN_POINT('Ctrl Pts',(-4.90332242625457,-0.388201355869752,
6.41202710696751));
#23870=CARTESIAN_POINT('Ctrl Pts',(-4.87692525221264,-0.674299447633779,
6.42813920866103));
#23871=CARTESIAN_POINT('Ctrl Pts',(-4.84127308265718,-0.895071847565557,
6.44061271800409));
#23872=CARTESIAN_POINT('Ctrl Pts',(-4.77626862988934,-1.17496066822926,
6.45680897234867));
#23873=CARTESIAN_POINT('Ctrl Pts',(-4.7605837988785,-1.23697873026874,6.4604214837415));
#23874=CARTESIAN_POINT('Ctrl Pts',(-4.72457726150975,-1.36850069337734,
6.46814080145536));
#23875=CARTESIAN_POINT('Ctrl Pts',(-4.70392126793976,-1.43789741908723,
6.47224907536894));
#23876=CARTESIAN_POINT('Ctrl Pts',(-4.66937855276934,-1.54522336114714,
6.478662937225));
#23877=CARTESIAN_POINT('Ctrl Pts',(-4.65654380800173,-1.58348067361957,
6.48096127111801));
#23878=CARTESIAN_POINT('Ctrl Pts',(-4.57902831121979,-1.80543951935753,
6.49436778766183));
#23879=CARTESIAN_POINT('Ctrl Pts',(-4.50395269367732,-1.98532649315502,
6.50553107493504));
#23880=CARTESIAN_POINT('Ctrl Pts',(-4.38645067987844,-2.22565220641557,
6.5208227379221));
#23881=CARTESIAN_POINT('Ctrl Pts',(-4.35304405580042,-2.29030236888245,
6.52497480778277));
#23882=CARTESIAN_POINT('Ctrl Pts',(-4.30000015922807,-2.38759916720453,
6.53127510341335));
#23883=CARTESIAN_POINT('Ctrl Pts',(-4.28139788170872,-2.42079808984258,
6.53343407288476));
#23884=CARTESIAN_POINT('Ctrl Pts',(-4.23804790655977,-2.49610051731637,
6.53835102910746));
#23885=CARTESIAN_POINT('Ctrl Pts',(-4.21305465290573,-2.53805800197352,
6.54110582230903));
#23886=CARTESIAN_POINT('Ctrl Pts',(-4.15391546406366,-2.63405672965554,
6.54745341383125));
#23887=CARTESIAN_POINT('Ctrl Pts',(-4.11933253421103,-2.68781846700604,
6.55104167402111));
#23888=CARTESIAN_POINT('Ctrl Pts',(-3.95919476207011,-2.92641110212529,
6.56715590881812));
#23889=CARTESIAN_POINT('Ctrl Pts',(-3.82218185833917,-3.10322895657413,
6.5796325671518));
#23890=CARTESIAN_POINT('Ctrl Pts',(-3.63109643789519,-3.31789283219575,
6.59583186933676));
#23891=CARTESIAN_POINT('Ctrl Pts',(-3.58764089355813,-3.3648338584015,6.59944420412304));
#23892=CARTESIAN_POINT('Ctrl Pts',(-3.49307026046255,-3.46307453662107,
6.60716360002116));
#23893=CARTESIAN_POINT('Ctrl Pts',(-3.4417127417228,-3.51411985128582,6.61127213081374));
#23894=CARTESIAN_POINT('Ctrl Pts',(-3.36000320386708,-3.59182268156121,
6.6176865357552));
#23895=CARTESIAN_POINT('Ctrl Pts',(-3.33041781073134,-3.61927187240741,
6.61998515559381));
#23896=CARTESIAN_POINT('Ctrl Pts',(-3.15611492101516,-3.7770421803878,6.633391518541));
#23897=CARTESIAN_POINT('Ctrl Pts',(-3.00409750124454,-3.89903914432749,
6.64455435374067));
#23898=CARTESIAN_POINT('Ctrl Pts',(-2.78590797394217,-4.05378744601438,
6.65984499410598));
#23899=CARTESIAN_POINT('Ctrl Pts',(-2.72563892459175,-4.09455352036824,
6.66399650542669));
#23900=CARTESIAN_POINT('Ctrl Pts',(-2.63250292993435,-4.15458293517651,
6.67029616093516));
#23901=CARTESIAN_POINT('Ctrl Pts',(-2.60028012236711,-4.17482627031082,
6.67245504574602));
#23902=CARTESIAN_POINT('Ctrl Pts',(-2.52617107903467,-4.22019288809571,
6.67737219548491));
#23903=CARTESIAN_POINT('Ctrl Pts',(-2.48413904789124,-4.24507027067345,
6.68012726489912));
#23904=CARTESIAN_POINT('Ctrl Pts',(-2.38625013356782,-4.30105570045904,
6.68647570174519));
#23905=CARTESIAN_POINT('Ctrl Pts',(-2.33014324305514,-4.33170894759047,
6.69006452930829));
#23906=CARTESIAN_POINT('Ctrl Pts',(-2.07535229382865,-4.46452736069087,
6.70617764021293));
#23907=CARTESIAN_POINT('Ctrl Pts',(-1.87044581954264,-4.55417645095849,
6.71865263951328));
#23908=CARTESIAN_POINT('Ctrl Pts',(-1.59994815344273,-4.65117622857774,
6.73485033595483));
#23909=CARTESIAN_POINT('Ctrl Pts',(-1.53932371869043,-4.67159039092748,
6.73846276378926));
#23910=CARTESIAN_POINT('Ctrl Pts',(-1.40926726626786,-4.71257790642061,
6.74618211845602));
#23911=CARTESIAN_POINT('Ctrl Pts',(-1.33974418774053,-4.73281207088394,
6.75029051386871));
#23912=CARTESIAN_POINT('Ctrl Pts',(-1.23081467734926,-4.7619225869941,6.75670463259733));
#23913=CARTESIAN_POINT('Ctrl Pts',(-1.19170238672114,-4.771860946282,6.75900310174045));
#23914=CARTESIAN_POINT('Ctrl Pts',(-0.963142482804232,-4.82695225004833,
6.77240966312414));
#23915=CARTESIAN_POINT('Ctrl Pts',(-0.771269805782495,-4.86130161291053,
6.78357285535616));
#23916=CARTESIAN_POINT('Ctrl Pts',(-0.505617272158434,-4.89273212417459,
6.79886408140672));
#23917=CARTESIAN_POINT('Ctrl Pts',(-0.433184010815897,-4.89967634230047,
6.80301581710834));
#23918=CARTESIAN_POINT('Ctrl Pts',(-0.322672362076679,-4.90780130331323,
6.80931572976934));
#23919=CARTESIAN_POINT('Ctrl Pts',(-0.284690448949799,-4.91015096458474,
6.81147464858849));
#23920=CARTESIAN_POINT('Ctrl Pts',(-0.19790886319272,-4.9145091536491,6.81639172056273));
#23921=CARTESIAN_POINT('Ctrl Pts',(-0.149098890094445,-4.91623206727721,
6.81914667899317));
#23922=CARTESIAN_POINT('Ctrl Pts',(-0.0363604621139229,-4.91853100351121,
6.8254947761769));
#23923=CARTESIAN_POINT('Ctrl Pts',(0.02756980110591,-4.91858814327327,6.82908337575979));
#23924=CARTESIAN_POINT('Ctrl Pts',(0.314859149471245,-4.91324340934329,
6.84519693820587));
#23925=CARTESIAN_POINT('Ctrl Pts',(0.53769045165593,-4.89387219634178,6.85767260407866));
#23926=CARTESIAN_POINT('Ctrl Pts',(0.821628175002489,-4.84955683112862,
6.87387094568142));
#23927=CARTESIAN_POINT('Ctrl Pts',(0.884627108629116,-4.83846143763935,
6.8774833361316));
#23928=CARTESIAN_POINT('Ctrl Pts',(1.01843579026431,-4.81219424265948,6.88520270735362));
#23929=CARTESIAN_POINT('Ctrl Pts',(1.08916311691707,-4.79668098040192,6.88931115714788));
#23930=CARTESIAN_POINT('Ctrl Pts',(1.19873895105736,-4.77009816529883,6.89572539084788));
#23931=CARTESIAN_POINT('Ctrl Pts',(1.23783755790536,-4.7601018617538,6.89802392052561));
#23932=CARTESIAN_POINT('Ctrl Pts',(1.46488165059817,-4.69906718937616,6.91143043352738));
#23933=CARTESIAN_POINT('Ctrl Pts',(1.64978505091154,-4.63738277533979,6.92259351401493));
#23934=CARTESIAN_POINT('Ctrl Pts',(1.89806798841607,-4.5378204130107,6.93788451726422));
#23935=CARTESIAN_POINT('Ctrl Pts',(1.96498631693775,-4.50924662724441,6.94203614417355));
#23936=CARTESIAN_POINT('Ctrl Pts',(2.06590227474172,-4.46348281677045,6.94833593215241));
#23937=CARTESIAN_POINT('Ctrl Pts',(2.10037469255156,-4.44736520604732,6.9504948344821));
#23938=CARTESIAN_POINT('Ctrl Pts',(2.1786553176585,-4.40965182755431,6.95541194415692));
#23939=CARTESIAN_POINT('Ctrl Pts',(2.22233583897437,-4.38780032945321,6.9581669563948));
#23940=CARTESIAN_POINT('Ctrl Pts',(2.32242274327858,-4.33585310759225,6.96451521825342));
#23941=CARTESIAN_POINT('Ctrl Pts',(2.37858231812219,-4.30530089847534,6.96810392836518));
#23942=CARTESIAN_POINT('Ctrl Pts',(2.62825926812963,-4.16309352426808,6.98421727188625));
#23943=CARTESIAN_POINT('Ctrl Pts',(2.81462700601331,-4.03942672935072,6.99669261458354));
#23944=CARTESIAN_POINT('Ctrl Pts',(3.04270679528162,-3.86460990480026,7.01289064339163));
#23945=CARTESIAN_POINT('Ctrl Pts',(3.09270892510015,-3.82471250572877,7.01650305196705));
#23946=CARTESIAN_POINT('Ctrl Pts',(3.19761919515084,-3.73760034042959,7.02422241516076));
#23947=CARTESIAN_POINT('Ctrl Pts',(3.25229154497666,-3.69012525037815,7.02833083858715));
#23948=CARTESIAN_POINT('Ctrl Pts',(3.33577377972258,-3.61433601491832,7.03474501654138));
#23949=CARTESIAN_POINT('Ctrl Pts',(3.36531697440985,-3.58684445921951,7.03704351686796));
#23950=CARTESIAN_POINT('Ctrl Pts',(3.53544619155861,-3.42457754102047,7.05045005859609));
#23951=CARTESIAN_POINT('Ctrl Pts',(3.66826527567222,-3.28191102770945,7.06161319859044));
#23952=CARTESIAN_POINT('Ctrl Pts',(3.83860093819687,-3.07564938708435,7.07690431196482));
#23953=CARTESIAN_POINT('Ctrl Pts',(3.88367821962874,-3.0185294404834,7.08105598848666));
#23954=CARTESIAN_POINT('Ctrl Pts',(3.9503770514992,-2.93004304153632,7.08735583332418));
#23955=CARTESIAN_POINT('Ctrl Pts',(3.97292882179493,-2.89939092084906,7.08951474317347));
#23956=CARTESIAN_POINT('Ctrl Pts',(4.02360660282389,-2.82880860014699,7.09443183565475));
#23957=CARTESIAN_POINT('Ctrl Pts',(4.05149810912533,-2.78871499820808,7.09718682335397));
#23958=CARTESIAN_POINT('Ctrl Pts',(4.11450790945524,-2.69519834457089,7.10353501011303));
#23959=CARTESIAN_POINT('Ctrl Pts',(4.14919102093863,-2.6414926512652,7.10712366981832));
#23960=CARTESIAN_POINT('Ctrl Pts',(4.30033764449198,-2.3971215668924,7.12323711317747));
#23961=CARTESIAN_POINT('Ctrl Pts',(4.40477389066716,-2.19933209126232,7.13571260325617));
#23962=CARTESIAN_POINT('Ctrl Pts',(4.5213488951806,-1.93666685498963,7.15191077471157));
#23963=CARTESIAN_POINT('Ctrl Pts',(4.54615291529909,-1.87770282484303,7.15552317502115));
#23964=CARTESIAN_POINT('Ctrl Pts',(4.59656596951498,-1.75100146772376,7.16324254187564));
#23965=CARTESIAN_POINT('Ctrl Pts',(4.6218433579639,-1.68314843716951,7.16735097732638));
#23966=CARTESIAN_POINT('Ctrl Pts',(4.65886271020273,-1.57664511050129,7.17376518070197));
#23967=CARTESIAN_POINT('Ctrl Pts',(4.67164226754552,-1.53836603437918,7.17606369441338));
#23968=CARTESIAN_POINT('Ctrl Pts',(4.74334300352038,-1.31446113729494,7.18947022427023));
#23969=CARTESIAN_POINT('Ctrl Pts',(4.79166765767429,-1.12562471879695,7.20063333837024));
#23970=CARTESIAN_POINT('Ctrl Pts',(4.84249076595225,-0.862994459733448,
7.2159244020139));
#23971=CARTESIAN_POINT('Ctrl Pts',(4.85472691289473,-0.791266730478749,
7.22007605517951));
#23972=CARTESIAN_POINT('Ctrl Pts',(4.87093260873582,-0.681649903374358,
7.22637587324951));
#23973=CARTESIAN_POINT('Ctrl Pts',(4.87606079811396,-0.643942717480421,
7.22853477955875));
#23974=CARTESIAN_POINT('Ctrl Pts',(4.88677026056715,-0.557713753790923,
7.23345188013408));
#23975=CARTESIAN_POINT('Ctrl Pts',(4.89206741692258,-0.50916075844421,7.23620687938527));
#23976=CARTESIAN_POINT('Ctrl Pts',(4.90262645512341,-0.396892113144574,
7.24255510149858));
#23977=CARTESIAN_POINT('Ctrl Pts',(4.90737094656236,-0.333136611869135,
7.24614378493346));
#23978=CARTESIAN_POINT('Ctrl Pts',(4.92310448246431,-0.0462315612044295,
7.26225718129194));
#23979=CARTESIAN_POINT('Ctrl Pts',(4.92012375211529,0.177415835946856,7.27473260198826));
#23980=CARTESIAN_POINT('Ctrl Pts',(4.89674708081442,0.463834425980844,7.29093070628994));
#23981=CARTESIAN_POINT('Ctrl Pts',(4.89030077242132,0.527477574863849,7.29454311049082));
#23982=CARTESIAN_POINT('Ctrl Pts',(4.87391548083669,0.662851962028703,7.30226247562188));
#23983=CARTESIAN_POINT('Ctrl Pts',(4.86362993746052,0.734526040634645,7.30637090541187));
#23984=CARTESIAN_POINT('Ctrl Pts',(4.84515319410033,0.845755327414831,7.31278509681974));
#23985=CARTESIAN_POINT('Ctrl Pts',(4.83805068678152,0.885481267418061,7.31508360422993));
#23986=CARTESIAN_POINT('Ctrl Pts',(4.79382776815947,1.1163898714064,7.32849013993213));
#23987=CARTESIAN_POINT('Ctrl Pts',(4.74586681008939,1.30531921586182,7.339653266482));
#23988=CARTESIAN_POINT('Ctrl Pts',(4.6647767160168,1.56023539026103,7.3549443536397));
#23989=CARTESIAN_POINT('Ctrl Pts',(4.64118623628629,1.62906930027749,7.35909601764795));
#23990=CARTESIAN_POINT('Ctrl Pts',(4.60294471798695,1.73306981825063,7.3653958481442));
#23991=CARTESIAN_POINT('Ctrl Pts',(4.58939804413654,1.76863131402072,7.36755475609683));
#23992=CARTESIAN_POINT('Ctrl Pts',(4.55752595544476,1.84946623835404,7.37247185291465));
#23993=CARTESIAN_POINT('Ctrl Pts',(4.53893614759754,1.8946310797409,7.37522684680306));
#23994=CARTESIAN_POINT('Ctrl Pts',(4.49446774063554,1.99825654285989,7.38157505250386));
#23995=CARTESIAN_POINT('Ctrl Pts',(4.4681158035053,2.05650449806004,7.38516372492274));
#23996=CARTESIAN_POINT('Ctrl Pts',(4.34459761442576,2.31593759231043,7.40127714310026));
#23997=CARTESIAN_POINT('Ctrl Pts',(4.23492756844381,2.51087292893292,7.41375259600591));
#23998=CARTESIAN_POINT('Ctrl Pts',(4.07730338704221,2.75115819865284,7.42995073148231));
#23999=CARTESIAN_POINT('Ctrl Pts',(4.04117966895238,2.80395098312828,7.43356313387674));
#24000=CARTESIAN_POINT('Ctrl Pts',(3.96199412911397,2.91496610020577,7.44128249980783));
#24001=CARTESIAN_POINT('Ctrl Pts',(3.91865538660908,2.97297235784486,7.44539093222567));
#24002=CARTESIAN_POINT('Ctrl Pts',(3.84919097806788,3.06178711974118,7.45180512918924));
#24003=CARTESIAN_POINT('Ctrl Pts',(3.82393945699752,3.09326664808159,7.4541036395246));
#24004=CARTESIAN_POINT('Ctrl Pts',(3.67458349587361,3.27483543226568,7.46751017257027));
#24005=CARTESIAN_POINT('Ctrl Pts',(3.54203969687229,3.4177572735651,7.47867329339827));
#24006=CARTESIAN_POINT('Ctrl Pts',(3.34882296625803,3.6027574177494,7.49396436966288));
#24007=CARTESIAN_POINT('Ctrl Pts',(3.29516212942431,3.65190128467041,7.49811602860376));
#24008=CARTESIAN_POINT('Ctrl Pts',(3.21180463970207,3.72490832466444,7.50441585329254));
#24009=CARTESIAN_POINT('Ctrl Pts',(3.18288859267893,3.74964682844187,7.50657476047713));
#24010=CARTESIAN_POINT('Ctrl Pts',(3.11621195223415,3.80536348782805,7.51149185905104));
#24011=CARTESIAN_POINT('Ctrl Pts',(3.07827119880927,3.83611974672936,7.51424685544575));
#24012=CARTESIAN_POINT('Ctrl Pts',(2.98962586473817,3.90581703147857,7.52059506881696));
#24013=CARTESIAN_POINT('Ctrl Pts',(2.93860749021198,3.94434476362664,7.52418374638418));
#24014=CARTESIAN_POINT('Ctrl Pts',(2.70597695217865,4.11300182049617,7.54029715436445));
#24015=CARTESIAN_POINT('Ctrl Pts',(2.51637810379095,4.23165871643153,7.55277259221695));
#24016=CARTESIAN_POINT('Ctrl Pts',(2.26296817405587,4.36717865322322,7.56897071312374));
#24017=CARTESIAN_POINT('Ctrl Pts',(2.20598148821953,4.39623929150023,7.57258311636243));
#24018=CARTESIAN_POINT('Ctrl Pts',(2.08331757197039,4.45580663132141,7.58030248191965));
#24019=CARTESIAN_POINT('Ctrl Pts',(2.01750063482169,4.485991068307,7.58441091310937));
#24020=CARTESIAN_POINT('Ctrl Pts',(1.91399845690158,4.53071975047165,7.59082510747651));
#24021=CARTESIAN_POINT('Ctrl Pts',(1.87675951482418,4.54627157663472,7.5931236164448));
#24022=CARTESIAN_POINT('Ctrl Pts',(1.65871446616653,4.63419651230902,7.60653015074433));
#24023=CARTESIAN_POINT('Ctrl Pts',(1.47392943744713,4.69623700712047,7.61769327425889));
#24024=CARTESIAN_POINT('Ctrl Pts',(1.21573224659156,4.7661799568481,7.6329843556193));
#24025=CARTESIAN_POINT('Ctrl Pts',(1.14509462496572,4.78364241535902,7.63713601692109));
#24026=CARTESIAN_POINT('Ctrl Pts',(1.03683686822607,4.80786959794581,7.64344307169396));
#24027=CARTESIAN_POINT('Ctrl Pts',(0.99948247674698,4.81577362446879,7.64560917348137));
#24028=CARTESIAN_POINT('Ctrl Pts',(0.927939186921827,4.8300435829962,7.64973741796102));
#24029=CARTESIAN_POINT('Ctrl Pts',(0.893767593379231,4.83648339884518,7.65170070792163));
#24030=CARTESIAN_POINT('Ctrl Pts',(0.85560335904116,4.84325736068748,7.65388558077693));
#24031=CARTESIAN_POINT('Ctrl Pts',(0.85167548729847,4.84394961103328,7.65411035631631));
#24032=CARTESIAN_POINT('Ctrl Pts',(0.841213707107986,4.84578028281944,7.65470880054106));
#24033=CARTESIAN_POINT('Ctrl Pts',(0.834678326720705,4.84691026752705,7.65508239480081));
#24034=CARTESIAN_POINT('Ctrl Pts',(0.817317607904486,4.84987582801172,7.65607418497732));
#24035=CARTESIAN_POINT('Ctrl Pts',(0.806488364786014,4.85168838008895,7.6566921890241));
#24036=CARTESIAN_POINT('Ctrl Pts',(0.724373839009992,4.8651498316236,7.66137369467279));
#24037=CARTESIAN_POINT('Ctrl Pts',(0.652845340211353,4.87526342165295,7.66542547178192));
#24038=CARTESIAN_POINT('Ctrl Pts',(0.3784903304552,4.9079087320114,7.68091165053709));
#24039=CARTESIAN_POINT('Ctrl Pts',(0.174558611429953,4.91938525749718,7.6923169665087));
#24040=CARTESIAN_POINT('Ctrl Pts',(-0.0930765618389588,4.91778026207772,
7.70739970893978));
#24041=CARTESIAN_POINT('Ctrl Pts',(-0.156645318064476,4.91616599474898,
7.71098981375896));
#24042=CARTESIAN_POINT('Ctrl Pts',(-0.284131261217925,4.91045338619682,
7.71821205787909));
#24043=CARTESIAN_POINT('Ctrl Pts',(-0.348035527932679,4.90633816485267,
7.72184362564228));
#24044=CARTESIAN_POINT('Ctrl Pts',(-0.484321578294143,4.8948857227741,7.72961775328187));
#24045=CARTESIAN_POINT('Ctrl Pts',(-0.556657849699929,4.88718789516025,
7.73376173588517));
#24046=CARTESIAN_POINT('Ctrl Pts',(-0.759828367297922,4.8609977000814,7.74545535619367));
#24047=CARTESIAN_POINT('Ctrl Pts',(-0.890126085322538,4.83883384570765,
7.75301992334525));
#24048=CARTESIAN_POINT('Ctrl Pts',(-1.12306673609224,4.7894821599995,7.76664820089394));
#24049=CARTESIAN_POINT('Ctrl Pts',(-1.2260248762179,4.76416641732152,7.77270903999833));
#24050=CARTESIAN_POINT('Ctrl Pts',(-1.36761361164759,4.72445779511306,7.78107714959033));
#24051=CARTESIAN_POINT('Ctrl Pts',(-1.40700199835899,4.71287745300862,7.78340858655596));
#24052=CARTESIAN_POINT('Ctrl Pts',(-1.47808680716164,4.69100763089798,7.78762061087861));
#24053=CARTESIAN_POINT('Ctrl Pts',(-1.50983230982812,4.68088662826973,7.78950337733068));
#24054=CARTESIAN_POINT('Ctrl Pts',(-1.54921060694038,4.66788988251512,7.79184263322448));
#24055=CARTESIAN_POINT('Ctrl Pts',(-1.55694215998566,4.66531677067464,7.79230210687444));
#24056=CARTESIAN_POINT('Ctrl Pts',(-1.57440098300788,4.65945812523704,7.79334011271191));
#24057=CARTESIAN_POINT('Ctrl Pts',(-1.58412443661279,4.65616132088417,7.79391853676024));
#24058=CARTESIAN_POINT('Ctrl Pts',(-1.60284438574317,4.64974876532318,7.79503283002394));
#24059=CARTESIAN_POINT('Ctrl Pts',(-1.61184229527788,4.64663729175639,7.79556873317469));
#24060=CARTESIAN_POINT('Ctrl Pts',(-1.68756493844513,4.62020601693896,7.80008151295579));
#24061=CARTESIAN_POINT('Ctrl Pts',(-1.75378926871329,4.59547629552562,7.80404696352562));
#24062=CARTESIAN_POINT('Ctrl Pts',(-2.01266330356796,4.4923953958986,7.81966617551992));
#24063=CARTESIAN_POINT('Ctrl Pts',(-2.20079311862945,4.40328724624318,7.83128755476275));
#24064=CARTESIAN_POINT('Ctrl Pts',(-2.41927666459205,4.28229262630039,7.84536297369916));
#24065=CARTESIAN_POINT('Ctrl Pts',(-2.45557791612058,4.26158031538454,7.8477213545114));
#24066=CARTESIAN_POINT('Ctrl Pts',(-2.54989189255759,4.20616260388858,7.85390339851401));
#24067=CARTESIAN_POINT('Ctrl Pts',(-2.60746050539538,4.17071961307367,7.85773208944402));
#24068=CARTESIAN_POINT('Ctrl Pts',(-2.72097051952861,4.09756649022808,7.86539931504959));
#24069=CARTESIAN_POINT('Ctrl Pts',(-2.77690329354805,4.05986941713503,7.86923699637247));
#24070=CARTESIAN_POINT('Ctrl Pts',(-2.87630836174342,3.98985772875539,7.87616937621111));
#24071=CARTESIAN_POINT('Ctrl Pts',(-2.92005596430082,3.95795245097997,7.87926084872527));
#24072=CARTESIAN_POINT('Ctrl Pts',(-3.10763152500895,3.81634999236261,7.89269505717952));
#24073=CARTESIAN_POINT('Ctrl Pts',(-3.24587337153958,3.69948742128846,7.90306746712873));
#24074=CARTESIAN_POINT('Ctrl Pts',(-3.41518489999616,3.53954829161749,7.91635078105455));
#24075=CARTESIAN_POINT('Ctrl Pts',(-3.45243742265772,3.50322222261266,7.91931212149051));
#24076=CARTESIAN_POINT('Ctrl Pts',(-3.51546145991991,3.43978372627169,7.92438607435672));
#24077=CARTESIAN_POINT('Ctrl Pts',(-3.54151260918142,3.41295617141851,7.92650250108592));
#24078=CARTESIAN_POINT('Ctrl Pts',(-3.57662920391338,3.37595793762689,7.92938335719712));
#24079=CARTESIAN_POINT('Ctrl Pts',(-3.5859617582813,3.36604318581503,7.93015174584316));
#24080=CARTESIAN_POINT('Ctrl Pts',(-3.60081466876786,3.35013182020227,7.93137924529148));
#24081=CARTESIAN_POINT('Ctrl Pts',(-3.60636148561714,3.344160033093,7.93183868955648));
#24082=CARTESIAN_POINT('Ctrl Pts',(-3.66481626328689,3.28091216233567,7.93669167442809));
#24083=CARTESIAN_POINT('Ctrl Pts',(-3.71637029823852,3.22239892947686,7.94106884369432));
#24084=CARTESIAN_POINT('Ctrl Pts',(-3.90811626378505,2.9940443597575,7.95778826929178));
#24085=CARTESIAN_POINT('Ctrl Pts',(-4.03823391256918,2.81608596980777,7.9700873078123));
#24086=CARTESIAN_POINT('Ctrl Pts',(-4.19188774783474,2.57327948826339,7.98628413891051));
#24087=CARTESIAN_POINT('Ctrl Pts',(-4.22662242456887,2.51582053535723,7.99007616922156));
#24088=CARTESIAN_POINT('Ctrl Pts',(-4.29191806672198,2.40263583924494,7.9974750697209));
#24089=CARTESIAN_POINT('Ctrl Pts',(-4.32259680498291,2.34699305863723,8.00108025677559));
#24090=CARTESIAN_POINT('Ctrl Pts',(-4.38736284553651,2.22394544153685,8.00898780776939));
#24091=CARTESIAN_POINT('Ctrl Pts',(-4.42099287813049,2.15631813023155,8.01329240851244));
#24092=CARTESIAN_POINT('Ctrl Pts',(-4.51615926623172,1.95335247217197,8.02609452662168));
#24093=CARTESIAN_POINT('Ctrl Pts',(-4.57313180781293,1.81596958664167,8.03461102999183));
#24094=CARTESIAN_POINT('Ctrl Pts',(-4.64817323254806,1.60897027349304,8.04720508761879));
#24095=CARTESIAN_POINT('Ctrl Pts',(-4.67108231578293,1.5411975475882,8.05129135760475));
#24096=CARTESIAN_POINT('Ctrl Pts',(-4.70577863845991,1.43066236506373,8.05788921025566));
#24097=CARTESIAN_POINT('Ctrl Pts',(-4.71848002125068,1.38819802177408,8.0604081695738));
#24098=CARTESIAN_POINT('Ctrl Pts',(-4.73983902255868,1.31310627375847,8.06483255285959));
#24099=CARTESIAN_POINT('Ctrl Pts',(-4.74873789707925,1.2805508395401,8.06674071604243));
#24100=CARTESIAN_POINT('Ctrl Pts',(-4.75956918758595,1.23925950449858,8.0691499986643));
#24101=CARTESIAN_POINT('Ctrl Pts',(-4.76181370441031,1.23060684651069,8.06965426408417));
#24102=CARTESIAN_POINT('Ctrl Pts',(-4.76403458713635,1.22194824565879,8.07015829796832));
#24103=CARTESIAN_POINT('Origin',(0.,0.,-3.23514056400928));
#24104=CARTESIAN_POINT('',(-4.76403458704821,1.22194824600244,10.1653249229632));
#24105=CARTESIAN_POINT('',(-4.76374494423105,1.22187361077196,9.81992259791717));
#24106=CARTESIAN_POINT('',(-4.76403458704967,1.22194824599672,-3.23514056400928));
#24107=CARTESIAN_POINT('',(-4.91824999837441,0.000126452135718109,8.48514056400927));
#24108=CARTESIAN_POINT('Ctrl Pts',(-4.76403458704821,1.22194824600244,10.1653249229632));
#24109=CARTESIAN_POINT('Ctrl Pts',(-4.76379686960342,1.22287503986022,10.1652702466491));
#24110=CARTESIAN_POINT('Ctrl Pts',(-4.76355888131435,1.22380176589749,10.1652155692027));
#24111=CARTESIAN_POINT('Ctrl Pts',(-4.72137445563459,1.38786911408632,10.1555345787607));
#24112=CARTESIAN_POINT('Ctrl Pts',(-4.67107487714302,1.54874686609432,10.1458780018919));
#24113=CARTESIAN_POINT('Ctrl Pts',(-4.59083775675595,1.76559678829643,10.1326750074967));
#24114=CARTESIAN_POINT('Ctrl Pts',(-4.56792959485441,1.82404569052493,10.12909764159));
#24115=CARTESIAN_POINT('Ctrl Pts',(-4.52983613972323,1.91601670895238,10.1234442094655));
#24116=CARTESIAN_POINT('Ctrl Pts',(-4.5153828869176,1.94983407238386,10.1213604786415));
#24117=CARTESIAN_POINT('Ctrl Pts',(-4.47710686609372,2.03668275729377,10.1159953495209));
#24118=CARTESIAN_POINT('Ctrl Pts',(-4.45272068633773,2.08945953606607,10.1127207221413));
#24119=CARTESIAN_POINT('Ctrl Pts',(-4.36174400915149,2.27752193488876,10.1009760808265));
#24120=CARTESIAN_POINT('Ctrl Pts',(-4.28987640509362,2.41016138859182,10.0925469864519));
#24121=CARTESIAN_POINT('Ctrl Pts',(-4.14862070490562,2.64446826013169,10.0772106915698));
#24122=CARTESIAN_POINT('Ctrl Pts',(-4.0812956305547,2.74723344088206,10.0703171379118));
#24123=CARTESIAN_POINT('Ctrl Pts',(-3.97388873739136,2.89850378996609,10.0598568339744));
#24124=CARTESIAN_POINT('Ctrl Pts',(-3.93660756454765,2.94893823176713,10.0563141078044));
#24125=CARTESIAN_POINT('Ctrl Pts',(-3.85407027465479,3.05624037300058,10.0486490059244));
#24126=CARTESIAN_POINT('Ctrl Pts',(-3.8084975719434,3.11284580055319,10.0445247538165));
#24127=CARTESIAN_POINT('Ctrl Pts',(-3.71073577283674,3.22891290696235,10.0358901827421));
#24128=CARTESIAN_POINT('Ctrl Pts',(-3.65833223703798,3.28816721094897,10.0313792131835));
#24129=CARTESIAN_POINT('Ctrl Pts',(-3.48480347951792,3.47509602234596,10.0168054996788));
#24130=CARTESIAN_POINT('Ctrl Pts',(-3.35824921395468,3.59754218673306,10.006716469207));
#24131=CARTESIAN_POINT('Ctrl Pts',(-3.17975157962301,3.75260178478131,9.99321831354768));
#24132=CARTESIAN_POINT('Ctrl Pts',(-3.13336924390907,3.79141630137753,9.98977269901734));
#24133=CARTESIAN_POINT('Ctrl Pts',(-3.05767059483008,3.85242572894921,9.9842521917851));
#24134=CARTESIAN_POINT('Ctrl Pts',(-3.02880105558526,3.87516421195266,9.98217044645512));
#24135=CARTESIAN_POINT('Ctrl Pts',(-2.95197167751795,3.93429414144715,9.97669093754206));
#24136=CARTESIAN_POINT('Ctrl Pts',(-2.90359380173349,3.97013228247349,9.97330074030465));
#24137=CARTESIAN_POINT('Ctrl Pts',(-2.78066560570278,4.05774793137651,9.96481632029374));
#24138=CARTESIAN_POINT('Ctrl Pts',(-2.70531717305857,4.10836690848389,9.95973195871955));
#24139=CARTESIAN_POINT('Ctrl Pts',(-2.49171174242977,4.24344096399808,9.94557327542539));
#24140=CARTESIAN_POINT('Ctrl Pts',(-2.35062077042142,4.32319324756917,9.93650494876144));
#24141=CARTESIAN_POINT('Ctrl Pts',(-2.14027416845257,4.42874622856134,9.92324995664961));
#24142=CARTESIAN_POINT('Ctrl Pts',(-2.07396703265842,4.46018242401888,9.91910864883493));
#24143=CARTESIAN_POINT('Ctrl Pts',(-1.94243041748114,4.51897627139127,9.91095448332424));
#24144=CARTESIAN_POINT('Ctrl Pts',(-1.87726467116537,4.54643373078613,9.90694338686368));
#24145=CARTESIAN_POINT('Ctrl Pts',(-1.66178531833791,4.63180264343459,9.89376297661376));
#24146=CARTESIAN_POINT('Ctrl Pts',(-1.50921829070979,4.68373623425784,9.88455750945212));
#24147=CARTESIAN_POINT('Ctrl Pts',(-1.21893522283393,4.76688901259839,9.86727257949013));
#24148=CARTESIAN_POINT('Ctrl Pts',(-1.08188386701515,4.79985019243221,9.85920517059126));
#24149=CARTESIAN_POINT('Ctrl Pts',(-0.902948178720308,4.83483028412233,
9.84882814445847));
#24150=CARTESIAN_POINT('Ctrl Pts',(-0.86219127418395,4.8422645066816,9.84647502193498));
#24151=CARTESIAN_POINT('Ctrl Pts',(-0.779592497046392,4.85625492379467,
9.84172959527507));
#24152=CARTESIAN_POINT('Ctrl Pts',(-0.737750069124316,4.86278739384556,
9.8393377143324));
#24153=CARTESIAN_POINT('Ctrl Pts',(-0.587648426827218,4.88423937604565,
9.83079066061389));
#24154=CARTESIAN_POINT('Ctrl Pts',(-0.478982327106876,4.89609041575107,
9.82466437227494));
#24155=CARTESIAN_POINT('Ctrl Pts',(-0.330168538068199,4.9073178262427,9.81630216199654));
#24156=CARTESIAN_POINT('Ctrl Pts',(-0.290291022566702,4.90983814755577,
9.81406410772107));
#24157=CARTESIAN_POINT('Ctrl Pts',(-0.0986536452562509,4.91960703995444,
9.80331377585089));
#24158=CARTESIAN_POINT('Ctrl Pts',(0.0533552664461227,4.92030673605178,
9.79479868821307));
#24159=CARTESIAN_POINT('Ctrl Pts',(0.268532306588229,4.91132341200776,9.78265922315142));
#24160=CARTESIAN_POINT('Ctrl Pts',(0.33185605757132,4.90745134519767,9.77907658964663));
#24161=CARTESIAN_POINT('Ctrl Pts',(0.466398097436955,4.89660844019906,9.77143581988103));
#24162=CARTESIAN_POINT('Ctrl Pts',(0.537574988305485,4.8893061240547,9.76737630607454));
#24163=CARTESIAN_POINT('Ctrl Pts',(0.767508788425144,4.86063460104369,9.75419596892673));
#24164=CARTESIAN_POINT('Ctrl Pts',(0.925386064185252,4.83306299749805,9.74504012016212));
#24165=CARTESIAN_POINT('Ctrl Pts',(1.2156461660436,4.76762618650111,9.72800752022895));
#24166=CARTESIAN_POINT('Ctrl Pts',(1.34833465840257,4.73181247639205,9.7201423867171));
#24167=CARTESIAN_POINT('Ctrl Pts',(1.51903665017495,4.67797417520116,9.70995452050717));
#24168=CARTESIAN_POINT('Ctrl Pts',(1.55856274125989,4.66495412251792,9.70759072700317));
#24169=CARTESIAN_POINT('Ctrl Pts',(1.6377799961365,4.63774041399282,9.70284589577237));
#24170=CARTESIAN_POINT('Ctrl Pts',(1.6774635113954,4.62353497732534,9.70046518518342));
#24171=CARTESIAN_POINT('Ctrl Pts',(1.76485036628183,4.5909800755694,9.69520829968754));
#24172=CARTESIAN_POINT('Ctrl Pts',(1.81246023038522,4.5723935578756,9.69233467556155));
#24173=CARTESIAN_POINT('Ctrl Pts',(1.97125812018535,4.50753007351493,9.68270283866493));
#24174=CARTESIAN_POINT('Ctrl Pts',(2.08103441066348,4.45791228447537,9.67596501276302));
#24175=CARTESIAN_POINT('Ctrl Pts',(2.30752289452494,4.34535088683849,9.6617912982349));
#24176=CARTESIAN_POINT('Ctrl Pts',(2.42373462353738,4.28161722855317,9.65435853704751));
#24177=CARTESIAN_POINT('Ctrl Pts',(2.5912268385222,4.18075346230769,9.64333613268098));
#24178=CARTESIAN_POINT('Ctrl Pts',(2.64459302378546,4.14720190886849,9.63977583477576));
#24179=CARTESIAN_POINT('Ctrl Pts',(2.75761229834963,4.07307744539168,9.63212383175679));
#24180=CARTESIAN_POINT('Ctrl Pts',(2.81704740274419,4.03219905661168,9.62803048150884));
#24181=CARTESIAN_POINT('Ctrl Pts',(2.9388209033491,3.94443848725308,9.61949101454432));
#24182=CARTESIAN_POINT('Ctrl Pts',(3.00098668885025,3.89735063949391,9.61504438220197));
#24183=CARTESIAN_POINT('Ctrl Pts',(3.19312877377477,3.74448754513546,9.60101693677749));
#24184=CARTESIAN_POINT('Ctrl Pts',(3.31883438164156,3.63353773855162,9.59141218229546));
#24185=CARTESIAN_POINT('Ctrl Pts',(3.48716765548531,3.46892681650276,9.57796187969366));
#24186=CARTESIAN_POINT('Ctrl Pts',(3.53471622064002,3.42046384557414,9.5740911050927));
#24187=CARTESIAN_POINT('Ctrl Pts',(3.60658289763835,3.34411561798373,9.56813452784262));
#24188=CARTESIAN_POINT('Ctrl Pts',(3.63161496112999,3.31691457348638,9.56603922599912));
#24189=CARTESIAN_POINT('Ctrl Pts',(3.69288285178246,3.24881283710017,9.56085917029369));
#24190=CARTESIAN_POINT('Ctrl Pts',(3.72874823813457,3.207585585262,9.55777985300247));
#24191=CARTESIAN_POINT('Ctrl Pts',(3.86219353239414,3.048926709225,9.54611960073225));
#24192=CARTESIAN_POINT('Ctrl Pts',(3.95497424984526,2.92757105254055,9.53758432389728));
#24193=CARTESIAN_POINT('Ctrl Pts',(4.11281148504426,2.69989441241424,9.52205654350608));
#24194=CARTESIAN_POINT('Ctrl Pts',(4.17976045802128,2.59504337713921,9.51507770187174));
#24195=CARTESIAN_POINT('Ctrl Pts',(4.27460809724857,2.43328937455458,9.50450715953463));
#24196=CARTESIAN_POINT('Ctrl Pts',(4.30550067155555,2.37820003893879,9.50094008003325));
#24197=CARTESIAN_POINT('Ctrl Pts',(4.36929557217262,2.25911810590922,9.49329206617317));
#24198=CARTESIAN_POINT('Ctrl Pts',(4.40187185366961,2.19496752498877,9.4892095707269));
#24199=CARTESIAN_POINT('Ctrl Pts',(4.45043430535197,2.09390366526493,9.48283094233865));
#24200=CARTESIAN_POINT('Ctrl Pts',(4.46739491706761,2.05746948839183,9.48054193859886));
#24201=CARTESIAN_POINT('Ctrl Pts',(4.56382874449322,1.8434980235541,9.46715853316292));
#24202=CARTESIAN_POINT('Ctrl Pts',(4.63315972021679,1.6615799132947,9.45600931320434));
#24203=CARTESIAN_POINT('Ctrl Pts',(4.71431345957692,1.40363547551885,9.4405524479604));
#24204=CARTESIAN_POINT('Ctrl Pts',(4.73541343816889,1.33071549279272,9.43622170977432));
#24205=CARTESIAN_POINT('Ctrl Pts',(4.76438994797274,1.22113616544467,9.42977999246851));
#24206=CARTESIAN_POINT('Ctrl Pts',(4.77354873962446,1.18482808786651,9.42765652133304));
#24207=CARTESIAN_POINT('Ctrl Pts',(4.79421222192891,1.09878035466701,9.42265047384854));
#24208=CARTESIAN_POINT('Ctrl Pts',(4.80535886023037,1.0489592024184,9.41977195675482));
#24209=CARTESIAN_POINT('Ctrl Pts',(4.8464905393913,0.8506766230049,9.4083763568927));
#24210=CARTESIAN_POINT('Ctrl Pts',(4.87038693639682,0.7010371380656,9.39990800673258));
#24211=CARTESIAN_POINT('Ctrl Pts',(4.88961768096841,0.53031677156654,9.39028027568745));
#24212=CARTESIAN_POINT('Ctrl Pts',(4.89176947319828,0.510086624099066,9.38913998010303));
#24213=CARTESIAN_POINT('Ctrl Pts',(4.90584185316167,0.369496168752397,9.38121806222294));
#24214=CARTESIAN_POINT('Ctrl Pts',(4.91344445156743,0.248746447774333,9.37442629238887));
#24215=CARTESIAN_POINT('Ctrl Pts',(4.91835528027675,0.0598821449223939,
9.36376973764994));
#24216=CARTESIAN_POINT('Ctrl Pts',(4.91871311481507,-0.00810509747336468,
9.3599270785901));
#24217=CARTESIAN_POINT('Ctrl Pts',(4.91646504737613,-0.153420773411911,
9.35169152091769));
#24218=CARTESIAN_POINT('Ctrl Pts',(4.91344405681667,-0.230724510835193,
9.34729689970407));
#24219=CARTESIAN_POINT('Ctrl Pts',(4.90239795447109,-0.406809796795339,
9.33724816159998));
#24220=CARTESIAN_POINT('Ctrl Pts',(4.89320803648174,-0.505484654148446,
9.33158907696805));
#24221=CARTESIAN_POINT('Ctrl Pts',(4.85824986835514,-0.788075728287074,
9.31529934921482));
#24222=CARTESIAN_POINT('Ctrl Pts',(4.82503975880103,-0.970900296213722,
9.30465420832144));
#24223=CARTESIAN_POINT('Ctrl Pts',(4.77333716600311,-1.18561077336241,9.29209405504729));
#24224=CARTESIAN_POINT('Ctrl Pts',(4.76473470897244,-1.21972283727005,9.29009701520104));
#24225=CARTESIAN_POINT('Ctrl Pts',(4.74472702463483,-1.29561727175221,9.2856519460565));
#24226=CARTESIAN_POINT('Ctrl Pts',(4.73313436642068,-1.3373472927828,9.28320634162732));
#24227=CARTESIAN_POINT('Ctrl Pts',(4.71327999300418,-1.40532252077077,9.27921545059115));
#24228=CARTESIAN_POINT('Ctrl Pts',(4.70534660956014,-1.43166091473649,9.27766732444666));
#24229=CARTESIAN_POINT('Ctrl Pts',(4.65108945065757,-1.60646771172044,9.26737600368524));
#24230=CARTESIAN_POINT('Ctrl Pts',(4.5979663373299,-1.75273435792148,9.2586827538543));
#24231=CARTESIAN_POINT('Ctrl Pts',(4.49120130920548,-2.00824017091746,9.24315915279642));
#24232=CARTESIAN_POINT('Ctrl Pts',(4.44027057061565,-2.11846985443216,9.23634479207004));
#24233=CARTESIAN_POINT('Ctrl Pts',(4.35700930345676,-2.28244642931361,9.22597494628348));
#24234=CARTESIAN_POINT('Ctrl Pts',(4.32764382451953,-2.33764637967326,9.22244282289246));
#24235=CARTESIAN_POINT('Ctrl Pts',(4.26171453812721,-2.45607509110152,9.21476756203614));
#24236=CARTESIAN_POINT('Ctrl Pts',(4.22477854412438,-2.5190795427007,9.21062239753048));
#24237=CARTESIAN_POINT('Ctrl Pts',(4.14454916263361,-2.64920184584863,9.20192360513128));
#24238=CARTESIAN_POINT('Ctrl Pts',(4.10099606986845,-2.7161349819613,9.19736923545529));
#24239=CARTESIAN_POINT('Ctrl Pts',(3.96186183938436,-2.91897817504703,9.1833132734703));
#24240=CARTESIAN_POINT('Ctrl Pts',(3.86100947263396,-3.051129064422,9.17378998380648));
#24241=CARTESIAN_POINT('Ctrl Pts',(3.71151622078594,-3.22770587482084,9.16057585216328));
#24242=CARTESIAN_POINT('Ctrl Pts',(3.6683820313404,-3.27664634849965,9.15685750750201));
#24243=CARTESIAN_POINT('Ctrl Pts',(3.59937732546918,-3.35186869541264,9.15105939842205));
#24244=CARTESIAN_POINT('Ctrl Pts',(3.57416336947065,-3.378741945967,9.14897109346012));
#24245=CARTESIAN_POINT('Ctrl Pts',(3.50967140968571,-3.44594817282243,9.14370486038983));
#24246=CARTESIAN_POINT('Ctrl Pts',(3.46999849901174,-3.48589482642406,9.14053300034068));
#24247=CARTESIAN_POINT('Ctrl Pts',(3.37172487137077,-3.58150601801696,9.13282313638277));
#24248=CARTESIAN_POINT('Ctrl Pts',(3.31242098542295,-3.63642425064118,9.12829285936765));
#24249=CARTESIAN_POINT('Ctrl Pts',(3.10803220043903,-3.81654765738064,9.11302768590466));
#24250=CARTESIAN_POINT('Ctrl Pts',(2.95699421758855,-3.93472797984795,9.10230903105011));
#24251=CARTESIAN_POINT('Ctrl Pts',(2.74728643826898,-4.07990504647664,9.08793228076171));
#24252=CARTESIAN_POINT('Ctrl Pts',(2.69443077468446,-4.11500311712939,9.08434934050108));
#24253=CARTESIAN_POINT('Ctrl Pts',(2.58056377755479,-4.18748026047541,9.07670868913933));
#24254=CARTESIAN_POINT('Ctrl Pts',(2.51938587796649,-4.22457039007471,9.07264960399454));
#24255=CARTESIAN_POINT('Ctrl Pts',(2.31973212503026,-4.3397340932608,9.0595391116142));
#24256=CARTESIAN_POINT('Ctrl Pts',(2.17827523823209,-4.41243300006857,9.05045337362229));
#24257=CARTESIAN_POINT('Ctrl Pts',(1.90714666265894,-4.53555365342887,9.03340776031207));
#24258=CARTESIAN_POINT('Ctrl Pts',(1.77836975984092,-4.58757637019983,9.02545929719546));
#24259=CARTESIAN_POINT('Ctrl Pts',(1.60842579967038,-4.64799687394563,9.01519340198725));
#24260=CARTESIAN_POINT('Ctrl Pts',(1.5691124717664,-4.66141551460841,9.01283391216292));
#24261=CARTESIAN_POINT('Ctrl Pts',(1.48950075017981,-4.687467727895,9.00808889272457));
#24262=CARTESIAN_POINT('Ctrl Pts',(1.44920012969174,-4.70008353377655,9.00570372866885));
#24263=CARTESIAN_POINT('Ctrl Pts',(1.35963656085164,-4.72685924453157,9.00043418042529));
#24264=CARTESIAN_POINT('Ctrl Pts',(1.31030458450458,-4.74077123014954,8.99755236758017));
#24265=CARTESIAN_POINT('Ctrl Pts',(1.14355802989694,-4.78499336532816,8.98786588846651));
#24266=CARTESIAN_POINT('Ctrl Pts',(1.02524230931461,-4.81173200576692,8.98108183534108));
#24267=CARTESIAN_POINT('Ctrl Pts',(0.77741366775612,-4.85818300742241,8.96695111412338));
#24268=CARTESIAN_POINT('Ctrl Pts',(0.647858156546125,-4.87715012594922,
8.95960791547125));
#24269=CARTESIAN_POINT('Ctrl Pts',(0.449287006469579,-4.89816876755121,
8.94835113327228));
#24270=CARTESIAN_POINT('Ctrl Pts',(0.380728321367008,-4.90397409206418,
8.94446462303749));
#24271=CARTESIAN_POINT('Ctrl Pts',(0.252993107993749,-4.91209546442165,
8.93721560062547));
#24272=CARTESIAN_POINT('Ctrl Pts',(0.193852650364851,-4.91478467727583,
8.9338562559431));
#24273=CARTESIAN_POINT('Ctrl Pts',(0.0602279577463912,-4.91844514999225,
8.92625505543547));
#24274=CARTESIAN_POINT('Ctrl Pts',(-0.0142587363162196,-4.91879320934879,
8.92201016832599));
#24275=CARTESIAN_POINT('Ctrl Pts',(-0.232898185613029,-4.91484836499791,
8.90952316325364));
#24276=CARTESIAN_POINT('Ctrl Pts',(-0.376887746122749,-4.90590779622597,
8.90126317323262));
#24277=CARTESIAN_POINT('Ctrl Pts',(-0.608333217285808,-4.88128627954514,
8.88794769081639));
#24278=CARTESIAN_POINT('Ctrl Pts',(-0.69612303946579,-4.86954187079948,
8.88288854422808));
#24279=CARTESIAN_POINT('Ctrl Pts',(-0.822761046317827,-4.84910558664577,
8.87559057875893));
#24280=CARTESIAN_POINT('Ctrl Pts',(-0.861895873358112,-4.84230278827586,
8.87333535806386));
#24281=CARTESIAN_POINT('Ctrl Pts',(-0.937738991330432,-4.8281704090436,
8.86896672169268));
#24282=CARTESIAN_POINT('Ctrl Pts',(-0.974454414857338,-4.82089437205882,
8.8668525822506));
#24283=CARTESIAN_POINT('Ctrl Pts',(-1.01444164373047,-4.81249446639752,
8.86454879001763));
#24284=CARTESIAN_POINT('Ctrl Pts',(-1.01779910481413,-4.81178551266636,
8.86435534630946));
#24285=CARTESIAN_POINT('Ctrl Pts',(-1.02509046355174,-4.81023791333416,
8.86393522294324));
#24286=CARTESIAN_POINT('Ctrl Pts',(-1.02902408054916,-4.80939795432142,
8.86370855533334));
#24287=CARTESIAN_POINT('Ctrl Pts',(-1.0376559299184,-4.80754369046655,8.86321112238485));
#24288=CARTESIAN_POINT('Ctrl Pts',(-1.04235371571048,-4.80652732188719,
8.86294037534294));
#24289=CARTESIAN_POINT('Ctrl Pts',(-1.10521165810498,-4.79283148309207,
8.85931730671267));
#24290=CARTESIAN_POINT('Ctrl Pts',(-1.16313882040914,-4.77910395441256,
8.8559739986206));
#24291=CARTESIAN_POINT('Ctrl Pts',(-1.39546955289134,-4.71957194859762,
8.8425194767058));
#24292=CARTESIAN_POINT('Ctrl Pts',(-1.56754243727073,-4.66524439092781,
8.83244572881302));
#24293=CARTESIAN_POINT('Ctrl Pts',(-1.80989581021524,-4.57380118784936,
8.81788812726857));
#24294=CARTESIAN_POINT('Ctrl Pts',(-1.88287053067865,-4.54424675062605,
8.81345557348258));
#24295=CARTESIAN_POINT('Ctrl Pts',(-2.00224869747087,-4.49252968777582,
8.80610924268411));
#24296=CARTESIAN_POINT('Ctrl Pts',(-2.0490703190493,-4.47136820339269,8.80320318619195));
#24297=CARTESIAN_POINT('Ctrl Pts',(-2.16399586378667,-4.41724220346222,
8.79600461437046));
#24298=CARTESIAN_POINT('Ctrl Pts',(-2.23168673167228,-4.38343255111028,
8.79170666911089));
#24299=CARTESIAN_POINT('Ctrl Pts',(-2.3760935202413,-4.30709322380119,8.78240432795874));
#24300=CARTESIAN_POINT('Ctrl Pts',(-2.45250641415723,-4.26404555934227,
8.77739788200632));
#24301=CARTESIAN_POINT('Ctrl Pts',(-2.67304584173115,-4.13191322621563,
8.76269560726573));
#24302=CARTESIAN_POINT('Ctrl Pts',(-2.81376957642028,-4.03739793114908,
8.7529838023842));
#24303=CARTESIAN_POINT('Ctrl Pts',(-2.99032344619345,-3.90509566256631,
8.74040324934802));
#24304=CARTESIAN_POINT('Ctrl Pts',(-3.03082928388353,-3.87374242616237,
8.73748849438426));
#24305=CARTESIAN_POINT('Ctrl Pts',(-3.09805012838817,-3.82001074145402,
8.73260633175094));
#24306=CARTESIAN_POINT('Ctrl Pts',(-3.12503001080965,-3.79797105276432,
8.73063461283748));
#24307=CARTESIAN_POINT('Ctrl Pts',(-3.15839488539357,-3.77011925510705,
8.72817969360587));
#24308=CARTESIAN_POINT('Ctrl Pts',(-3.16500144492923,-3.76457478393626,
8.7276927653901));
#24309=CARTESIAN_POINT('Ctrl Pts',(-3.17709761395905,-3.75436887875197,
8.7267996626337));
#24310=CARTESIAN_POINT('Ctrl Pts',(-3.18259163201268,-3.7497127130559,8.72639342219237));
#24311=CARTESIAN_POINT('Ctrl Pts',(-3.1959067632568,-3.73837782969405,8.72540738492953));
#24312=CARTESIAN_POINT('Ctrl Pts',(-3.20371719853828,-3.73168660921981,
8.72482774167346));
#24313=CARTESIAN_POINT('Ctrl Pts',(-3.22578974253956,-3.7126566296321,8.72318599332096));
#24314=CARTESIAN_POINT('Ctrl Pts',(-3.24000197548396,-3.70026024963596,
8.72212454007649));
#24315=CARTESIAN_POINT('Ctrl Pts',(-3.3115807945471,-3.63709825733186,8.716755333729));
#24316=CARTESIAN_POINT('Ctrl Pts',(-3.36782737576097,-3.58507879932278,
8.71245980224359));
#24317=CARTESIAN_POINT('Ctrl Pts',(-3.56773108643695,-3.39134072243121,
8.69685919985536));
#24318=CARTESIAN_POINT('Ctrl Pts',(-3.70384552709633,-3.24213265198416,
8.68557681518277));
#24319=CARTESIAN_POINT('Ctrl Pts',(-3.87347026614292,-3.03152174189137,
8.67033112404397));
#24320=CARTESIAN_POINT('Ctrl Pts',(-3.91540710032853,-2.97716023660427,
8.66645268296599));
#24321=CARTESIAN_POINT('Ctrl Pts',(-3.96012541627941,-2.91661337612306,
8.66218946709337));
#24322=CARTESIAN_POINT('Ctrl Pts',(-3.96404812423363,-2.91127967860756,
8.66181438487778));
#24323=CARTESIAN_POINT('Ctrl Pts',(-3.97149017706006,-2.90111780747741,
8.66110066374459));
#24324=CARTESIAN_POINT('Ctrl Pts',(-3.97501151818084,-2.89629110926061,
8.66076204140052));
#24325=CARTESIAN_POINT('Ctrl Pts',(-3.98378491041336,-2.8842192922372,8.65991607690125));
#24326=CARTESIAN_POINT('Ctrl Pts',(-3.98902599704824,-2.87696623767165,
8.65940864941668));
#24327=CARTESIAN_POINT('Ctrl Pts',(-4.04368087443625,-2.80089376474113,
8.65409538453157));
#24328=CARTESIAN_POINT('Ctrl Pts',(-4.09132792552962,-2.73082340198061,
8.64927628126284));
#24329=CARTESIAN_POINT('Ctrl Pts',(-4.1952015255127,-2.56924026783685,8.63832208188501));
#24330=CARTESIAN_POINT('Ctrl Pts',(-4.2502886706651,-2.47704608638311,8.63218221578728));
#24331=CARTESIAN_POINT('Ctrl Pts',(-4.36272849798232,-2.27405560456766,
8.6188997409065));
#24332=CARTESIAN_POINT('Ctrl Pts',(-4.41897411213275,-2.16272905236547,
8.61175950152938));
#24333=CARTESIAN_POINT('Ctrl Pts',(-4.49239050723868,-2.00256420936867,
8.60171152332366));
#24334=CARTESIAN_POINT('Ctrl Pts',(-4.51311571000412,-1.95540853947422,
8.59878003938712));
#24335=CARTESIAN_POINT('Ctrl Pts',(-4.54659222573431,-1.87587112165083,
8.59388355267721));
#24336=CARTESIAN_POINT('Ctrl Pts',(-4.55974727004699,-1.84366433781596,
8.59191417461849));
#24337=CARTESIAN_POINT('Ctrl Pts',(-4.59539094156781,-1.75368421923288,
8.58644662141081));
#24338=CARTESIAN_POINT('Ctrl Pts',(-4.61713065241062,-1.6956211016924,8.58295709963222));
#24339=CARTESIAN_POINT('Ctrl Pts',(-4.67130923271195,-1.54214354480996,
8.57381280496334));
#24340=CARTESIAN_POINT('Ctrl Pts',(-4.70192352877415,-1.44611617359454,
8.5681705738051));
#24341=CARTESIAN_POINT('Ctrl Pts',(-4.77359076766381,-1.19489250333297,
8.55353498666965));
#24342=CARTESIAN_POINT('Ctrl Pts',(-4.81003494102768,-1.0385084848992,8.54454372832498));
#24343=CARTESIAN_POINT('Ctrl Pts',(-4.85008662028798,-0.818436494833083,
8.53193411522017));
#24344=CARTESIAN_POINT('Ctrl Pts',(-4.86020445934079,-0.756036392071409,
8.52836400066404));
#24345=CARTESIAN_POINT('Ctrl Pts',(-4.87801276479547,-0.6309955321278,8.52121380370745));
#24346=CARTESIAN_POINT('Ctrl Pts',(-4.88570595530992,-0.568367050155467,
8.51763441550896));
#24347=CARTESIAN_POINT('Ctrl Pts',(-4.89819102465612,-0.447563356708912,
8.51072956049755));
#24348=CARTESIAN_POINT('Ctrl Pts',(-4.90315642882732,-0.389416525542466,
8.50740577200676));
#24349=CARTESIAN_POINT('Ctrl Pts',(-4.91452940169788,-0.220911331953344,
8.49777044851229));
#24350=CARTESIAN_POINT('Ctrl Pts',(-4.91825281349053,-0.110408334943236,
8.49144711962447));
#24351=CARTESIAN_POINT('Ctrl Pts',(-4.91824999840495,0.00012525870399141,
8.48511971591668));
#24352=CARTESIAN_POINT('Ctrl Pts',(-4.76403458704967,1.22194824599671,8.41520471722259));
#24353=CARTESIAN_POINT('Ctrl Pts',(-4.79982248259297,1.0824212466131,8.42336126929135));
#24354=CARTESIAN_POINT('Ctrl Pts',(-4.82947364947956,0.941332311715187,
8.43151782136011));
#24355=CARTESIAN_POINT('Ctrl Pts',(-4.85287602958132,0.799235449673663,
8.43967437342887));
#24356=CARTESIAN_POINT('Ctrl Pts',(-4.86756266525287,0.71005969772877,8.44479318220169));
#24357=CARTESIAN_POINT('Ctrl Pts',(-4.87978926605988,0.620487210156302,
8.44991199097452));
#24358=CARTESIAN_POINT('Ctrl Pts',(-4.88953849541565,0.530656540851442,
8.45503079974735));
#24359=CARTESIAN_POINT('Ctrl Pts',(-4.90598317603319,0.379133111412091,
8.46366503865378));
#24360=CARTESIAN_POINT('Ctrl Pts',(-4.91538074332051,0.226839147476468,
8.47229927756021));
#24361=CARTESIAN_POINT('Ctrl Pts',(-4.9176871206407,0.0744072979253948,
8.48093351646665));
#24362=CARTESIAN_POINT('Ctrl Pts',(-4.91806171606027,0.0496497389009686,
8.48233586564752));
#24363=CARTESIAN_POINT('Ctrl Pts',(-4.91824936172107,0.0248885507464108,
8.4837382148284));
#24364=CARTESIAN_POINT('Ctrl Pts',(-4.91824999837441,0.000126452135718109,
8.48514056400927));
#24365=CARTESIAN_POINT('',(-4.91787035223228,-3.97720175591356E-5,8.1398455264357));
#24366=CARTESIAN_POINT('Ctrl Pts',(-4.76403458713635,1.22194824565879,8.07015829796832));
#24367=CARTESIAN_POINT('Ctrl Pts',(-4.7829881060944,1.14805377411723,8.07445983792208));
#24368=CARTESIAN_POINT('Ctrl Pts',(-4.80022027915519,1.07372647371595,8.07874466348763));
#24369=CARTESIAN_POINT('Ctrl Pts',(-4.86183194194516,0.776733074723372,
8.09575746200658));
#24370=CARTESIAN_POINT('Ctrl Pts',(-4.89249982611999,0.551514877477385,
8.10843153398002));
#24371=CARTESIAN_POINT('Ctrl Pts',(-4.91127259025011,0.268034296101974,
8.12444404401394));
#24372=CARTESIAN_POINT('Ctrl Pts',(-4.91405238549001,0.21102112114891,8.12766659502292));
#24373=CARTESIAN_POINT('Ctrl Pts',(-4.91744686864092,0.102646600721967,
8.13380112341401));
#24374=CARTESIAN_POINT('Ctrl Pts',(-4.91825054455029,0.0512986358838704,
8.13671144365306));
#24375=CARTESIAN_POINT('Ctrl Pts',(-4.91824999972317,-5.2182147148742E-5,
8.13962702323731));
#24376=CARTESIAN_POINT('Ctrl Pts',(-4.91784618449604,-3.89820090755666E-5,
8.13985943599073));
#24377=CARTESIAN_POINT('Ctrl Pts',(-4.91794771965564,-0.366944504507531,
8.16063286907332));
#24378=CARTESIAN_POINT('Ctrl Pts',(-4.78704988297834,-1.55224723866423,
8.22774630066009));
#24379=CARTESIAN_POINT('Ctrl Pts',(-3.84485907817879,-3.39191518737209,
8.34119973075105));
#24380=CARTESIAN_POINT('Ctrl Pts',(-1.75217326669541,-4.81849756800367,
8.48021972626356));
#24381=CARTESIAN_POINT('Ctrl Pts',(0.768055611337776,-5.06933137082908,
8.61923972177608));
#24382=CARTESIAN_POINT('Ctrl Pts',(3.10087331400732,-4.08321131707098,8.75825971728859));
#24383=CARTESIAN_POINT('Ctrl Pts',(4.67705529414154,-2.10075789774117,8.89727971280111));
#24384=CARTESIAN_POINT('Ctrl Pts',(5.11200164370846,0.394295782505144,9.03629970831364));
#24385=CARTESIAN_POINT('Ctrl Pts',(4.29958227865011,2.79313841377351,9.17531970382614));
#24386=CARTESIAN_POINT('Ctrl Pts',(2.43803345405823,4.51043488438445,9.31433969933867));
#24387=CARTESIAN_POINT('Ctrl Pts',(-0.0184133290357824,5.12715232060577,
9.45335969485118));
#24388=CARTESIAN_POINT('Ctrl Pts',(-2.47036712544234,4.49280716645095,9.5923796903637));
#24389=CARTESIAN_POINT('Ctrl Pts',(-4.09563866263082,2.97172585056254,9.71456732471902));
#24390=CARTESIAN_POINT('Ctrl Pts',(-4.63391221881488,1.72658135255771,9.79041496057018));
#24391=CARTESIAN_POINT('Ctrl Pts',(-4.76374494423105,1.22187361077196,9.81992259791717));
#24392=CARTESIAN_POINT('Origin',(0.,0.,-3.23514056400928));
#24393=CARTESIAN_POINT('',(-4.76403457734943,1.22194828381523,11.9150196727617));
#24394=CARTESIAN_POINT('',(-4.76403460025573,1.22194819451,11.5699436565254));
#24395=CARTESIAN_POINT('',(-4.76403458704967,1.22194824599672,-3.23514056400928));
#24396=CARTESIAN_POINT('Ctrl Pts',(-4.76403457734944,1.22194828381523,11.9150196727617));
#24397=CARTESIAN_POINT('Ctrl Pts',(-4.7244905674948,1.37611931770409,11.9060746123167));
#24398=CARTESIAN_POINT('Ctrl Pts',(-4.67747937823696,1.52830606459855,11.8971783354818));
#24399=CARTESIAN_POINT('Ctrl Pts',(-4.60398021861279,1.73081177289111,11.8850980175744));
#24400=CARTESIAN_POINT('Ctrl Pts',(-4.58389655736411,1.78332149431695,11.8819432183635));
#24401=CARTESIAN_POINT('Ctrl Pts',(-4.53123569457204,1.91423427479359,11.8740121046384));
#24402=CARTESIAN_POINT('Ctrl Pts',(-4.49752056546728,1.99215920738576,11.8692307682782));
#24403=CARTESIAN_POINT('Ctrl Pts',(-4.43562557068445,2.12562490050214,11.860918742926));
#24404=CARTESIAN_POINT('Ctrl Pts',(-4.40837645993941,2.18157564673165,11.8573957671926));
#24405=CARTESIAN_POINT('Ctrl Pts',(-4.33998825313583,2.31548095496047,11.8488642653837));
#24406=CARTESIAN_POINT('Ctrl Pts',(-4.29780126794634,2.392875691752,11.8438491696215));
#24407=CARTESIAN_POINT('Ctrl Pts',(-4.16496665594137,2.62171252167947,11.8287537188025));
#24408=CARTESIAN_POINT('Ctrl Pts',(-4.06822584951849,2.76945148479429,11.8186415546403));
#24409=CARTESIAN_POINT('Ctrl Pts',(-3.92877394929637,2.95929213479102,11.8051718261099));
#24410=CARTESIAN_POINT('Ctrl Pts',(-3.89293631351057,3.00628036340595,11.8017969201398));
#24411=CARTESIAN_POINT('Ctrl Pts',(-3.83346821661113,3.08140438852422,11.7963378933445));
#24412=CARTESIAN_POINT('Ctrl Pts',(-3.81035401818076,3.10994113480862,11.7942489473734));
#24413=CARTESIAN_POINT('Ctrl Pts',(-3.76373841711918,3.16619272151378,11.7901020555366));
#24414=CARTESIAN_POINT('Ctrl Pts',(-3.74024528769188,3.193911151498,11.7880445167892));
#24415=CARTESIAN_POINT('Ctrl Pts',(-3.67450264140116,3.26975753757497,11.7823730628181));
#24416=CARTESIAN_POINT('Ctrl Pts',(-3.63161692229767,3.31732462927569,11.7787683406521));
#24417=CARTESIAN_POINT('Ctrl Pts',(-3.47030442281233,3.48936749830215,11.7655185374147));
#24418=CARTESIAN_POINT('Ctrl Pts',(-3.3463083419578,3.60845108683862,11.7559215004634));
#24419=CARTESIAN_POINT('Ctrl Pts',(-3.15691230812849,3.77216879101442,11.7418745563128));
#24420=CARTESIAN_POINT('Ctrl Pts',(-3.09626749269752,3.82210415470926,11.7374611812107));
#24421=CARTESIAN_POINT('Ctrl Pts',(-2.97951976547875,3.91363226063336,11.7291039663979));
#24422=CARTESIAN_POINT('Ctrl Pts',(-2.92367608697119,3.95552442793255,11.7251635355641));
#24423=CARTESIAN_POINT('Ctrl Pts',(-2.81069941748672,4.03657605552683,11.7172941763925));
#24424=CARTESIAN_POINT('Ctrl Pts',(-2.75359303278346,4.07574566582514,11.7133662917186));
#24425=CARTESIAN_POINT('Ctrl Pts',(-2.57174881594076,4.1949070333938,11.7010037259994));
#24426=CARTESIAN_POINT('Ctrl Pts',(-2.44421331635595,4.27047506302232,11.6925395973986));
#24427=CARTESIAN_POINT('Ctrl Pts',(-2.21836016760169,4.390862739709,11.6778912930164));
#24428=CARTESIAN_POINT('Ctrl Pts',(-2.12161647647625,4.43841650664979,11.6717193035401));
#24429=CARTESIAN_POINT('Ctrl Pts',(-1.97897522108829,4.50280074747896,11.6627802138757));
#24430=CARTESIAN_POINT('Ctrl Pts',(-1.93426603593116,4.52218668965104,11.6600008187116));
#24431=CARTESIAN_POINT('Ctrl Pts',(-1.85392462957113,4.55561330381255,11.6550488779386));
#24432=CARTESIAN_POINT('Ctrl Pts',(-1.81840253394566,4.56990824545826,11.6528740641586));
#24433=CARTESIAN_POINT('Ctrl Pts',(-1.74951436905888,4.59670008705208,11.6486862822818));
#24434=CARTESIAN_POINT('Ctrl Pts',(-1.71617230597098,4.6092520939032,11.6466727668808));
#24435=CARTESIAN_POINT('Ctrl Pts',(-1.6072407171445,4.64891479299054,11.6401325628829));
#24436=CARTESIAN_POINT('Ctrl Pts',(-1.5311225431248,4.67453692599931,11.6356216086757));
#24437=CARTESIAN_POINT('Ctrl Pts',(-1.31035813489288,4.7428772149839,11.6226586322734));
#24438=CARTESIAN_POINT('Ctrl Pts',(-1.16433115678242,4.78082165324332,11.614228115212));
#24439=CARTESIAN_POINT('Ctrl Pts',(-0.93619494143326,4.82902765031254,11.6011399787944));
#24440=CARTESIAN_POINT('Ctrl Pts',(-0.855183149266913,4.84403040958246,
11.5965087092486));
#24441=CARTESIAN_POINT('Ctrl Pts',(-0.716853764278619,4.86606954711842,
11.5886111462403));
#24442=CARTESIAN_POINT('Ctrl Pts',(-0.659719143635766,4.87414430708519,
11.5853522521962));
#24443=CARTESIAN_POINT('Ctrl Pts',(-0.533470063845456,4.88972640514343,
11.5781522650352));
#24444=CARTESIAN_POINT('Ctrl Pts',(-0.464311872666966,4.8967774060811,11.5742088613727));
#24445=CARTESIAN_POINT('Ctrl Pts',(-0.177320180609664,4.91990295387174,
11.5578353192441));
#24446=CARTESIAN_POINT('Ctrl Pts',(0.0413123148125404,4.92292376582453,
11.5453276418417));
#24447=CARTESIAN_POINT('Ctrl Pts',(0.324647561748035,4.90795823283804,11.529096159069));
#24448=CARTESIAN_POINT('Ctrl Pts',(0.38980410966039,4.90321352849762,11.5253630825652));
#24449=CARTESIAN_POINT('Ctrl Pts',(0.493199458271979,4.89361021623511,11.5194435126087));
#24450=CARTESIAN_POINT('Ctrl Pts',(0.531508874276635,4.88959763234913,11.5172512075485));
#24451=CARTESIAN_POINT('Ctrl Pts',(0.590002087466434,4.88277540042378,11.5139066451562));
#24452=CARTESIAN_POINT('Ctrl Pts',(0.610221985699057,4.88028966447644,11.5127510116306));
#24453=CARTESIAN_POINT('Ctrl Pts',(0.63597067456829,4.87696172030142,11.5112802220076));
#24454=CARTESIAN_POINT('Ctrl Pts',(0.641514193277487,4.87623562393877,11.5109636201346));
#24455=CARTESIAN_POINT('Ctrl Pts',(0.652094264631559,4.87483148005618,11.5103594520851));
#24456=CARTESIAN_POINT('Ctrl Pts',(0.657131026752012,4.87415507577591,11.5100718664993));
#24457=CARTESIAN_POINT('Ctrl Pts',(0.668800865182612,4.8725694750713,11.5094056211974));
#24458=CARTESIAN_POINT('Ctrl Pts',(0.675433154306773,4.8716545383418,11.5090270289994));
#24459=CARTESIAN_POINT('Ctrl Pts',(0.740437120809957,4.86255182215224,11.5053168125755));
#24460=CARTESIAN_POINT('Ctrl Pts',(0.798659547235146,4.85332879616948,11.5019969126584));
#24461=CARTESIAN_POINT('Ctrl Pts',(1.031819681583,4.8120844523055,11.4886868846752));
#24462=CARTESIAN_POINT('Ctrl Pts',(1.20512849217673,4.77163227574737,11.4787548336228));
#24463=CARTESIAN_POINT('Ctrl Pts',(1.45202900179808,4.69969022421419,11.4643264813003));
#24464=CARTESIAN_POINT('Ctrl Pts',(1.52764374349726,4.67565833467376,11.4598695648807));
#24465=CARTESIAN_POINT('Ctrl Pts',(1.67144881163996,4.62609322113823,11.4513014330926));
#24466=CARTESIAN_POINT('Ctrl Pts',(1.73971860354431,4.60085412063183,11.4471931620788));
#24467=CARTESIAN_POINT('Ctrl Pts',(1.86566830250704,4.551086660596,11.4395277860474));
#24468=CARTESIAN_POINT('Ctrl Pts',(1.92348832946062,4.52695267769817,11.4359742686168));
#24469=CARTESIAN_POINT('Ctrl Pts',(2.09235392855577,4.45264904144882,11.4254870840906));
#24470=CARTESIAN_POINT('Ctrl Pts',(2.20201350561321,4.39945046082844,11.4185346720033));
#24471=CARTESIAN_POINT('Ctrl Pts',(2.44785964546724,4.26868783988599,11.4026082874923));
#24472=CARTESIAN_POINT('Ctrl Pts',(2.58254435506734,4.18857703776568,11.3936314581767));
#24473=CARTESIAN_POINT('Ctrl Pts',(2.73554869453851,4.08738007028649,11.3831648563363));
#24474=CARTESIAN_POINT('Ctrl Pts',(2.75779911215781,4.0724005901083,11.3816359254806));
#24475=CARTESIAN_POINT('Ctrl Pts',(2.81507242078053,4.03315825661325,11.3776832830877));
#24476=CARTESIAN_POINT('Ctrl Pts',(2.84990476634391,4.008620852083,11.3752625796703));
#24477=CARTESIAN_POINT('Ctrl Pts',(2.91778310031388,3.95947245216452,11.3705143891019));
#24478=CARTESIAN_POINT('Ctrl Pts',(2.95084739502148,3.93489263105812,11.3681867522965));
#24479=CARTESIAN_POINT('Ctrl Pts',(3.09876989239596,3.82201469904843,11.3576950358432));
#24480=CARTESIAN_POINT('Ctrl Pts',(3.21000253829246,3.7290824419785,11.349587046979));
#24481=CARTESIAN_POINT('Ctrl Pts',(3.43000513533123,3.52812761538154,11.3328943125461));
#24482=CARTESIAN_POINT('Ctrl Pts',(3.53815548318082,3.41966002863199,11.3243172389735));
#24483=CARTESIAN_POINT('Ctrl Pts',(3.68926887629328,3.25324741581559,11.3116516610141));
#24484=CARTESIAN_POINT('Ctrl Pts',(3.73630116590786,3.19912129059041,11.3076032248845));
#24485=CARTESIAN_POINT('Ctrl Pts',(3.82261214581019,3.09529146283879,11.2999590334696));
#24486=CARTESIAN_POINT('Ctrl Pts',(3.86214677326821,3.04581927373262,11.2963663719308));
#24487=CARTESIAN_POINT('Ctrl Pts',(3.99611483504287,2.87137289363798,11.2838600351471));
#24488=CARTESIAN_POINT('Ctrl Pts',(4.08552499571757,2.74266301803783,11.2749105775543));
#24489=CARTESIAN_POINT('Ctrl Pts',(4.22321707792243,2.52273625988765,11.260058370783));
#24490=CARTESIAN_POINT('Ctrl Pts',(4.27504645325742,2.43387318521027,11.2541690979252));
#24491=CARTESIAN_POINT('Ctrl Pts',(4.35477380844231,2.28676309161599,11.2446129607616));
#24492=CARTESIAN_POINT('Ctrl Pts',(4.38437846665882,2.22947661269929,11.2409377476548));
#24493=CARTESIAN_POINT('Ctrl Pts',(4.42910704578718,2.1385859134006,11.2351841247694));
#24494=CARTESIAN_POINT('Ctrl Pts',(4.44499415426079,2.10536598870881,11.2330974433948));
#24495=CARTESIAN_POINT('Ctrl Pts',(4.48387562960427,2.02166252704719,11.2278795893127));
#24496=CARTESIAN_POINT('Ctrl Pts',(4.50639177829064,1.97096252655223,11.2247541579613));
#24497=CARTESIAN_POINT('Ctrl Pts',(4.59889822442862,1.7527870313095,11.211428263852));
#24498=CARTESIAN_POINT('Ctrl Pts',(4.66044645631806,1.5818871130622,11.20129258381));
#24499=CARTESIAN_POINT('Ctrl Pts',(4.74342535230206,1.30416198834911,11.1850310731285));
#24500=CARTESIAN_POINT('Ctrl Pts',(4.7710037379179,1.19935210770026,11.1789413851554));
#24501=CARTESIAN_POINT('Ctrl Pts',(4.8102037499395,1.02749072581088,11.1689943713321));
#24502=CARTESIAN_POINT('Ctrl Pts',(4.82393581494914,0.960958076300132,11.1651530049468));
#24503=CARTESIAN_POINT('Ctrl Pts',(4.8509747700032,0.814711677053215,11.1567215550321));
#24504=CARTESIAN_POINT('Ctrl Pts',(4.86370399427486,0.734911267762847,11.1521287224107));
#24505=CARTESIAN_POINT('Ctrl Pts',(4.89263884105355,0.519525776076575,11.1397440487492));
#24506=CARTESIAN_POINT('Ctrl Pts',(4.90517415958433,0.383520178632083,11.1319346787192));
#24507=CARTESIAN_POINT('Ctrl Pts',(4.91841971519391,0.120290824076351,11.1168470553203));
#24508=CARTESIAN_POINT('Ctrl Pts',(4.91988585020692,-0.00678998865839053,
11.1095754556349));
#24509=CARTESIAN_POINT('Ctrl Pts',(4.91526297003377,-0.176674280481472,
11.0998993840201));
#24510=CARTESIAN_POINT('Ctrl Pts',(4.91353471336303,-0.219546221357184,
11.0974614982575));
#24511=CARTESIAN_POINT('Ctrl Pts',(4.90935805768069,-0.297722042531042,
11.0930255902301));
#24512=CARTESIAN_POINT('Ctrl Pts',(4.90708919011208,-0.333032523742834,
11.0910256249111));
#24513=CARTESIAN_POINT('Ctrl Pts',(4.89850406295982,-0.44735087531657,11.084557444096));
#24514=CARTESIAN_POINT('Ctrl Pts',(4.89065896730684,-0.526231849482437,
11.0801046133913));
#24515=CARTESIAN_POINT('Ctrl Pts',(4.86220525429989,-0.755827612450618,
11.067126451132));
#24516=CARTESIAN_POINT('Ctrl Pts',(4.83650816569251,-0.905816814448504,
11.0586239157759));
#24517=CARTESIAN_POINT('Ctrl Pts',(4.78224613211133,-1.15304369469664,11.0444170325476));
#24518=CARTESIAN_POINT('Ctrl Pts',(4.75755516543369,-1.25102211025607,11.038735926388));
#24519=CARTESIAN_POINT('Ctrl Pts',(4.71135253285143,-1.41311758381988,11.0292216053931));
#24520=CARTESIAN_POINT('Ctrl Pts',(4.69150458321728,-1.47767675950514,11.0254011956502));
#24521=CARTESIAN_POINT('Ctrl Pts',(4.64406846125941,-1.6213670055684,11.0168200298761));
#24522=CARTESIAN_POINT('Ctrl Pts',(4.61577476468717,-1.70024289988798,11.0120555059813));
#24523=CARTESIAN_POINT('Ctrl Pts',(4.52026759711774,-1.94650745030007,10.9969964375777));
#24524=CARTESIAN_POINT('Ctrl Pts',(4.44585535547024,-2.1109428269787,10.9866641765529));
#24525=CARTESIAN_POINT('Ctrl Pts',(4.34205925707084,-2.31034195054938,10.9738057362076));
#24526=CARTESIAN_POINT('Ctrl Pts',(4.32100347477446,-2.34948665008068,10.9712653168886));
#24527=CARTESIAN_POINT('Ctrl Pts',(4.27100898910727,-2.43948523756618,10.9653891660272));
#24528=CARTESIAN_POINT('Ctrl Pts',(4.24168745156505,-2.49011921183023,10.9620564843368));
#24529=CARTESIAN_POINT('Ctrl Pts',(4.19247985484302,-2.57170128544579,10.9566475643527));
#24530=CARTESIAN_POINT('Ctrl Pts',(4.17313798447193,-2.60297027159792,10.9545651666386));
#24531=CARTESIAN_POINT('Ctrl Pts',(4.12006834574893,-2.68665298707303,10.9489654428427));
#24532=CARTESIAN_POINT('Ctrl Pts',(4.08569187845162,-2.73864737811433,10.9454565087779));
#24533=CARTESIAN_POINT('Ctrl Pts',(3.95289981190829,-2.93142780059339,10.9323027001105));
#24534=CARTESIAN_POINT('Ctrl Pts',(3.8481198567885,-3.06767989436164,10.9227077378722));
#24535=CARTESIAN_POINT('Ctrl Pts',(3.68473539528482,-3.25856213738321,10.9086112330787));
#24536=CARTESIAN_POINT('Ctrl Pts',(3.63158786517697,-3.31769069646575,10.9041453211765));
#24537=CARTESIAN_POINT('Ctrl Pts',(3.52702876075377,-3.42849224601403,10.8955638468174));
#24538=CARTESIAN_POINT('Ctrl Pts',(3.4758557319513,-3.48036172382289,10.8914512583837));
#24539=CARTESIAN_POINT('Ctrl Pts',(3.37860040705878,-3.5746555178347,10.88378395934));
#24540=CARTESIAN_POINT('Ctrl Pts',(3.33282328770755,-3.61737357862419,10.8802328704035));
#24541=CARTESIAN_POINT('Ctrl Pts',(3.19601789929503,-3.74023516176712,10.869780737857));
#24542=CARTESIAN_POINT('Ctrl Pts',(3.10282724385609,-3.81789889429667,10.8628611758776));
#24543=CARTESIAN_POINT('Ctrl Pts',(2.85784266244473,-4.00716605671408,10.8451552767022));
#24544=CARTESIAN_POINT('Ctrl Pts',(2.70233291258256,-4.113640972227,10.8343565145569));
#24545=CARTESIAN_POINT('Ctrl Pts',(2.50595032105009,-4.23214857629367,10.8213030755625));
#24546=CARTESIAN_POINT('Ctrl Pts',(2.47053499452362,-4.25291964211589,10.8189713262023));
#24547=CARTESIAN_POINT('Ctrl Pts',(2.39770089289377,-4.29441997553446,10.8142233269937));
#24548=CARTESIAN_POINT('Ctrl Pts',(2.36026338174731,-4.31510942202753,10.8118077012397));
#24549=CARTESIAN_POINT('Ctrl Pts',(2.2149870038767,-4.39293853385853,10.8025184267318));
#24550=CARTESIAN_POINT('Ctrl Pts',(2.10530466229432,-4.44654576889522,10.7956816005542));
#24551=CARTESIAN_POINT('Ctrl Pts',(1.83672874274556,-4.56564467935578,10.7792217846967));
#24552=CARTESIAN_POINT('Ctrl Pts',(1.67617834340497,-4.62699784631384,10.7696072668492));
#24553=CARTESIAN_POINT('Ctrl Pts',(1.44449707614652,-4.70188859843657,10.7558881807876));
#24554=CARTESIAN_POINT('Ctrl Pts',(1.3757708247917,-4.72245515349356,10.7518379672928));
#24555=CARTESIAN_POINT('Ctrl Pts',(1.24559462598124,-4.75832785546681,10.7441933146452));
#24556=CARTESIAN_POINT('Ctrl Pts',(1.18425080404157,-4.77396479615308,10.7406019845797));
#24557=CARTESIAN_POINT('Ctrl Pts',(0.969320674726666,-4.82435423259623,
10.728049944093));
#24558=CARTESIAN_POINT('Ctrl Pts',(0.814382911509027,-4.85291207845091,
10.7190529601176));
#24559=CARTESIAN_POINT('Ctrl Pts',(0.556874565091969,-4.88769453288823,
10.7041793239958));
#24560=CARTESIAN_POINT('Ctrl Pts',(0.455000721114591,-4.8982284151843,10.6983162460567));
#24561=CARTESIAN_POINT('Ctrl Pts',(0.288713442575388,-4.91018994115737,
10.688794999373));
#24562=CARTESIAN_POINT('Ctrl Pts',(0.224469721518231,-4.91354599033202,
10.6851285386314));
#24563=CARTESIAN_POINT('Ctrl Pts',(0.12338053489275,-4.91684002280076,10.6793839206464));
#24564=CARTESIAN_POINT('Ctrl Pts',(0.0865704821135372,-4.91762586655673,
10.6772975462724));
#24565=CARTESIAN_POINT('Ctrl Pts',(-0.00581759150620979,-4.9185605415174,
10.6720741144194));
#24566=CARTESIAN_POINT('Ctrl Pts',(-0.06139579123391,-4.91818079250148,
10.6689428374763));
#24567=CARTESIAN_POINT('Ctrl Pts',(-0.298272090618897,-4.91254627786168,
10.6556190098578));
#24568=CARTESIAN_POINT('Ctrl Pts',(-0.479211637011975,-4.89820723622012,
10.6454909880087));
#24569=CARTESIAN_POINT('Ctrl Pts',(-0.738001355605268,-4.86321920916054,
10.6308402635684));
#24570=CARTESIAN_POINT('Ctrl Pts',(-0.816784611373685,-4.85060922136111,
10.6263586715613));
#24571=CARTESIAN_POINT('Ctrl Pts',(-0.966997531568134,-4.82280276826103,
10.617753933895));
#24572=CARTESIAN_POINT('Ctrl Pts',(-1.03846407717233,-4.80792085678421,
10.6136338140703));
#24573=CARTESIAN_POINT('Ctrl Pts',(-1.17873252734246,-4.7754384428343,10.605484583352));
#24574=CARTESIAN_POINT('Ctrl Pts',(-1.2475372695405,-4.75792741617651,10.6014570378615));
#24575=CARTESIAN_POINT('Ctrl Pts',(-1.48337123395864,-4.69243948446795,
10.5875370479908));
#24576=CARTESIAN_POINT('Ctrl Pts',(-1.64822055199276,-4.63710535859989,
10.5776008996415));
#24577=CARTESIAN_POINT('Ctrl Pts',(-1.92885623999235,-4.5260460572966,10.5603236948443));
#24578=CARTESIAN_POINT('Ctrl Pts',(-2.04603519113683,-4.47429546022447,
10.5529955488369));
#24579=CARTESIAN_POINT('Ctrl Pts',(-2.19786767535073,-4.40002722195041,
10.5433766098407));
#24580=CARTESIAN_POINT('Ctrl Pts',(-2.23444760751868,-4.38156431197187,
10.541049558764));
#24581=CARTESIAN_POINT('Ctrl Pts',(-2.30881995330094,-4.34285290155752,
10.5363007261591));
#24582=CARTESIAN_POINT('Ctrl Pts',(-2.34658692964247,-4.32256298282666,
10.5338796145433));
#24583=CARTESIAN_POINT('Ctrl Pts',(-2.56752679638586,-4.20011622683668,
10.5196424860244));
#24584=CARTESIAN_POINT('Ctrl Pts',(-2.74428038348977,-4.08681993558374,
10.5079431263938));
#24585=CARTESIAN_POINT('Ctrl Pts',(-2.97721662631528,-3.91556703001333,
10.4917225570818));
#24586=CARTESIAN_POINT('Ctrl Pts',(-3.04002299989872,-3.86700711280358,
10.4872629864342));
#24587=CARTESIAN_POINT('Ctrl Pts',(-3.15812504082092,-3.77103821131222,
10.4786909180222));
#24588=CARTESIAN_POINT('Ctrl Pts',(-3.2135971153543,-3.72387921164953,10.4745813733624));
#24589=CARTESIAN_POINT('Ctrl Pts',(-3.32116695431864,-3.62823569170451,
10.4664340651944));
#24590=CARTESIAN_POINT('Ctrl Pts',(-3.373300068129,-3.579817127543,10.4623977669007));
#24591=CARTESIAN_POINT('Ctrl Pts',(-3.56085064125861,-3.39789373459276,
10.447536985881));
#24592=CARTESIAN_POINT('Ctrl Pts',(-3.68954307446087,-3.25769999598795,
10.4366578778787));
#24593=CARTESIAN_POINT('Ctrl Pts',(-3.86011207468373,-3.0487781751467,10.4212202614789));
#24594=CARTESIAN_POINT('Ctrl Pts',(-3.90892776621562,-2.98593325997835,
10.4166687028537));
#24595=CARTESIAN_POINT('Ctrl Pts',(-3.97218966995185,-2.90027875892196,
10.4105929666145));
#24596=CARTESIAN_POINT('Ctrl Pts',(-3.98800381045214,-2.87849496639993,
10.409058531442));
#24597=CARTESIAN_POINT('Ctrl Pts',(-4.02844140873953,-2.82181971638326,
10.4050947068313));
#24598=CARTESIAN_POINT('Ctrl Pts',(-4.05279083571904,-2.78673522127334,
10.4026683283143));
#24599=CARTESIAN_POINT('Ctrl Pts',(-4.09967943092282,-2.71725999456605,
10.3979192632281));
#24600=CARTESIAN_POINT('Ctrl Pts',(-4.12225039424235,-2.68289490055045,
10.3955963812893));
#24601=CARTESIAN_POINT('Ctrl Pts',(-4.22313405006362,-2.52501671304363,
10.3850318629094));
#24602=CARTESIAN_POINT('Ctrl Pts',(-4.2963452864242,-2.39833041056331,10.3768475983938));
#24603=CARTESIAN_POINT('Ctrl Pts',(-4.43230731972234,-2.13679484452241,
10.3603341294461));
#24604=CARTESIAN_POINT('Ctrl Pts',(-4.49480701624097,-2.00198640737134,
10.3520128972845));
#24605=CARTESIAN_POINT('Ctrl Pts',(-4.57859906874176,-1.79746240085071,
10.3395619395194));
#24606=CARTESIAN_POINT('Ctrl Pts',(-4.60460035147513,-1.72976760222191,
10.3354685899248));
#24607=CARTESIAN_POINT('Ctrl Pts',(-4.65031093746895,-1.60241539284799,
10.3278094892047));
#24608=CARTESIAN_POINT('Ctrl Pts',(-4.67039235411379,-1.54290701494473,
10.3242472064281));
#24609=CARTESIAN_POINT('Ctrl Pts',(-4.72696197406515,-1.36403444774561,
10.3135823071809));
#24610=CARTESIAN_POINT('Ctrl Pts',(-4.7600518413802,-1.24364998951344,10.3064597189482));
#24611=CARTESIAN_POINT('Ctrl Pts',(-4.82352072643319,-0.972807890322336,
10.2905475216113));
#24612=CARTESIAN_POINT('Ctrl Pts',(-4.85151036882933,-0.821921397181798,
10.2817571973669));
#24613=CARTESIAN_POINT('Ctrl Pts',(-4.87603128716218,-0.643592335528763,
10.2714871104685));
#24614=CARTESIAN_POINT('Ctrl Pts',(-4.87944453888547,-0.617181666680833,
10.2699692291038));
#24615=CARTESIAN_POINT('Ctrl Pts',(-4.88773665754798,-0.548645342023595,
10.266039056218));
#24616=CARTESIAN_POINT('Ctrl Pts',(-4.89228552337227,-0.506481744906349,
10.2636297671248));
#24617=CARTESIAN_POINT('Ctrl Pts',(-4.8996543684323,-0.428767407664563,
10.2592070075046));
#24618=CARTESIAN_POINT('Ctrl Pts',(-4.90263407618996,-0.393234747177966,
10.2571917698034));
#24619=CARTESIAN_POINT('Ctrl Pts',(-4.91134152187288,-0.273818284863138,
10.2504369324928));
#24620=CARTESIAN_POINT('Ctrl Pts',(-4.91530472988333,-0.189820123855565,
10.245714926708));
#24621=CARTESIAN_POINT('Ctrl Pts',(-4.91786999539248,-0.0705540499605967,
10.2390244879591));
#24622=CARTESIAN_POINT('Ctrl Pts',(-4.91824910538206,-0.0353399245040969,
10.2370508736839));
#24623=CARTESIAN_POINT('Ctrl Pts',(-4.91825477204957,0.188114146117957,
10.2245303756001));
#24624=CARTESIAN_POINT('Ctrl Pts',(-4.90745272922607,0.376196211149348,
10.2139997504658));
#24625=CARTESIAN_POINT('Ctrl Pts',(-4.87779411797335,0.633494626895945,
10.1994022806027));
#24626=CARTESIAN_POINT('Ctrl Pts',(-4.86817435285551,0.703611554061901,
10.1954053538392));
#24627=CARTESIAN_POINT('Ctrl Pts',(-4.84551871392882,0.845874047925768,
10.1872476796469));
#24628=CARTESIAN_POINT('Ctrl Pts',(-4.83237603175276,0.917984874495307,
10.1830871854366));
#24629=CARTESIAN_POINT('Ctrl Pts',(-4.80164031852491,1.06758784650079,10.1743958106042));
#24630=CARTESIAN_POINT('Ctrl Pts',(-4.7837709210378,1.14500179752884,10.1698643878674));
#24631=CARTESIAN_POINT('Ctrl Pts',(-4.76403458704821,1.22194824600244,10.1653249229632));
#24632=CARTESIAN_POINT('',(-4.91847990603042,0.000102917318248914,9.88985943599074));
#24633=CARTESIAN_POINT('Ctrl Pts',(-4.76374494423105,1.22187361077196,9.81992259791717));
#24634=CARTESIAN_POINT('Ctrl Pts',(-4.83780683195621,0.933967707338634,
9.83675495907435));
#24635=CARTESIAN_POINT('Ctrl Pts',(-4.90451732111342,0.526079169820603,
9.86006723843221));
#24636=CARTESIAN_POINT('Ctrl Pts',(-4.91858617934998,0.114510461609331,
9.88337951779007));
#24637=CARTESIAN_POINT('Ctrl Pts',(-4.91847990603042,0.000102917318248914,
9.88985943599074));
#24638=CARTESIAN_POINT('Ctrl Pts',(-4.91824999876294,0.000110310282362309,
9.88999175175149));
#24639=CARTESIAN_POINT('Ctrl Pts',(-4.91825453779905,-0.202265332865951,
9.90134365005785));
#24640=CARTESIAN_POINT('Ctrl Pts',(-4.90576812281614,-0.404447615577542,
9.91264566029797));
#24641=CARTESIAN_POINT('Ctrl Pts',(-4.87289744207536,-0.669508609740337,
9.92767551990786));
#24642=CARTESIAN_POINT('Ctrl Pts',(-4.86366606934858,-0.733569026504508,
9.93132374267188));
#24643=CARTESIAN_POINT('Ctrl Pts',(-4.84285675483651,-0.860215179119433,
9.9385757723957));
#24644=CARTESIAN_POINT('Ctrl Pts',(-4.8313227855427,-0.92279560612633,9.94217860732116));
#24645=CARTESIAN_POINT('Ctrl Pts',(-4.79975029445116,-1.07722585063687,
9.95112425534546));
#24646=CARTESIAN_POINT('Ctrl Pts',(-4.77828661142264,-1.16875795308923,
9.95647522580859));
#24647=CARTESIAN_POINT('Ctrl Pts',(-4.69310277752286,-1.49026986293166,
9.97545931182569));
#24648=CARTESIAN_POINT('Ctrl Pts',(-4.61528813011351,-1.71616818121476,
9.98915931489593));
#24649=CARTESIAN_POINT('Ctrl Pts',(-4.5054544861416,-1.97273965245129,10.0050442085078));
#24650=CARTESIAN_POINT('Ctrl Pts',(-4.48906419700856,-2.00975733533123,
10.0073437676501));
#24651=CARTESIAN_POINT('Ctrl Pts',(-4.45467149444764,-2.08491322213457,
10.0120261686412));
#24652=CARTESIAN_POINT('Ctrl Pts',(-4.43663178725853,-2.12303078303241,
10.0144082690615));
#24653=CARTESIAN_POINT('Ctrl Pts',(-4.36071909717125,-2.27823847923328,
10.0241486493368));
#24654=CARTESIAN_POINT('Ctrl Pts',(-4.29868279070856,-2.39323392314751,
10.0314630305708));
#24655=CARTESIAN_POINT('Ctrl Pts',(-4.17292731400944,-2.60564207440643,
10.045291497569));
#24656=CARTESIAN_POINT('Ctrl Pts',(-4.11018565601439,-2.70352855235342,
10.0518004780026));
#24657=CARTESIAN_POINT('Ctrl Pts',(-3.99377011426145,-2.8717214089548,10.0632938232787));
#24658=CARTESIAN_POINT('Ctrl Pts',(-3.9415580828843,-2.94297522860048,10.0682666269201));
#24659=CARTESIAN_POINT('Ctrl Pts',(-3.88111108590409,-3.02097121720359,
10.0738406735553));
#24660=CARTESIAN_POINT('Ctrl Pts',(-3.87474005314753,-3.02913847097678,
10.0744259906496));
#24661=CARTESIAN_POINT('Ctrl Pts',(-3.8636049146689,-3.04332039020862,10.0754452394634));
#24662=CARTESIAN_POINT('Ctrl Pts',(-3.85885244369161,-3.04934415108085,
10.0758790756252));
#24663=CARTESIAN_POINT('Ctrl Pts',(-3.84398846546855,-3.0680938596647,10.0772323079428));
#24664=CARTESIAN_POINT('Ctrl Pts',(-3.83382797033259,-3.08078080141492,
10.078152097182));
#24665=CARTESIAN_POINT('Ctrl Pts',(-3.80124348828779,-3.12105670885988,
10.0810854215126));
#24666=CARTESIAN_POINT('Ctrl Pts',(-3.77858323860506,-3.14845290996315,
10.0831008577279));
#24667=CARTESIAN_POINT('Ctrl Pts',(-3.70427897573426,-3.23632893135392,
10.0896327616442));
#24668=CARTESIAN_POINT('Ctrl Pts',(-3.65146495520528,-3.29580205117316,
10.0941584660166));
#24669=CARTESIAN_POINT('Ctrl Pts',(-3.47466138870684,-3.48542925322802,
10.1089468804662));
#24670=CARTESIAN_POINT('Ctrl Pts',(-3.34497641622151,-3.61007213664745,
10.1192465150454));
#24671=CARTESIAN_POINT('Ctrl Pts',(-3.16356840353964,-3.76624138507315,
10.1329349241729));
#24672=CARTESIAN_POINT('Ctrl Pts',(-3.11767055738278,-3.80432248800459,
10.1363410267463));
#24673=CARTESIAN_POINT('Ctrl Pts',(-3.03500724895677,-3.87040673228028,
10.1423710496987));
#24674=CARTESIAN_POINT('Ctrl Pts',(-2.99851821360445,-3.89874413937888,
10.1449979812391));
#24675=CARTESIAN_POINT('Ctrl Pts',(-2.93061991554279,-3.9499568561393,10.1498199417267));
#24676=CARTESIAN_POINT('Ctrl Pts',(-2.89932872405437,-3.97298190691566,
10.1520166365853));
#24677=CARTESIAN_POINT('Ctrl Pts',(-2.80524481460706,-4.04050830936632,
10.1585516564845));
#24678=CARTESIAN_POINT('Ctrl Pts',(-2.74167669366778,-4.08390927848074,
10.1628763192199));
#24679=CARTESIAN_POINT('Ctrl Pts',(-2.54722356455809,-4.21008442479594,
10.1758816517908));
#24680=CARTESIAN_POINT('Ctrl Pts',(-2.41342358950316,-4.28818672538865,
10.1845367222657));
#24681=CARTESIAN_POINT('Ctrl Pts',(-2.20837238548503,-4.39523862388356,
10.197519351947));
#24682=CARTESIAN_POINT('Ctrl Pts',(-2.1397662946987,-4.42904405154125,10.201817743285));
#24683=CARTESIAN_POINT('Ctrl Pts',(-2.00970074295045,-4.48940574839535,
10.2098982595506));
#24684=CARTESIAN_POINT('Ctrl Pts',(-1.94843297421072,-4.51633367543774,
10.2136769085086));
#24685=CARTESIAN_POINT('Ctrl Pts',(-1.83631583245147,-4.56290435431281,
10.2205491921026));
#24686=CARTESIAN_POINT('Ctrl Pts',(-1.78565280542158,-4.58296803071386,
10.223639198762));
#24687=CARTESIAN_POINT('Ctrl Pts',(-1.62300713282659,-4.64427283973423,
10.2335150634465));
#24688=CARTESIAN_POINT('Ctrl Pts',(-1.50985359894462,-4.68228190871158,
10.2403208171079));
#24689=CARTESIAN_POINT('Ctrl Pts',(-1.2640779129937,-4.75500308051646,10.2549761087533));
#24690=CARTESIAN_POINT('Ctrl Pts',(-1.13115839664881,-4.788363804184,10.2628252112486));
#24691=CARTESIAN_POINT('Ctrl Pts',(-0.944139328405097,-4.82707988484651,
10.27374100434));
#24692=CARTESIAN_POINT('Ctrl Pts',(-0.891081463195211,-4.83715548450801,
10.276823444333));
#24693=CARTESIAN_POINT('Ctrl Pts',(-0.833708393484895,-4.84707449891059,
10.2801389545071));
#24694=CARTESIAN_POINT('Ctrl Pts',(-0.829547700261919,-4.84778830977509,
10.2803792953215));
#24695=CARTESIAN_POINT('Ctrl Pts',(-0.821788863246662,-4.84910913898542,
10.2808272932941));
#24696=CARTESIAN_POINT('Ctrl Pts',(-0.818190953500681,-4.84971751148334,
10.2810349624566));
#24697=CARTESIAN_POINT('Ctrl Pts',(-0.811411481920297,-4.85085609691034,
10.2814261260442));
#24698=CARTESIAN_POINT('Ctrl Pts',(-0.808230069436244,-4.85138718520848,
10.2816096284923));
#24699=CARTESIAN_POINT('Ctrl Pts',(-0.769567965604294,-4.85780214789214,
10.2838389129152));
#24700=CARTESIAN_POINT('Ctrl Pts',(-0.734024013661139,-4.86329984154134,
10.2858809559073));
#24701=CARTESIAN_POINT('Ctrl Pts',(-0.655752472887715,-4.87452869285757,
10.2903597697187));
#24702=CARTESIAN_POINT('Ctrl Pts',(-0.613003267108175,-4.88008896808139,
10.2927943215402));
#24703=CARTESIAN_POINT('Ctrl Pts',(-0.449352733539945,-4.89919022053326,
10.3020806558717));
#24704=CARTESIAN_POINT('Ctrl Pts',(-0.328036348878668,-4.90880590896388,
10.3088959458809));
#24705=CARTESIAN_POINT('Ctrl Pts',(-0.0867202898605512,-4.91894624303943,
10.3224272000269));
#24706=CARTESIAN_POINT('Ctrl Pts',(0.0331902186420285,-4.91959863579707,
10.3291386278264));
#24707=CARTESIAN_POINT('Ctrl Pts',(0.223430798605837,-4.91367748938978,
10.3398314847085));
#24708=CARTESIAN_POINT('Ctrl Pts',(0.29380181124556,-4.90997231768317,10.343796389656));
#24709=CARTESIAN_POINT('Ctrl Pts',(0.413754207979656,-4.90106853611265,
10.3505814568448));
#24710=CARTESIAN_POINT('Ctrl Pts',(0.46338079400134,-4.89662572868215,10.3533963369673));
#24711=CARTESIAN_POINT('Ctrl Pts',(0.575773910052433,-4.88483982553145,
10.3597926947478));
#24712=CARTESIAN_POINT('Ctrl Pts',(0.638483498859213,-4.87703951468597,
10.363376687218));
#24713=CARTESIAN_POINT('Ctrl Pts',(0.822879047335149,-4.85048548965462,
10.3739667208791));
#24714=CARTESIAN_POINT('Ctrl Pts',(0.944030009033002,-4.82836888850827,
10.3809919480464));
#24715=CARTESIAN_POINT('Ctrl Pts',(1.21197480950682,-4.76898347484425,10.3966897109753));
#24716=CARTESIAN_POINT('Ctrl Pts',(1.35813765337885,-4.72943428217761,10.4053632815479));
#24717=CARTESIAN_POINT('Ctrl Pts',(1.55766824051209,-4.665430379579,10.4173226980138));
#24718=CARTESIAN_POINT('Ctrl Pts',(1.61277289979163,-4.64666920102113,10.4206380535241));
#24719=CARTESIAN_POINT('Ctrl Pts',(1.70250237364478,-4.61433099151768,10.4260525627033));
#24720=CARTESIAN_POINT('Ctrl Pts',(1.73732873664354,-4.60133173431402,10.428157679161));
#24721=CARTESIAN_POINT('Ctrl Pts',(1.8324179779233,-4.56460530719894,10.4339173634115));
#24722=CARTESIAN_POINT('Ctrl Pts',(1.89236490333903,-4.54008066931748,10.4375626405245));
#24723=CARTESIAN_POINT('Ctrl Pts',(2.10478604920366,-4.44823950749769,10.4505636540001));
#24724=CARTESIAN_POINT('Ctrl Pts',(2.25430134203274,-4.37436680089563,10.4598749871749));
#24725=CARTESIAN_POINT('Ctrl Pts',(2.47002588358666,-4.25377855135578,10.4737394150351));
#24726=CARTESIAN_POINT('Ctrl Pts',(2.53929903148868,-4.21279243460511,10.4782603026381));
#24727=CARTESIAN_POINT('Ctrl Pts',(2.66995074349636,-4.13109731453634,10.4869395049358));
#24728=CARTESIAN_POINT('Ctrl Pts',(2.73148206263846,-4.09067324154082,10.4910947228509));
#24729=CARTESIAN_POINT('Ctrl Pts',(2.84412235436368,-4.01299727011866,10.4988391936614));
#24730=CARTESIAN_POINT('Ctrl Pts',(2.89546525157868,-3.97611115574936,10.5024247248457));
#24731=CARTESIAN_POINT('Ctrl Pts',(3.04502524018541,-3.86422985722543,10.5130421194359));
#24732=CARTESIAN_POINT('Ctrl Pts',(3.14114242521811,-3.78651221195174,10.5200933546459));
#24733=CARTESIAN_POINT('Ctrl Pts',(3.31919911108462,-3.63109087774792,10.5336121436552));
#24734=CARTESIAN_POINT('Ctrl Pts',(3.40159205396748,-3.55402239581124,10.5400728038296));
#24735=CARTESIAN_POINT('Ctrl Pts',(3.51051459684917,-3.44487810903477,10.5488907039106));
#24736=CARTESIAN_POINT('Ctrl Pts',(3.53939543843366,-3.41519807267941,10.5512569083409));
#24737=CARTESIAN_POINT('Ctrl Pts',(3.58657143394745,-3.36547536937454,10.555167859758));
#24738=CARTESIAN_POINT('Ctrl Pts',(3.60508166634326,-3.3456397448249,10.5567144196348));
#24739=CARTESIAN_POINT('Ctrl Pts',(3.65251935714299,-3.29395453875242,10.5607086133711));
#24740=CARTESIAN_POINT('Ctrl Pts',(3.68119487640266,-3.26187653002807,10.5631531902242));
#24741=CARTESIAN_POINT('Ctrl Pts',(3.73683420692254,-3.19796700492586,10.5679541535831));
#24742=CARTESIAN_POINT('Ctrl Pts',(3.76382129218169,-3.1661604798308,10.5703106636474));
#24743=CARTESIAN_POINT('Ctrl Pts',(3.87968173354682,-3.02603428565132,10.580562089299));
#24744=CARTESIAN_POINT('Ctrl Pts',(3.96430884837542,-2.91428723382091,10.5884051439988));
#24745=CARTESIAN_POINT('Ctrl Pts',(4.12900310119292,-2.67634044089566,10.6046165962002));
#24746=CARTESIAN_POINT('Ctrl Pts',(4.20832358431271,-2.54979934754399,10.6129778650592));
#24747=CARTESIAN_POINT('Ctrl Pts',(4.3183107628147,-2.35518411303656,10.6255671417043));
#24748=CARTESIAN_POINT('Ctrl Pts',(4.35338596557883,-2.28970096610409,10.6297591356357));
#24749=CARTESIAN_POINT('Ctrl Pts',(4.4191990525009,-2.15984880739337,10.6379978962051));
#24750=CARTESIAN_POINT('Ctrl Pts',(4.45004651880877,-2.09555552506387,10.6420427708163));
#24751=CARTESIAN_POINT('Ctrl Pts',(4.55754573015877,-1.85841498352604,10.65684946934));
#24752=CARTESIAN_POINT('Ctrl Pts',(4.62561103308836,-1.68185913012717,10.667665442533));
#24753=CARTESIAN_POINT('Ctrl Pts',(4.70825651854234,-1.42413495691479,10.6831578845587));
#24754=CARTESIAN_POINT('Ctrl Pts',(4.73123337113465,-1.34583458717698,10.6878257955512));
#24755=CARTESIAN_POINT('Ctrl Pts',(4.7593084965076,-1.24053055285824,10.6940446954036));
#24756=CARTESIAN_POINT('Ctrl Pts',(4.76614393052881,-1.2140038968994,10.6956063131025));
#24757=CARTESIAN_POINT('Ctrl Pts',(4.78320989659181,-1.14540843955969,10.6996310272541));
#24758=CARTESIAN_POINT('Ctrl Pts',(4.79310725979743,-1.10325892822445,10.7020910593208));
#24759=CARTESIAN_POINT('Ctrl Pts',(4.81139511192857,-1.02048063529088,10.7068944564715));
#24760=CARTESIAN_POINT('Ctrl Pts',(4.81983063366231,-0.979865480218618,
10.7092380709465));
#24761=CARTESIAN_POINT('Ctrl Pts',(4.85530129297295,-0.797526290371632,
10.7197120598799));
#24762=CARTESIAN_POINT('Ctrl Pts',(4.87660643751717,-0.654759059181606,
10.7277868246346));
#24763=CARTESIAN_POINT('Ctrl Pts',(4.90762437728455,-0.357987799616617,
10.7445028265277));
#24764=CARTESIAN_POINT('Ctrl Pts',(4.91643121418963,-0.204048114438797,
10.7531364784312));
#24765=CARTESIAN_POINT('Ctrl Pts',(4.91872977752001,0.0222614244504118,
10.7658886621944));
#24766=CARTESIAN_POINT('Ctrl Pts',(4.91787265926533,0.0944803843395491,
10.7699664682051));
#24767=CARTESIAN_POINT('Ctrl Pts',(4.91294825881184,0.239724842675599,10.7781946786687));
#24768=CARTESIAN_POINT('Ctrl Pts',(4.90884178898662,0.312731058954474,10.7823443341099));
#24769=CARTESIAN_POINT('Ctrl Pts',(4.89095861970288,0.540114485856213,10.795321887893));
#24770=CARTESIAN_POINT('Ctrl Pts',(4.87151250100734,0.693948696867291,10.8041810658028));
#24771=CARTESIAN_POINT('Ctrl Pts',(4.82807097118783,0.942549789180452,10.8186277644665));
#24772=CARTESIAN_POINT('Ctrl Pts',(4.80845895023498,1.03797498600089,10.8242040387665));
#24773=CARTESIAN_POINT('Ctrl Pts',(4.77157645023075,1.19380798303528,10.8333480793429));
#24774=CARTESIAN_POINT('Ctrl Pts',(4.75595943213808,1.25457934709739,10.8369235192983));
#24775=CARTESIAN_POINT('Ctrl Pts',(4.72925621012607,1.35081359723044,10.8425950121735));
#24776=CARTESIAN_POINT('Ctrl Pts',(4.71892367477497,1.38647793731166,10.8446986458065));
#24777=CARTESIAN_POINT('Ctrl Pts',(4.6908799310336,1.47932825172955,10.850181054024));
#24778=CARTESIAN_POINT('Ctrl Pts',(4.67252675702473,1.53631391227947,10.8535524730919));
#24779=CARTESIAN_POINT('Ctrl Pts',(4.595727323005,1.7606512537303,10.8668803902101));
#24780=CARTESIAN_POINT('Ctrl Pts',(4.52929271328128,1.92512612168283,10.8767800299091));
#24781=CARTESIAN_POINT('Ctrl Pts',(4.42037760088476,2.15772514150769,10.8911897421422));
#24782=CARTESIAN_POINT('Ctrl Pts',(4.38488688494591,2.22896450595652,10.89566067467));
#24783=CARTESIAN_POINT('Ctrl Pts',(4.31346974260532,2.36400459036397,10.9042659388265));
#24784=CARTESIAN_POINT('Ctrl Pts',(4.27781648405565,2.42792604654686,10.9083973407692));
#24785=CARTESIAN_POINT('Ctrl Pts',(4.20420579608915,2.55324162265044,10.9166242060046));
#24786=CARTESIAN_POINT('Ctrl Pts',(4.16629678512446,2.61464339716152,10.9207183542512));
#24787=CARTESIAN_POINT('Ctrl Pts',(4.0314524699551,2.82266962737561,10.9348200258843));
#24788=CARTESIAN_POINT('Ctrl Pts',(3.92801832070811,2.96491879635683,10.944871924919));
#24789=CARTESIAN_POINT('Ctrl Pts',(3.76228534837853,3.16890746826185,10.9599175803453));
#24790=CARTESIAN_POINT('Ctrl Pts',(3.7055909517281,3.23502108474885,10.9649008954576));
#24791=CARTESIAN_POINT('Ctrl Pts',(3.60764257044835,3.34328725541346,10.973234175767));
#24792=CARTESIAN_POINT('Ctrl Pts',(3.56733178262398,3.38626618270303,10.9765904807856));
#24793=CARTESIAN_POINT('Ctrl Pts',(3.50036134701894,3.45514595677104,10.9820445555773));
#24794=CARTESIAN_POINT('Ctrl Pts',(3.47416355286357,3.48148686456857,10.9841485424768));
#24795=CARTESIAN_POINT('Ctrl Pts',(3.40213225590443,3.5522888790613,10.9898558574977));
#24796=CARTESIAN_POINT('Ctrl Pts',(3.35572725656295,3.59615835251417,10.9934502588543));
#24797=CARTESIAN_POINT('Ctrl Pts',(3.18443279412108,3.75188986628587,11.0064569032389));
#24798=CARTESIAN_POINT('Ctrl Pts',(3.054699027469,3.85825142891675,11.0158231975103));
#24799=CARTESIAN_POINT('Ctrl Pts',(2.85489817870372,4.0056512170232,11.0297517671742));
#24800=CARTESIAN_POINT('Ctrl Pts',(2.78884201183321,4.05191872506418,11.0342814331302));
#24801=CARTESIAN_POINT('Ctrl Pts',(2.66030115574118,4.13731928837812,11.0429736360396));
#24802=CARTESIAN_POINT('Ctrl Pts',(2.5980154189877,4.17671268442128,11.0471330467238));
#24803=CARTESIAN_POINT('Ctrl Pts',(2.48073143703083,4.24725153423737,11.054879440332));
#24804=CARTESIAN_POINT('Ctrl Pts',(2.42597231029193,4.27876527716147,11.0584626682572));
#24805=CARTESIAN_POINT('Ctrl Pts',(2.26294008323037,4.36845393780467,11.0690399301249));
#24806=CARTESIAN_POINT('Ctrl Pts',(2.15307700464381,4.42363497717238,11.0760530643338));
#24807=CARTESIAN_POINT('Ctrl Pts',(1.90027975062149,4.53895724255116,11.0919458666604));
#24808=CARTESIAN_POINT('Ctrl Pts',(1.75633458444715,4.59657318369448,11.1008275454499));
#24809=CARTESIAN_POINT('Ctrl Pts',(1.5842273423605,4.65619431914305,11.1112206220899));
#24810=CARTESIAN_POINT('Ctrl Pts',(1.55847140683504,4.664878207896,11.112770032296));
#24811=CARTESIAN_POINT('Ctrl Pts',(1.49171422786373,4.68677151313694,11.1167700075476));
#24812=CARTESIAN_POINT('Ctrl Pts',(1.45060882249536,4.69965665296393,11.1192175141761));
#24813=CARTESIAN_POINT('Ctrl Pts',(1.36942029670281,4.72393979450627,11.1240188883864));
#24814=CARTESIAN_POINT('Ctrl Pts',(1.32935103975748,4.73537168474138,11.1263729035258));
#24815=CARTESIAN_POINT('Ctrl Pts',(1.1531158100579,4.78323895126235,11.1366694928455));
#24816=CARTESIAN_POINT('Ctrl Pts',(1.01556359198251,4.81432055593229,11.1445594611984));
#24817=CARTESIAN_POINT('Ctrl Pts',(0.722232394343318,4.86746954773252,11.1612596406445));
#24818=CARTESIAN_POINT('Ctrl Pts',(0.566346945827341,4.88805991800792,11.1700626349582));
#24819=CARTESIAN_POINT('Ctrl Pts',(0.337829955120684,4.90716434514307,11.1829836385668));
#24820=CARTESIAN_POINT('Ctrl Pts',(0.265791838299751,4.91159297257837,11.1870586830919));
#24821=CARTESIAN_POINT('Ctrl Pts',(0.120570360926469,4.91731630109065,11.1952873492919));
#24822=CARTESIAN_POINT('Ctrl Pts',(0.0474031804538423,4.91856580576221,
11.1994402529787));
#24823=CARTESIAN_POINT('Ctrl Pts',(-0.179580576738728,4.91737674624483,
11.212355479898));
#24824=CARTESIAN_POINT('Ctrl Pts',(-0.333273012809801,4.90935549042928,
11.2211484141319));
#24825=CARTESIAN_POINT('Ctrl Pts',(-0.624127961619186,4.88045303890979,
11.2378801883569));
#24826=CARTESIAN_POINT('Ctrl Pts',(-0.761282733999841,4.86094710743022,
11.2458087761434));
#24827=CARTESIAN_POINT('Ctrl Pts',(-0.938972266765734,4.82797050046806,
11.2560962169342));
#24828=CARTESIAN_POINT('Ctrl Pts',(-0.980411596812561,4.81972626069503,
11.2584963228103));
#24829=CARTESIAN_POINT('Ctrl Pts',(-1.0632584020914,4.8021314197854,11.263294195181));
#24830=CARTESIAN_POINT('Ctrl Pts',(-1.10466139503448,4.79277663379129,11.2656917110484));
#24831=CARTESIAN_POINT('Ctrl Pts',(-1.26962935098017,4.75325173665569,11.2752543594274));
#24832=CARTESIAN_POINT('Ctrl Pts',(-1.39212547193389,4.71882910417538,11.2823784165381));
#24833=CARTESIAN_POINT('Ctrl Pts',(-1.66524233102293,4.63051849031779,11.2984589052828));
#24834=CARTESIAN_POINT('Ctrl Pts',(-1.81484510571672,4.57395562108618,11.3074081005433));
#24835=CARTESIAN_POINT('Ctrl Pts',(-2.02964932608798,4.48054028778274,11.3205992118557));
#24836=CARTESIAN_POINT('Ctrl Pts',(-2.09718952433785,4.44932731821316,11.3247977771892));
#24837=CARTESIAN_POINT('Ctrl Pts',(-2.22795273842943,4.38525737579467,11.3330384974887));
#24838=CARTESIAN_POINT('Ctrl Pts',(-2.29122154266443,4.35253481793322,11.3370787008989));
#24839=CARTESIAN_POINT('Ctrl Pts',(-2.51875745094776,4.22851712706546,11.3518150964457));
#24840=CARTESIAN_POINT('Ctrl Pts',(-2.6784662105056,4.12920248928634,11.3625647005813));
#24841=CARTESIAN_POINT('Ctrl Pts',(-2.8995403429102,3.97349390074871,11.3780432902847));
#24842=CARTESIAN_POINT('Ctrl Pts',(-2.96577752162708,3.92430271529468,11.382763090999));
#24843=CARTESIAN_POINT('Ctrl Pts',(-3.05246605767687,3.85647437199492,11.3890443829365));
#24844=CARTESIAN_POINT('Ctrl Pts',(-3.07404252703777,3.83929761387948,11.3906166475733));
#24845=CARTESIAN_POINT('Ctrl Pts',(-3.12926427750536,3.79457230357593,11.3946629082647));
#24846=CARTESIAN_POINT('Ctrl Pts',(-3.16269093105303,3.76675722858857,11.3971338348229));
#24847=CARTESIAN_POINT('Ctrl Pts',(-3.22289155969841,3.71529655936839,11.4016214305927));
#24848=CARTESIAN_POINT('Ctrl Pts',(-3.24978513776297,3.69179564939717,11.4036401256431));
#24849=CARTESIAN_POINT('Ctrl Pts',(-3.40891153078802,3.54965703426927,11.4156782168946));
#24850=CARTESIAN_POINT('Ctrl Pts',(-3.53489477033996,3.42421720426567,11.4256054723474));
#24851=CARTESIAN_POINT('Ctrl Pts',(-3.72659081949087,3.21146750948727,11.4416530757779));
#24852=CARTESIAN_POINT('Ctrl Pts',(-3.79666723299588,3.12830949722579,11.44775029539));
#24853=CARTESIAN_POINT('Ctrl Pts',(-3.91163141969075,2.98232579894194,11.4582088664809));
#24854=CARTESIAN_POINT('Ctrl Pts',(-3.95790174523656,2.92064053281702,11.4625577215321));
#24855=CARTESIAN_POINT('Ctrl Pts',(-4.04280236092864,2.80173061052302,11.4708225852292));
#24856=CARTESIAN_POINT('Ctrl Pts',(-4.08171541248564,2.74473031292967,11.4747351791655));
#24857=CARTESIAN_POINT('Ctrl Pts',(-4.24019973466902,2.5017531242543,11.491222555841));
#24858=CARTESIAN_POINT('Ctrl Pts',(-4.34835849498808,2.30864422782793,11.5038790772387));
#24859=CARTESIAN_POINT('Ctrl Pts',(-4.46431287622472,2.06434684620571,11.5193521263622));
#24860=CARTESIAN_POINT('Ctrl Pts',(-4.48479716282679,2.01945829355026,11.5221733657652));
#24861=CARTESIAN_POINT('Ctrl Pts',(-4.52960675793347,1.91721821393183,11.528547176138));
#24862=CARTESIAN_POINT('Ctrl Pts',(-4.55352502141188,1.85969703877645,11.5320968015898));
#24863=CARTESIAN_POINT('Ctrl Pts',(-4.58863643128285,1.77051535587367,11.5375394989834));
#24864=CARTESIAN_POINT('Ctrl Pts',(-4.60060866329848,1.73916902174103,11.5394409567526));
#24865=CARTESIAN_POINT('Ctrl Pts',(-4.63105907937749,1.65692680613651,11.5443999699896));
#24866=CARTESIAN_POINT('Ctrl Pts',(-4.64901924671663,1.60584394675804,11.5474513627748));
#24867=CARTESIAN_POINT('Ctrl Pts',(-4.70267021721186,1.44479754551616,11.5569987762822));
#24868=CARTESIAN_POINT('Ctrl Pts',(-4.73532314901596,1.33388612096574,11.5634697876258));
#24869=CARTESIAN_POINT('Ctrl Pts',(-4.76403460025573,1.22194819451,11.5699436565254));
#24870=CARTESIAN_POINT('Origin',(0.,0.,-3.23514056400928));
#24871=CARTESIAN_POINT('',(-4.76403458702644,1.22194824608729,13.6654522135017));
#24872=CARTESIAN_POINT('',(-4.76403458795361,1.2219482424725,13.3199864568809));
#24873=CARTESIAN_POINT('',(-4.76403458704967,1.22194824599672,-3.23514056400928));
#24874=CARTESIAN_POINT('',(-4.91824987725453,7.97280680624427E-5,11.9853488470161));
#24875=CARTESIAN_POINT('Ctrl Pts',(-4.76403458702644,1.22194824608729,13.6654522135017));
#24876=CARTESIAN_POINT('Ctrl Pts',(-4.74749192885731,1.28644344539825,13.6616823062681));
#24877=CARTESIAN_POINT('Ctrl Pts',(-4.72964128849383,1.35059602842922,13.6579039764822));
#24878=CARTESIAN_POINT('Ctrl Pts',(-4.69919306528571,1.45200268377938,13.6518820798644));
#24879=CARTESIAN_POINT('Ctrl Pts',(-4.68744182409409,1.48950205793768,13.6496443602594));
#24880=CARTESIAN_POINT('Ctrl Pts',(-4.6434992367366,1.62405449416783,13.6415748319803));
#24881=CARTESIAN_POINT('Ctrl Pts',(-4.60873278690012,1.72023835122265,13.6357297656318));
#24882=CARTESIAN_POINT('Ctrl Pts',(-4.51090312638626,1.96658149489708,13.6205600978903));
#24883=CARTESIAN_POINT('Ctrl Pts',(-4.4433355123608,2.11481917321635,13.6112319379519));
#24884=CARTESIAN_POINT('Ctrl Pts',(-4.35198178344643,2.29144862239404,13.5999189376336));
#24885=CARTESIAN_POINT('Ctrl Pts',(-4.33507169156301,2.32328123492653,13.5978721073683));
#24886=CARTESIAN_POINT('Ctrl Pts',(-4.29781068710802,2.39160019774105,13.5934635259008));
#24887=CARTESIAN_POINT('Ctrl Pts',(-4.27734166387624,2.42801905918483,13.5911036349509));
#24888=CARTESIAN_POINT('Ctrl Pts',(-4.19183988926921,2.57570783617989,13.5814827167307));
#24889=CARTESIAN_POINT('Ctrl Pts',(-4.1229090377552,2.68466278955151,13.5742644366832));
#24890=CARTESIAN_POINT('Ctrl Pts',(-3.96478163196837,2.91412539207323,13.5586525581168));
#24891=CARTESIAN_POINT('Ctrl Pts',(-3.87419582731745,3.03351715070708,13.5502656369448));
#24892=CARTESIAN_POINT('Ctrl Pts',(-3.72929977990374,3.20739233238047,13.5375263805228));
#24893=CARTESIAN_POINT('Ctrl Pts',(-3.67893017903384,3.26504440652756,13.5332087834669));
#24894=CARTESIAN_POINT('Ctrl Pts',(-3.5806066494643,3.3724184769856,13.5249734352092));
#24895=CARTESIAN_POINT('Ctrl Pts',(-3.53291052514645,3.42235203319116,13.5210589017055));
#24896=CARTESIAN_POINT('Ctrl Pts',(-3.39356557741864,3.56221541485905,13.509838407936));
#24897=CARTESIAN_POINT('Ctrl Pts',(-3.29942630375064,3.6495823514634,13.502512343544));
#24898=CARTESIAN_POINT('Ctrl Pts',(-3.07913823650141,3.83852593340706,13.48591173545));
#24899=CARTESIAN_POINT('Ctrl Pts',(-2.95117266312915,3.93776000823887,13.4766355023107));
#24900=CARTESIAN_POINT('Ctrl Pts',(-2.77680396093254,4.05969673197617,13.4645030830632));
#24901=CARTESIAN_POINT('Ctrl Pts',(-2.73460852932787,4.08823850441202,13.4616044135441));
#24902=CARTESIAN_POINT('Ctrl Pts',(-2.66383415509746,4.13452554071916,13.4568069408464));
#24903=CARTESIAN_POINT('Ctrl Pts',(-2.63550333433586,4.15264205639874,13.4549035835955));
#24904=CARTESIAN_POINT('Ctrl Pts',(-2.54954786919555,4.20637343198898,13.4491772771134));
#24905=CARTESIAN_POINT('Ctrl Pts',(-2.49137087827708,4.24108984875067,13.4453657170116));
#24906=CARTESIAN_POINT('Ctrl Pts',(-2.33420051716059,4.33052901406561,13.4352096473382));
#24907=CARTESIAN_POINT('Ctrl Pts',(-2.23400566223528,4.38305743858922,13.4288803637976));
#24908=CARTESIAN_POINT('Ctrl Pts',(-2.00385315194508,4.49377408594179,13.4145700730411));
#24909=CARTESIAN_POINT('Ctrl Pts',(-1.8730018093682,4.54986774438346,13.4065905002074));
#24910=CARTESIAN_POINT('Ctrl Pts',(-1.68083098074824,4.62255114599162,13.3950083199938));
#24911=CARTESIAN_POINT('Ctrl Pts',(-1.62133349472312,4.64375381287817,13.3914411017798));
#24912=CARTESIAN_POINT('Ctrl Pts',(-1.49323006352035,4.68664291922593,13.3837931639312));
#24913=CARTESIAN_POINT('Ctrl Pts',(-1.4245232187835,4.70798166017359,13.379710884901));
#24914=CARTESIAN_POINT('Ctrl Pts',(-1.3167466528588,4.73887919072883,13.3733327120224));
#24915=CARTESIAN_POINT('Ctrl Pts',(-1.27798555888444,4.74947898389579,13.3710439471497));
#24916=CARTESIAN_POINT('Ctrl Pts',(-1.05082889829543,4.80861619264809,13.357658845234));
#24917=CARTESIAN_POINT('Ctrl Pts',(-0.859817066022298,4.84641565524565,
13.3465076622931));
#24918=CARTESIAN_POINT('Ctrl Pts',(-0.591882408590292,4.88309508910117,
13.331049422339));
#24919=CARTESIAN_POINT('Ctrl Pts',(-0.516464281686567,4.8916466849467,13.3267192545723));
#24920=CARTESIAN_POINT('Ctrl Pts',(-0.403585365849269,4.90180618895677,
13.3202781422558));
#24921=CARTESIAN_POINT('Ctrl Pts',(-0.366255447635611,4.90473669682284,
13.3181547095109));
#24922=CARTESIAN_POINT('Ctrl Pts',(-0.27795668760385,4.91065469496709,13.3131485036964));
#24923=CARTESIAN_POINT('Ctrl Pts',(-0.226967635776463,4.91327540780572,
13.3102697912342));
#24924=CARTESIAN_POINT('Ctrl Pts',(-0.140415964614919,4.91637371095197,
13.3053961082695));
#24925=CARTESIAN_POINT('Ctrl Pts',(-0.104872408415938,4.91726030488352,
13.3033983327393));
#24926=CARTESIAN_POINT('Ctrl Pts',(0.0610761293950787,4.91959956527556,
13.2940812658211));
#24927=CARTESIAN_POINT('Ctrl Pts',(0.191496361446129,4.9162505555357,13.2867872464725));
#24928=CARTESIAN_POINT('Ctrl Pts',(0.446495422878773,4.89953910154356,13.2724617233754));
#24929=CARTESIAN_POINT('Ctrl Pts',(0.571002444413348,4.88659361992049,13.2654368436197));
#24930=CARTESIAN_POINT('Ctrl Pts',(0.762398595181521,4.85927805447106,13.254532842792));
#24931=CARTESIAN_POINT('Ctrl Pts',(0.829710012372377,4.84823844164387,13.2506780241328));
#24932=CARTESIAN_POINT('Ctrl Pts',(0.972159468716897,4.82182207549118,13.2424690479482));
#24933=CARTESIAN_POINT('Ctrl Pts',(1.04721149933344,4.80608052825962,13.2381134273332));
#24934=CARTESIAN_POINT('Ctrl Pts',(1.22735954459834,4.76387570462259,13.2275765077693));
#24935=CARTESIAN_POINT('Ctrl Pts',(1.33200848961411,4.73568117491051,13.2213868525684));
#24936=CARTESIAN_POINT('Ctrl Pts',(1.6052055281734,4.65230361057469,13.2050433057154));
#24937=CARTESIAN_POINT('Ctrl Pts',(1.77185022306973,4.59142258506078,13.1948811535334));
#24938=CARTESIAN_POINT('Ctrl Pts',(1.96747457287629,4.50771411765555,13.1827782696507));
#24939=CARTESIAN_POINT('Ctrl Pts',(1.99995312058972,4.49339852621279,13.1807631771229));
#24940=CARTESIAN_POINT('Ctrl Pts',(2.07115662570032,4.46108915328266,13.1763343761193));
#24941=CARTESIAN_POINT('Ctrl Pts',(2.10980805224177,4.44294004476959,13.173922868979));
#24942=CARTESIAN_POINT('Ctrl Pts',(2.17242820236224,4.41253476556097,13.1699992674948));
#24943=CARTESIAN_POINT('Ctrl Pts',(2.19654107435516,4.40058117421988,13.1684843416449));
#24944=CARTESIAN_POINT('Ctrl Pts',(2.29152426996722,4.3525194823362,13.1624980852108));
#24945=CARTESIAN_POINT('Ctrl Pts',(2.36161269585703,4.31489222868149,13.1580389499542));
#24946=CARTESIAN_POINT('Ctrl Pts',(2.59173293086761,4.18406403501136,13.1432059270431));
#24947=CARTESIAN_POINT('Ctrl Pts',(2.74740947404174,4.08352931826245,13.1328484107231));
#24948=CARTESIAN_POINT('Ctrl Pts',(2.95545620293753,3.93188076414463,13.118344545202));
#24949=CARTESIAN_POINT('Ctrl Pts',(3.01292118538963,3.88802179553499,13.1142637510599));
#24950=CARTESIAN_POINT('Ctrl Pts',(3.12533421853084,3.7982356374216,13.106119618944));
#24951=CARTESIAN_POINT('Ctrl Pts',(3.18028764362498,3.75234303859302,13.1020574643793));
#24952=CARTESIAN_POINT('Ctrl Pts',(3.35099333965024,3.60333905172189,13.0891685015358));
#24953=CARTESIAN_POINT('Ctrl Pts',(3.46288227067792,3.4959482254365,13.0803096231098));
#24954=CARTESIAN_POINT('Ctrl Pts',(3.66800678810294,3.2795438821689,13.063241615592));
#24955=CARTESIAN_POINT('Ctrl Pts',(3.76191818507742,3.17138047154007,13.0550430351599));
#24956=CARTESIAN_POINT('Ctrl Pts',(3.87666621726056,3.02693701312246,13.0445438587821));
#24957=CARTESIAN_POINT('Ctrl Pts',(3.901946908681,2.99427771260203,13.0421981252545));
#24958=CARTESIAN_POINT('Ctrl Pts',(3.95239700468902,2.92737875823166,13.0374520257537));
#24959=CARTESIAN_POINT('Ctrl Pts',(3.97754005276687,2.89312351305757,13.0350521510918));
#24960=CARTESIAN_POINT('Ctrl Pts',(4.01776101058695,2.83681035728992,13.0311514458086));
#24961=CARTESIAN_POINT('Ctrl Pts',(4.03310850865928,2.8149480118026,13.0296477866961));
#24962=CARTESIAN_POINT('Ctrl Pts',(4.1354899661822,2.66655051408254,13.0195087346167));
#24963=CARTESIAN_POINT('Ctrl Pts',(4.21673445644975,2.53612303329006,13.0109235433458));
#24964=CARTESIAN_POINT('Ctrl Pts',(4.35249344802412,2.29356823095315,12.9953430469677));
#24965=CARTESIAN_POINT('Ctrl Pts',(4.40910351243269,2.18276432951868,12.9883619678482));
#24966=CARTESIAN_POINT('Ctrl Pts',(4.48787769374794,2.01297772182069,12.9778091183968));
#24967=CARTESIAN_POINT('Ctrl Pts',(4.51321019853709,1.95552016111104,12.9742621889819));
#24968=CARTESIAN_POINT('Ctrl Pts',(4.56541863483289,1.83068184306081,12.9666006158049));
#24969=CARTESIAN_POINT('Ctrl Pts',(4.59191801686957,1.76315968731107,12.9624841529034));
#24970=CARTESIAN_POINT('Ctrl Pts',(4.6440764643316,1.62109468921444,12.9538735269379));
#24971=CARTESIAN_POINT('Ctrl Pts',(4.66945625275408,1.54647092762302,12.9493787472607));
#24972=CARTESIAN_POINT('Ctrl Pts',(4.74502419619914,1.30542562236449,12.9349452274976));
#24973=CARTESIAN_POINT('Ctrl Pts',(4.78818893692642,1.13694206772998,12.9249808123392));
#24974=CARTESIAN_POINT('Ctrl Pts',(4.83458759626187,0.905443052705651,12.9114995120545));
#24975=CARTESIAN_POINT('Ctrl Pts',(4.84566905186505,0.844130275520592,12.9079491985528));
#24976=CARTESIAN_POINT('Ctrl Pts',(4.8614332198621,0.746325563740343,12.9023232632492));
#24977=CARTESIAN_POINT('Ctrl Pts',(4.86687647517669,0.70996353186131,12.9002401439926));
#24978=CARTESIAN_POINT('Ctrl Pts',(4.87992672603027,0.615567730797254,12.8948534607081));
#24979=CARTESIAN_POINT('Ctrl Pts',(4.88690645051748,0.557453090019006,12.8915568186201));
#24980=CARTESIAN_POINT('Ctrl Pts',(4.89736161935942,0.454983635883838,12.8857665460685));
#24981=CARTESIAN_POINT('Ctrl Pts',(4.90127558706457,0.410680641534235,12.8832704705766));
#24982=CARTESIAN_POINT('Ctrl Pts',(4.91802246773135,0.186466304784413,12.8706612384507));
#24983=CARTESIAN_POINT('Ctrl Pts',(4.92155243729071,0.00599995829114273,
12.860582500595));
#24984=CARTESIAN_POINT('Ctrl Pts',(4.91219488473717,-0.257951611378148,
12.8457330282399));
#24985=CARTESIAN_POINT('Ctrl Pts',(4.90709006754119,-0.341561794685724,
12.8410142512721));
#24986=CARTESIAN_POINT('Ctrl Pts',(4.89401672904728,-0.492285135535927,
12.8324639582707));
#24987=CARTESIAN_POINT('Ctrl Pts',(4.88679532867845,-0.559442292800807,
12.8286385052027));
#24988=CARTESIAN_POINT('Ctrl Pts',(4.86531875422939,-0.726686941079942,
12.8190644922807));
#24989=CARTESIAN_POINT('Ctrl Pts',(4.84935660262994,-0.826523222251747,
12.8133064074555));
#24990=CARTESIAN_POINT('Ctrl Pts',(4.80165815682912,-1.07538939964532,12.7988339658511));
#24991=CARTESIAN_POINT('Ctrl Pts',(4.76605277958366,-1.22357019038186,12.7901065841066));
#24992=CARTESIAN_POINT('Ctrl Pts',(4.70161958018936,-1.4457526491025,12.7768774393197));
#24993=CARTESIAN_POINT('Ctrl Pts',(4.67778410044732,-1.52110601934953,12.7723656677487));
#24994=CARTESIAN_POINT('Ctrl Pts',(4.64067093286858,-1.6292962990354,12.7658602060999));
#24995=CARTESIAN_POINT('Ctrl Pts',(4.62883825429193,-1.66261528688749,12.7638529339004));
#24996=CARTESIAN_POINT('Ctrl Pts',(4.60183688074375,-1.73612367217808,12.7594175770459));
#24997=CARTESIAN_POINT('Ctrl Pts',(4.58649884049838,-1.77624787853159,12.7569917875394));
#24998=CARTESIAN_POINT('Ctrl Pts',(4.49952794048236,-1.995122337446,12.7437176441949));
#24999=CARTESIAN_POINT('Ctrl Pts',(4.41796940105603,-2.16974947306241,12.7329671455295));
#25000=CARTESIAN_POINT('Ctrl Pts',(4.26993253241486,-2.44355201436016,12.7155139950434));
#25001=CARTESIAN_POINT('Ctrl Pts',(4.2097228480303,-2.54587967292014,12.7088480930045));
#25002=CARTESIAN_POINT('Ctrl Pts',(4.10936563073724,-2.70312812961401,12.6983253542854));
#25003=CARTESIAN_POINT('Ctrl Pts',(4.07168048033703,-2.75956618021655,12.6944895072439));
#25004=CARTESIAN_POINT('Ctrl Pts',(3.98832199442357,-2.87897891029431,12.6862366513769));
#25005=CARTESIAN_POINT('Ctrl Pts',(3.94229796858069,-2.94168632331191,12.6818177618071));
#25006=CARTESIAN_POINT('Ctrl Pts',(3.83999919904504,-3.07435278892578,12.6722754356151));
#25007=CARTESIAN_POINT('Ctrl Pts',(3.78325664268296,-3.14391600934878,12.6671500171384));
#25008=CARTESIAN_POINT('Ctrl Pts',(3.61833640537448,-3.33516463603254,12.6527060716879));
#25009=CARTESIAN_POINT('Ctrl Pts',(3.50597492077443,-3.45308871233971,12.6433751181095));
#25010=CARTESIAN_POINT('Ctrl Pts',(3.35064211424312,-3.60069889886854,12.631154725642));
#25011=CARTESIAN_POINT('Ctrl Pts',(3.31275596473747,-3.63558566699827,12.6282236560214));
#25012=CARTESIAN_POINT('Ctrl Pts',(3.24658032947463,-3.6946288219731,12.623191489593));
#25013=CARTESIAN_POINT('Ctrl Pts',(3.2185522060674,-3.71907081052029,12.621086705534));
#25014=CARTESIAN_POINT('Ctrl Pts',(3.13554260286828,-3.78981825227685,12.6149268125057));
#25015=CARTESIAN_POINT('Ctrl Pts',(3.07981988626181,-3.83523916666179,12.6108839731272));
#25016=CARTESIAN_POINT('Ctrl Pts',(2.92244037331296,-3.95788043731194,12.5996823954742));
#25017=CARTESIAN_POINT('Ctrl Pts',(2.81874315776881,-4.03238918151887,12.5925427107956));
#25018=CARTESIAN_POINT('Ctrl Pts',(2.60885187264373,-4.1711440777764,12.5784392148485));
#25019=CARTESIAN_POINT('Ctrl Pts',(2.50289203306217,-4.23557339000261,12.5714813480575));
#25020=CARTESIAN_POINT('Ctrl Pts',(2.33978305097612,-4.32649265170639,12.5609528563646));
#25021=CARTESIAN_POINT('Ctrl Pts',(2.28437404045716,-4.35600258589951,12.5574068526786));
#25022=CARTESIAN_POINT('Ctrl Pts',(2.16373385446374,-4.41731857350783,12.5497445250737));
#25023=CARTESIAN_POINT('Ctrl Pts',(2.09833290915234,-4.44875785021114,12.5456263695164));
#25024=CARTESIAN_POINT('Ctrl Pts',(1.96043738859697,-4.51132896922765,12.5370105387455));
#25025=CARTESIAN_POINT('Ctrl Pts',(1.88784079521458,-4.5421867842771,12.5325122395333));
#25026=CARTESIAN_POINT('Ctrl Pts',(1.65255721292173,-4.63558066923525,12.5180484002647));
#25027=CARTESIAN_POINT('Ctrl Pts',(1.48727781368162,-4.69122138437479,12.5080570534598));
#25028=CARTESIAN_POINT('Ctrl Pts',(1.25976308759379,-4.75457797612843,12.4945723732099));
#25029=CARTESIAN_POINT('Ctrl Pts',(1.19982256219548,-4.77005667889414,12.4910449594774));
#25030=CARTESIAN_POINT('Ctrl Pts',(1.10435164529871,-4.79279707934915,12.4854717228737));
#25031=CARTESIAN_POINT('Ctrl Pts',(1.0690061064841,-4.8008043477951,12.4834183982528));
#25032=CARTESIAN_POINT('Ctrl Pts',(1.03206036881866,-4.80874587155152,12.4812821856536));
#25033=CARTESIAN_POINT('Ctrl Pts',(1.03054575847516,-4.80907069003373,12.4811946274699));
#25034=CARTESIAN_POINT('Ctrl Pts',(1.0275309130035,-4.80971575444775,12.4810203756845));
#25035=CARTESIAN_POINT('Ctrl Pts',(1.02603068100881,-4.81003601414708,12.4809336819387));
#25036=CARTESIAN_POINT('Ctrl Pts',(1.02302498124307,-4.81067618106065,12.4807600247561));
#25037=CARTESIAN_POINT('Ctrl Pts',(1.02151951264981,-4.81099608361409,12.4806730613798));
#25038=CARTESIAN_POINT('Ctrl Pts',(1.01848616054647,-4.81163916375126,12.4804978728357));
#25039=CARTESIAN_POINT('Ctrl Pts',(1.01695827276544,-4.81196232038722,12.4804096479059));
#25040=CARTESIAN_POINT('Ctrl Pts',(1.01386422637074,-4.81261518870416,12.4802310220451));
#25041=CARTESIAN_POINT('Ctrl Pts',(1.01229806019504,-4.81294486373869,12.4801406215189));
#25042=CARTESIAN_POINT('Ctrl Pts',(1.00911215003705,-4.81361386796449,12.4799567633444));
#25043=CARTESIAN_POINT('Ctrl Pts',(1.0074923951227,-4.81395314424492,12.4798633062699));
#25044=CARTESIAN_POINT('Ctrl Pts',(1.00418396726489,-4.81464438955609,12.4796724533781));
#25045=CARTESIAN_POINT('Ctrl Pts',(1.00249527973445,-4.81499628786041,12.4795750583155));
#25046=CARTESIAN_POINT('Ctrl Pts',(0.999033141422483,-4.81571584763252,
12.4793754202129));
#25047=CARTESIAN_POINT('Ctrl Pts',(0.997259671934652,-4.81608341804172,
12.4792731781301));
#25048=CARTESIAN_POINT('Ctrl Pts',(0.993611208404693,-4.81683749923351,
12.4790628856171));
#25049=CARTESIAN_POINT('Ctrl Pts',(0.991736190854317,-4.81722389507111,
12.4789548363763));
#25050=CARTESIAN_POINT('Ctrl Pts',(0.987866570630245,-4.81801897532477,
12.4787318962226));
#25051=CARTESIAN_POINT('Ctrl Pts',(0.985871938743684,-4.81842751614692,
12.4786170067716));
#25052=CARTESIAN_POINT('Ctrl Pts',(0.983160138138206,-4.81898119322629,
12.4784608453657));
#25053=CARTESIAN_POINT('Ctrl Pts',(0.982443190469378,-4.81912740808886,
12.4784195627736));
#25054=CARTESIAN_POINT('Ctrl Pts',(0.980876210056647,-4.81944661507176,
12.4783293419559));
#25055=CARTESIAN_POINT('Ctrl Pts',(0.980026164088165,-4.81961954231709,
12.4782804043685));
#25056=CARTESIAN_POINT('Ctrl Pts',(0.97816224901603,-4.81999821030666,12.4781731083966));
#25057=CARTESIAN_POINT('Ctrl Pts',(0.977148360607587,-4.82020385607519,
12.4781147509397));
#25058=CARTESIAN_POINT('Ctrl Pts',(0.97491720136122,-4.82065566653902,12.4779863447503));
#25059=CARTESIAN_POINT('Ctrl Pts',(0.973699901940516,-4.82090169012053,
12.4779162973843));
#25060=CARTESIAN_POINT('Ctrl Pts',(0.971010559042593,-4.82144416243935,
12.4777615654374));
#25061=CARTESIAN_POINT('Ctrl Pts',(0.969538472613948,-4.82174039817744,
12.4776768828985));
#25062=CARTESIAN_POINT('Ctrl Pts',(0.966272314896894,-4.8223961081474,12.4774890269009));
#25063=CARTESIAN_POINT('Ctrl Pts',(0.964478178039828,-4.82275525550491,
12.4773858565377));
#25064=CARTESIAN_POINT('Ctrl Pts',(0.960479238258706,-4.82355343593039,
12.4771559471917));
#25065=CARTESIAN_POINT('Ctrl Pts',(0.958274333638604,-4.8239919587307,12.4770292129689));
#25066=CARTESIAN_POINT('Ctrl Pts',(0.953336206927131,-4.82497055962427,
12.4767454471985));
#25067=CARTESIAN_POINT('Ctrl Pts',(0.950602824633124,-4.82550982741635,
12.476588423069));
#25068=CARTESIAN_POINT('Ctrl Pts',(0.944451063516573,-4.82671807587247,
12.4762351294651));
#25069=CARTESIAN_POINT('Ctrl Pts',(0.941032428649438,-4.82738574837216,
12.4760388716879));
#25070=CARTESIAN_POINT('Ctrl Pts',(0.933301291381195,-4.82888714454379,
12.4755952031977));
#25071=CARTESIAN_POINT('Ctrl Pts',(0.928988374639183,-4.82971872421858,
12.4753478110885));
#25072=CARTESIAN_POINT('Ctrl Pts',(0.865270786774493,-4.84191569676271,
12.4716945667584));
#25073=CARTESIAN_POINT('Ctrl Pts',(0.805662146167855,-4.85219020093511,
12.4682979459368));
#25074=CARTESIAN_POINT('Ctrl Pts',(0.559009464096017,-4.89003412043751,
12.4543003172029));
#25075=CARTESIAN_POINT('Ctrl Pts',(0.370643022856385,-4.90790676089643,
12.4437392596268));
#25076=CARTESIAN_POINT('Ctrl Pts',(0.100342408565345,-4.91790049558818,
12.4285293816744));
#25077=CARTESIAN_POINT('Ctrl Pts',(0.0189066834802143,-4.91888770038409,
12.4239408807574));
#25078=CARTESIAN_POINT('Ctrl Pts',(-0.0876736691723155,-4.91753286074616,
12.4179166280193));
#25079=CARTESIAN_POINT('Ctrl Pts',(-0.112829152108404,-4.91702000038844,
12.4164933998463));
#25080=CARTESIAN_POINT('Ctrl Pts',(-0.180391203396617,-4.91512382793135,
12.4126667597681));
#25081=CARTESIAN_POINT('Ctrl Pts',(-0.222785502628914,-4.91338476168384,
12.4102611712456));
#25082=CARTESIAN_POINT('Ctrl Pts',(-0.332222403201716,-4.90747622692522,
12.4040380914457));
#25083=CARTESIAN_POINT('Ctrl Pts',(-0.39921132557982,-4.90248149802811,
12.4002158304595));
#25084=CARTESIAN_POINT('Ctrl Pts',(-0.570674863714475,-4.88615935420432,
12.390394935081));
#25085=CARTESIAN_POINT('Ctrl Pts',(-0.674926651024151,-4.87285304146652,
12.3843874288826));
#25086=CARTESIAN_POINT('Ctrl Pts',(-0.916141303239926,-4.83417542507247,
12.3704048357757));
#25087=CARTESIAN_POINT('Ctrl Pts',(-1.05261408047837,-4.8063053365427,12.3624303166353));
#25088=CARTESIAN_POINT('Ctrl Pts',(-1.2334267554739,-4.76130863294554,12.3518126371884));
#25089=CARTESIAN_POINT('Ctrl Pts',(-1.27896721060993,-4.74927830348323,
12.3491341119404));
#25090=CARTESIAN_POINT('Ctrl Pts',(-1.35785592567837,-4.72722141786824,
12.3444894413808));
#25091=CARTESIAN_POINT('Ctrl Pts',(-1.3912831187497,-4.7174915317498,12.3425201818188));
#25092=CARTESIAN_POINT('Ctrl Pts',(-1.42821352579923,-4.70631526832061,
12.3403417923546));
#25093=CARTESIAN_POINT('Ctrl Pts',(-1.43182125024315,-4.70521893087799,
12.3401289559409));
#25094=CARTESIAN_POINT('Ctrl Pts',(-1.43666410257372,-4.70374116952377,
12.3398432108308));
#25095=CARTESIAN_POINT('Ctrl Pts',(-1.43790034396326,-4.7033634065771,12.33977026455));
#25096=CARTESIAN_POINT('Ctrl Pts',(-1.44077493814102,-4.70248376671346,
12.3396006359168));
#25097=CARTESIAN_POINT('Ctrl Pts',(-1.44241317806771,-4.70198152083979,
12.3395039573316));
#25098=CARTESIAN_POINT('Ctrl Pts',(-1.4462810280311,-4.70079351725624,12.339275684959));
#25099=CARTESIAN_POINT('Ctrl Pts',(-1.44851041371257,-4.70010702913194,
12.3391440985326));
#25100=CARTESIAN_POINT('Ctrl Pts',(-1.45386623397875,-4.69845365473027,
12.3388279468481));
#25101=CARTESIAN_POINT('Ctrl Pts',(-1.45699219436929,-4.69748523334786,
12.3386433967852));
#25102=CARTESIAN_POINT('Ctrl Pts',(-1.46464670555598,-4.6951054929536,12.3381914239928));
#25103=CARTESIAN_POINT('Ctrl Pts',(-1.46917418737869,-4.69369074069278,
12.3379240343906));
#25104=CARTESIAN_POINT('Ctrl Pts',(-1.48047711262466,-4.69014083443975,
12.3372563401194));
#25105=CARTESIAN_POINT('Ctrl Pts',(-1.48724999382016,-4.68799754521871,
12.336856111036));
#25106=CARTESIAN_POINT('Ctrl Pts',(-1.50443382134391,-4.68251870821666,
12.3358402907139));
#25107=CARTESIAN_POINT('Ctrl Pts',(-1.51483834221053,-4.67916310607729,
12.3352248752226));
#25108=CARTESIAN_POINT('Ctrl Pts',(-1.5916787829674,-4.65409784462052,12.3306769121839));
#25109=CARTESIAN_POINT('Ctrl Pts',(-1.65765679325125,-4.63100876370727,
12.3267554908878));
#25110=CARTESIAN_POINT('Ctrl Pts',(-1.91862173391321,-4.53339191868338,
12.3111365036432));
#25111=CARTESIAN_POINT('Ctrl Pts',(-2.10926747445009,-4.44789178569794,
12.2994723947233));
#25112=CARTESIAN_POINT('Ctrl Pts',(-2.35092203219417,-4.3204749469813,12.2840760735682));
#25113=CARTESIAN_POINT('Ctrl Pts',(-2.40734458242593,-4.28929249607858,
12.2804361716082));
#25114=CARTESIAN_POINT('Ctrl Pts',(-2.51881371244413,-4.22479563607489,
12.2731468599012));
#25115=CARTESIAN_POINT('Ctrl Pts',(-2.57385214466697,-4.1914920619834,12.2694981899941));
#25116=CARTESIAN_POINT('Ctrl Pts',(-2.68987632584927,-4.11813904582324,
12.2616946098737));
#25117=CARTESIAN_POINT('Ctrl Pts',(-2.75065628212739,-4.07779275108807,
12.2575383117097));
#25118=CARTESIAN_POINT('Ctrl Pts',(-2.92141966976215,-3.95888290034441,
12.2456589273973));
#25119=CARTESIAN_POINT('Ctrl Pts',(-3.02909274183899,-3.87711793944665,
12.2379201759736));
#25120=CARTESIAN_POINT('Ctrl Pts',(-3.2111578411961,-3.72664208839046,12.2244027498735));
#25121=CARTESIAN_POINT('Ctrl Pts',(-3.28705254872941,-3.65987456558176,
12.2186256206746));
#25122=CARTESIAN_POINT('Ctrl Pts',(-3.39046279915788,-3.56308737395465,
12.2105660014033));
#25123=CARTESIAN_POINT('Ctrl Pts',(-3.41974470013231,-3.53499305131765,
12.2082616629441));
#25124=CARTESIAN_POINT('Ctrl Pts',(-3.45218256253671,-3.50309046547008,
12.2056850005498));
#25125=CARTESIAN_POINT('Ctrl Pts',(-3.45568412320601,-3.49963633754612,
12.205406538103));
#25126=CARTESIAN_POINT('Ctrl Pts',(-3.46130201892822,-3.49407789025903,
12.2049592514128));
#25127=CARTESIAN_POINT('Ctrl Pts',(-3.4634216279619,-3.49197688944594,12.2047903721451));
#25128=CARTESIAN_POINT('Ctrl Pts',(-3.50010584028113,-3.45554847344008,
12.201865473296));
#25129=CARTESIAN_POINT('Ctrl Pts',(-3.53416075469713,-3.42071103463849,
12.1991179495173));
#25130=CARTESIAN_POINT('Ctrl Pts',(-3.63079654163704,-3.31887091832525,
12.191215479791));
#25131=CARTESIAN_POINT('Ctrl Pts',(-3.69202905576581,-3.25061677211752,
12.1860756386855));
#25132=CARTESIAN_POINT('Ctrl Pts',(-3.87536319405307,-3.03439180829279,
12.1701904957235));
#25133=CARTESIAN_POINT('Ctrl Pts',(-3.99074226239509,-2.88096314841509,
12.1594621702696));
#25134=CARTESIAN_POINT('Ctrl Pts',(-4.13096579999139,-2.66985078793095,
12.1451783330193));
#25135=CARTESIAN_POINT('Ctrl Pts',(-4.16409799853801,-2.61787498363122,
12.1416982144141));
#25136=CARTESIAN_POINT('Ctrl Pts',(-4.21350352823815,-2.53705853438356,
12.1363376528447));
#25137=CARTESIAN_POINT('Ctrl Pts',(-4.23047722361203,-2.50865311150036,
12.1344629215847));
#25138=CARTESIAN_POINT('Ctrl Pts',(-4.27952121560959,-2.42466471778734,
12.1289461525333));
#25139=CARTESIAN_POINT('Ctrl Pts',(-4.31079168558416,-2.36862317839646,
12.1252985561602));
#25140=CARTESIAN_POINT('Ctrl Pts',(-4.4164231085557,-2.17029094010327,12.1124994198052));
#25141=CARTESIAN_POINT('Ctrl Pts',(-4.48490615416431,-2.02498683376665,
12.103313244126));
#25142=CARTESIAN_POINT('Ctrl Pts',(-4.55221903231299,-1.86191759123798,
12.0932148872363));
#25143=CARTESIAN_POINT('Ctrl Pts',(-4.55820701822915,-1.84720979155811,
12.0923059573267));
#25144=CARTESIAN_POINT('Ctrl Pts',(-4.60202829792678,-1.73806454732453,
12.0855749718152));
#25145=CARTESIAN_POINT('Ctrl Pts',(-4.63699488322442,-1.64250164090664,
12.0797590196825));
#25146=CARTESIAN_POINT('Ctrl Pts',(-4.68175392539196,-1.50732102509259,
12.0716559901385));
#25147=CARTESIAN_POINT('Ctrl Pts',(-4.69405598062844,-1.46856222239915,
12.0693467976528));
#25148=CARTESIAN_POINT('Ctrl Pts',(-4.71546319001737,-1.39809789665345,
12.0651759736675));
#25149=CARTESIAN_POINT('Ctrl Pts',(-4.72473269007326,-1.36644497124293,
12.0633122071074));
#25150=CARTESIAN_POINT('Ctrl Pts',(-4.78602724535463,-1.14905620733739,
12.0505701575916));
#25151=CARTESIAN_POINT('Ctrl Pts',(-4.82740577608411,-0.960490658908029,
12.0398003807952));
#25152=CARTESIAN_POINT('Ctrl Pts',(-4.87707695667389,-0.647128576719021,
12.0220145408731));
#25153=CARTESIAN_POINT('Ctrl Pts',(-4.89188262449464,-0.523582719061208,
12.0150317542213));
#25154=CARTESIAN_POINT('Ctrl Pts',(-4.90758453802529,-0.330968325508063,
12.0041330333462));
#25155=CARTESIAN_POINT('Ctrl Pts',(-4.91173777046985,-0.262217397667348,
12.0002407800475));
#25156=CARTESIAN_POINT('Ctrl Pts',(-4.91698278804598,-0.128939089868967,
11.992683349764));
#25157=CARTESIAN_POINT('Ctrl Pts',(-4.91825104681945,-0.0644325092458331,
11.9890201256933));
#25158=CARTESIAN_POINT('Ctrl Pts',(-4.9182499993517,7.98561370042354E-5,
11.9853490513894));
#25159=CARTESIAN_POINT('Ctrl Pts',(-4.91824999935358,7.97400756539363E-5,
11.9853490579939));
#25160=CARTESIAN_POINT('Ctrl Pts',(-4.91824586312372,0.255196284351623,
11.9708316583857));
#25161=CARTESIAN_POINT('Ctrl Pts',(-4.89839170797622,0.509925348674778,
11.9561953390914));
#25162=CARTESIAN_POINT('Ctrl Pts',(-4.85195482658824,0.806045273478557,
11.939085497959));
#25163=CARTESIAN_POINT('Ctrl Pts',(-4.84444124173504,0.850037484604231,
11.9365418443026));
#25164=CARTESIAN_POINT('Ctrl Pts',(-4.83040234913672,0.92599125711354,11.9321491905602));
#25165=CARTESIAN_POINT('Ctrl Pts',(-4.82415588900359,0.95800138190684,11.9302976477932));
#25166=CARTESIAN_POINT('Ctrl Pts',(-4.81035161837271,1.02518005234567,11.926412434742));
#25167=CARTESIAN_POINT('Ctrl Pts',(-4.80272542381217,1.06033266985377,11.924379745439));
#25168=CARTESIAN_POINT('Ctrl Pts',(-4.78504506018961,1.1377221099375,11.9199017942449));
#25169=CARTESIAN_POINT('Ctrl Pts',(-4.77481742903138,1.17990896109132,11.9174588098249));
#25170=CARTESIAN_POINT('Ctrl Pts',(-4.76403457734943,1.22194828381523,11.9150196727617));
#25171=CARTESIAN_POINT('Ctrl Pts',(-4.76403460025573,1.22194819451,11.5699436565254));
#25172=CARTESIAN_POINT('Ctrl Pts',(-4.78098833517923,1.15585031888646,11.573766391097));
#25173=CARTESIAN_POINT('Ctrl Pts',(-4.79656778033866,1.08939451803579,11.5775899281936));
#25174=CARTESIAN_POINT('Ctrl Pts',(-4.82747975550792,0.943974298564324,
11.5859302393302));
#25175=CARTESIAN_POINT('Ctrl Pts',(-4.84226688445056,0.864927468062738,
11.5904471333619));
#25176=CARTESIAN_POINT('Ctrl Pts',(-4.86686164324608,0.71291982604495,11.5991204219165));
#25177=CARTESIAN_POINT('Ctrl Pts',(-4.87698231678454,0.64003144261876,11.6032737330627));
#25178=CARTESIAN_POINT('Ctrl Pts',(-4.89275288639956,0.504133468807987,
11.6110173433907));
#25179=CARTESIAN_POINT('Ctrl Pts',(-4.89882984601668,0.441188611407961,
11.6146039360536));
#25180=CARTESIAN_POINT('Ctrl Pts',(-4.91339697047539,0.252285496999654,
11.6253741599271));
#25181=CARTESIAN_POINT('Ctrl Pts',(-4.9182533146826,0.126100836882465,11.6325783485043));
#25182=CARTESIAN_POINT('Ctrl Pts',(-4.91824505553169,-0.188264015889626,
11.6505610645531));
#25183=CARTESIAN_POINT('Ctrl Pts',(-4.90744522725096,-0.376244584205871,
11.6613490122019));
#25184=CARTESIAN_POINT('Ctrl Pts',(-4.88180002559322,-0.598745212729988,
11.6740888745682));
#25185=CARTESIAN_POINT('Ctrl Pts',(-4.87730769301797,-0.634300423492197,
11.6761235414629));
#25186=CARTESIAN_POINT('Ctrl Pts',(-4.86653706601074,-0.712650395613172,
11.6806030201867));
#25187=CARTESIAN_POINT('Ctrl Pts',(-4.86008203348525,-0.755417955942893,
11.6830455462112));
#25188=CARTESIAN_POINT('Ctrl Pts',(-4.80969175839413,-1.06183157362575,
11.7005471002254));
#25189=CARTESIAN_POINT('Ctrl Pts',(-4.74489296991637,-1.32159540990317,
11.7154186912288));
#25190=CARTESIAN_POINT('Ctrl Pts',(-4.63369466279226,-1.65059275050297,
11.7349555154213));
#25191=CARTESIAN_POINT('Ctrl Pts',(-4.60623475035732,-1.72574154352134,
11.7394655261874));
#25192=CARTESIAN_POINT('Ctrl Pts',(-4.55172547928513,-1.86433076770848,
11.7478863131506));
#25193=CARTESIAN_POINT('Ctrl Pts',(-4.52515110206806,-1.92793708653123,
11.7517926779444));
#25194=CARTESIAN_POINT('Ctrl Pts',(-4.45019806079601,-2.09724330766243,
11.762311836897));
#25195=CARTESIAN_POINT('Ctrl Pts',(-4.39939505592838,-2.20182080367125,
11.7689395942986));
#25196=CARTESIAN_POINT('Ctrl Pts',(-4.24809266901591,-2.48708850108384,
11.7874000729362));
#25197=CARTESIAN_POINT('Ctrl Pts',(-4.13983601864805,-2.66339238904601,
11.7992580880018));
#25198=CARTESIAN_POINT('Ctrl Pts',(-4.00012025100349,-2.86173228450808,
11.8130584137562));
#25199=CARTESIAN_POINT('Ctrl Pts',(-3.97910994721514,-2.8908749122066,11.8150981909489));
#25200=CARTESIAN_POINT('Ctrl Pts',(-3.93220284564366,-2.95445770680338,
11.8195736280161));
#25201=CARTESIAN_POINT('Ctrl Pts',(-3.90616887642156,-2.98879312232786,
11.8220070625958));
#25202=CARTESIAN_POINT('Ctrl Pts',(-3.84731220176153,-3.06433461022059,
11.8274045304857));
#25203=CARTESIAN_POINT('Ctrl Pts',(-3.81427182960623,-3.10536443285343,
11.8303657975174));
#25204=CARTESIAN_POINT('Ctrl Pts',(-3.69826255434059,-3.24478028806058,
11.8405479629783));
#25205=CARTESIAN_POINT('Ctrl Pts',(-3.61209527463768,-3.34043604565295,
11.8477461484402));
#25206=CARTESIAN_POINT('Ctrl Pts',(-3.43613415240409,-3.52099397803826,
11.8618783329864));
#25207=CARTESIAN_POINT('Ctrl Pts',(-3.34669684877314,-3.60611094834908,
11.8688059895568));
#25208=CARTESIAN_POINT('Ctrl Pts',(-3.20676083151303,-3.72959287689251,
11.8793286289782));
#25209=CARTESIAN_POINT('Ctrl Pts',(-3.15856668220214,-3.77049525443292,
11.8828993261185));
#25210=CARTESIAN_POINT('Ctrl Pts',(-3.05255372544539,-3.85700919828873,
11.8906474310381));
#25211=CARTESIAN_POINT('Ctrl Pts',(-2.99447180271443,-3.90227403605745,
11.8948268513807));
#25212=CARTESIAN_POINT('Ctrl Pts',(-2.8707981671648,-3.99426873905427,11.903598033241));
#25213=CARTESIAN_POINT('Ctrl Pts',(-2.80503056586202,-4.04072619965047,
11.9081905427128));
#25214=CARTESIAN_POINT('Ctrl Pts',(-2.58471620400986,-4.18838188256451,
11.9233468428301));
#25215=CARTESIAN_POINT('Ctrl Pts',(-2.4256085924832,-4.28249035704451,11.9339394637194));
#25216=CARTESIAN_POINT('Ctrl Pts',(-2.21405030510433,-4.39204164750832,
11.9475296588114));
#25217=CARTESIAN_POINT('Ctrl Pts',(-2.16611580780215,-4.41587941283665,
11.9505771630055));
#25218=CARTESIAN_POINT('Ctrl Pts',(-2.0874745581742,-4.45339893724738,11.955521989465));
#25219=CARTESIAN_POINT('Ctrl Pts',(-2.05700030704158,-4.46755659030982,
11.9574246712789));
#25220=CARTESIAN_POINT('Ctrl Pts',(-1.96877752544967,-4.50744883454713,
11.9628960658759));
#25221=CARTESIAN_POINT('Ctrl Pts',(-1.91067463309062,-4.53238375841664,
11.9664551840295));
#25222=CARTESIAN_POINT('Ctrl Pts',(-1.70030090263576,-4.61790136053752,
11.979214730734));
#25223=CARTESIAN_POINT('Ctrl Pts',(-1.54550530741354,-4.67198565248014,
11.9883708900171));
#25224=CARTESIAN_POINT('Ctrl Pts',(-1.29012572899634,-4.74712871785957,
12.0033020623864));
#25225=CARTESIAN_POINT('Ctrl Pts',(-1.19107580359823,-4.77294390847587,
12.0090510865457));
#25226=CARTESIAN_POINT('Ctrl Pts',(-1.02969487315582,-4.80966760007122,
12.0183829845819));
#25227=CARTESIAN_POINT('Ctrl Pts',(-0.967832205204608,-4.82249672570205,
12.0219518969845));
#25228=CARTESIAN_POINT('Ctrl Pts',(-0.83330981147716,-4.84770132359213,
12.0297017826942));
#25229=CARTESIAN_POINT('Ctrl Pts',(-0.7605843570137,-4.8596424382312,12.0338847945671));
#25230=CARTESIAN_POINT('Ctrl Pts',(-0.607771056789594,-4.88121912619603,
12.0426670434425));
#25231=CARTESIAN_POINT('Ctrl Pts',(-0.527658800370901,-4.89052776546599,
12.047267044382));
#25232=CARTESIAN_POINT('Ctrl Pts',(-0.2736696191737,-4.91372629632837,12.0618422862466));
#25233=CARTESIAN_POINT('Ctrl Pts',(-0.0992640703909754,-4.92034021057034,
12.0718419787528));
#25234=CARTESIAN_POINT('Ctrl Pts',(0.134840340244993,-4.91676398581778,
12.0852069404104));
#25235=CARTESIAN_POINT('Ctrl Pts',(0.194536257817274,-4.91476406116013,
12.0886093805751));
#25236=CARTESIAN_POINT('Ctrl Pts',(0.291263699719364,-4.90975837487325,
12.0941084845825));
#25237=CARTESIAN_POINT('Ctrl Pts',(0.328323091291363,-4.90741946742565,
12.0962116520858));
#25238=CARTESIAN_POINT('Ctrl Pts',(0.428076507567132,-4.89998873894347,
12.1018644039));
#25239=CARTESIAN_POINT('Ctrl Pts',(0.490705256787886,-4.8941135697492,12.1054054407801));
#25240=CARTESIAN_POINT('Ctrl Pts',(0.650430182585883,-4.87603297592932,
12.114437512945));
#25241=CARTESIAN_POINT('Ctrl Pts',(0.747306182844398,-4.86212820348557,
12.1199170489853));
#25242=CARTESIAN_POINT('Ctrl Pts',(0.995513166931167,-4.81890875823923,
12.1340309761498));
#25243=CARTESIAN_POINT('Ctrl Pts',(1.1459954929802,-4.78535491654709,12.1426622720842));
#25244=CARTESIAN_POINT('Ctrl Pts',(1.36522866154184,-4.72553547851673,12.1554634954052));
#25245=CARTESIAN_POINT('Ctrl Pts',(1.43536552967434,-4.70470620639795,12.1595933574341));
#25246=CARTESIAN_POINT('Ctrl Pts',(1.57372652120927,-4.66023363504856,12.1678200857226));
#25247=CARTESIAN_POINT('Ctrl Pts',(1.64194683410348,-4.63663704932532,12.1719156523649));
#25248=CARTESIAN_POINT('Ctrl Pts',(1.85958908973308,-4.55595131851039,12.185119237694));
#25249=CARTESIAN_POINT('Ctrl Pts',(2.00675268876172,-4.49307316776388,12.1942619777953));
#25250=CARTESIAN_POINT('Ctrl Pts',(2.27439181097747,-4.36294344438658,12.2112979129175));
#25251=CARTESIAN_POINT('Ctrl Pts',(2.39561386256894,-4.29757704330211,12.2191795499294));
#25252=CARTESIAN_POINT('Ctrl Pts',(2.549891981026,-4.20582740307757,12.2293962081102));
#25253=CARTESIAN_POINT('Ctrl Pts',(2.58557525991751,-4.18398540784354,12.2317725510444));
#25254=CARTESIAN_POINT('Ctrl Pts',(2.65726345838225,-4.13883716163471,12.2365714648212));
#25255=CARTESIAN_POINT('Ctrl Pts',(2.69325095242651,-4.11550987157241,12.2389935703404));
#25256=CARTESIAN_POINT('Ctrl Pts',(2.75138682471223,-4.07673672157479,12.242932344316));
#25257=CARTESIAN_POINT('Ctrl Pts',(2.7737210177932,-4.06157401537206,12.2444518840647));
#25258=CARTESIAN_POINT('Ctrl Pts',(2.86147654458704,-4.0009352571259,12.2504503931676));
#25259=CARTESIAN_POINT('Ctrl Pts',(2.92591388801677,-3.95405602066236,12.2549170904686));
#25260=CARTESIAN_POINT('Ctrl Pts',(3.14000352353164,-3.79020203249851,12.2700237200506));
#25261=CARTESIAN_POINT('Ctrl Pts',(3.28400866277456,-3.66613415711815,12.2806463810935));
#25262=CARTESIAN_POINT('Ctrl Pts',(3.47208035656892,-3.48410654873394,12.295395632557));
#25263=CARTESIAN_POINT('Ctrl Pts',(3.52258306560186,-3.43303784337182,12.2994512630649));
#25264=CARTESIAN_POINT('Ctrl Pts',(3.62253383731474,-3.3274384592002,12.307684414492));
#25265=CARTESIAN_POINT('Ctrl Pts',(3.67191242947728,-3.27286679229285,12.3118614417936));
#25266=CARTESIAN_POINT('Ctrl Pts',(3.77265531652826,-3.15637811471549,12.3206252485247));
#25267=CARTESIAN_POINT('Ctrl Pts',(3.82376269945519,-3.09426721189536,12.3252127652597));
#25268=CARTESIAN_POINT('Ctrl Pts',(3.98671683084131,-2.8860229519787,12.3403235018235));
#25269=CARTESIAN_POINT('Ctrl Pts',(4.09188850663947,-2.73486527224022,12.3508753436892));
#25270=CARTESIAN_POINT('Ctrl Pts',(4.21667373355567,-2.53214663193979,12.3644554401123));
#25271=CARTESIAN_POINT('Ctrl Pts',(4.24424416456475,-2.48565796301862,12.367532457769));
#25272=CARTESIAN_POINT('Ctrl Pts',(4.28768432903433,-2.40957932072106,12.3725044562423));
#25273=CARTESIAN_POINT('Ctrl Pts',(4.3040268893569,-2.38026510502099,12.3744049727553));
#25274=CARTESIAN_POINT('Ctrl Pts',(4.34991074104524,-2.29594377058648,12.3798300078691));
#25275=CARTESIAN_POINT('Ctrl Pts',(4.37870643117465,-2.24053819078453,12.3833452321062));
#25276=CARTESIAN_POINT('Ctrl Pts',(4.42844543031621,-2.1402122705825,12.389637498959));
#25277=CARTESIAN_POINT('Ctrl Pts',(4.44977935230398,-2.09549546528303,12.392416683309));
#25278=CARTESIAN_POINT('Ctrl Pts',(4.56237464594534,-1.8500145001232,12.4075567080177));
#25279=CARTESIAN_POINT('Ctrl Pts',(4.6407283960526,-1.64361028202658,12.4198772819986));
#25280=CARTESIAN_POINT('Ctrl Pts',(4.72507273319894,-1.36661456342681,12.4362060421504));
#25281=CARTESIAN_POINT('Ctrl Pts',(4.74378704604622,-1.30016615049333,12.4401069882077));
#25282=CARTESIAN_POINT('Ctrl Pts',(4.7804195390905,-1.15875346003012,12.4483836219702));
#25283=CARTESIAN_POINT('Ctrl Pts',(4.79798677023111,-1.08371735632732,12.4527606428638));
#25284=CARTESIAN_POINT('Ctrl Pts',(4.83607943332904,-0.901856989705154,
12.4633418365647));
#25285=CARTESIAN_POINT('Ctrl Pts',(4.85483828423952,-0.794704454320485,
12.4695544239148));
#25286=CARTESIAN_POINT('Ctrl Pts',(4.89489172648632,-0.510780180795229,
12.4859610607633));
#25287=CARTESIAN_POINT('Ctrl Pts',(4.91016903207596,-0.333320255196364,
12.4961634956557));
#25288=CARTESIAN_POINT('Ctrl Pts',(4.91692035504379,-0.119785444310117,
12.5083148080151));
#25289=CARTESIAN_POINT('Ctrl Pts',(4.91765953992758,-0.0841369180339632,
12.5103390127729));
#25290=CARTESIAN_POINT('Ctrl Pts',(4.91844081732371,-0.00488619640901847,
12.5148276938987));
#25291=CARTESIAN_POINT('Ctrl Pts',(4.91829087786488,0.0387149766614358,
12.5172897548081));
#25292=CARTESIAN_POINT('Ctrl Pts',(4.91666364247416,0.135934692632118,12.5227694176435));
#25293=CARTESIAN_POINT('Ctrl Pts',(4.91488893389383,0.189542748932334,12.5257841141135));
#25294=CARTESIAN_POINT('Ctrl Pts',(4.90558340422741,0.377567595599534,12.5363515755941));
#25295=CARTESIAN_POINT('Ctrl Pts',(4.89341138872779,0.511694248772478,12.5438799646214));
#25296=CARTESIAN_POINT('Ctrl Pts',(4.85980570638349,0.765669813902728,12.5582434482152));
#25297=CARTESIAN_POINT('Ctrl Pts',(4.83939633156508,0.885553144829605,12.5650698065815));
#25298=CARTESIAN_POINT('Ctrl Pts',(4.80056665704078,1.0716533508382,12.5757930195174));
#25299=CARTESIAN_POINT('Ctrl Pts',(4.78516580992274,1.13845033494815,12.579667514265));
#25300=CARTESIAN_POINT('Ctrl Pts',(4.74913887420359,1.28102603885606,12.5880012263426));
#25301=CARTESIAN_POINT('Ctrl Pts',(4.72808371928204,1.35667678428075,12.5924623440499));
#25302=CARTESIAN_POINT('Ctrl Pts',(4.67880155679679,1.51863048567403,12.6021052957347));
#25303=CARTESIAN_POINT('Ctrl Pts',(4.64997746309202,1.60472175947004,12.6072891803258));
#25304=CARTESIAN_POINT('Ctrl Pts',(4.56291679509271,1.84266435625749,12.6217816929282));
#25305=CARTESIAN_POINT('Ctrl Pts',(4.49950766187454,1.99249912002729,12.6311021350282));
#25306=CARTESIAN_POINT('Ctrl Pts',(4.40634243916989,2.18540487858849,12.6433181384147));
#25307=CARTESIAN_POINT('Ctrl Pts',(4.38316042141994,2.23153601414809,12.6462560302448));
#25308=CARTESIAN_POINT('Ctrl Pts',(4.34352775000413,2.30740192031852,12.6511118941388));
#25309=CARTESIAN_POINT('Ctrl Pts',(4.32748778296205,2.33734602638833,12.6530345667343));
#25310=CARTESIAN_POINT('Ctrl Pts',(4.27799082788966,2.42749273023385,12.658843973673));
#25311=CARTESIAN_POINT('Ctrl Pts',(4.24357818988832,2.48716119392316,12.662718888001));
#25312=CARTESIAN_POINT('Ctrl Pts',(4.14766747263507,2.64567299747709,12.6731229881941));
#25313=CARTESIAN_POINT('Ctrl Pts',(4.08389500509627,2.74308820063897,12.6796360760718));
#25314=CARTESIAN_POINT('Ctrl Pts',(3.93687223313482,2.95116402587236,12.6939122493554));
#25315=CARTESIAN_POINT('Ctrl Pts',(3.85228473071804,3.0607570562648,12.7016733521907));
#25316=CARTESIAN_POINT('Ctrl Pts',(3.72224628283575,3.21529306839571,12.7130592062826));
#25317=CARTESIAN_POINT('Ctrl Pts',(3.68036327687757,3.26315076974412,12.7166511056339));
#25318=CARTESIAN_POINT('Ctrl Pts',(3.58846248043213,3.36414068772975,12.7243818166378));
#25319=CARTESIAN_POINT('Ctrl Pts',(3.53816648341238,3.41699916703725,12.728522350703));
#25320=CARTESIAN_POINT('Ctrl Pts',(3.38202900490992,3.57394665016725,12.7411181529036));
#25321=CARTESIAN_POINT('Ctrl Pts',(3.27263545404829,3.67438036903596,12.7496012959984));
#25322=CARTESIAN_POINT('Ctrl Pts',(3.04598311810229,3.86430604889635,12.7665280438839));
#25323=CARTESIAN_POINT('Ctrl Pts',(2.92890403246031,3.95378252491936,12.7749628617417));
#25324=CARTESIAN_POINT('Ctrl Pts',(2.77408223819932,4.06144754020602,12.7856947703326));
#25325=CARTESIAN_POINT('Ctrl Pts',(2.739882781973,4.08459677178946,12.7880401164099));
#25326=CARTESIAN_POINT('Ctrl Pts',(2.66905220012077,4.13125130064764,12.7928438028343));
#25327=CARTESIAN_POINT('Ctrl Pts',(2.63239242779999,4.15470662287336,12.7953013765048));
#25328=CARTESIAN_POINT('Ctrl Pts',(2.57197110734827,4.19224404633857,12.7993101648414));
#25329=CARTESIAN_POINT('Ctrl Pts',(2.54839391139228,4.20661788194225,12.8008642589004));
#25330=CARTESIAN_POINT('Ctrl Pts',(2.48814434605346,4.24265658527528,12.8048116434279));
#25331=CARTESIAN_POINT('Ctrl Pts',(2.45130923539939,4.26404505693337,12.8072026656876));
#25332=CARTESIAN_POINT('Ctrl Pts',(2.24530989914214,4.38010790126974,12.8204650456799));
#25333=CARTESIAN_POINT('Ctrl Pts',(2.07094160404649,4.46519454328312,12.8312931153747));
#25334=CARTESIAN_POINT('Ctrl Pts',(1.81733743792339,4.57088742324357,12.8467472920114));
#25335=CARTESIAN_POINT('Ctrl Pts',(1.74191113233369,4.60016006188954,12.8513073076284));
#25336=CARTESIAN_POINT('Ctrl Pts',(1.60112772581875,4.65083833598275,12.8597669537097));
#25337=CARTESIAN_POINT('Ctrl Pts',(1.53597723902097,4.67275946311942,12.863661813852));
#25338=CARTESIAN_POINT('Ctrl Pts',(1.36276118265149,4.72702716528049,12.8739730987878));
#25339=CARTESIAN_POINT('Ctrl Pts',(1.25400621760271,4.75703392323669,12.8804031565053));
#25340=CARTESIAN_POINT('Ctrl Pts',(0.95166791222481,4.82936322028765,12.8981719767938));
#25341=CARTESIAN_POINT('Ctrl Pts',(0.756409996755351,4.86377068043257,12.9095349950983));
#25342=CARTESIAN_POINT('Ctrl Pts',(0.514959687059944,4.89142304227158,12.9233773513371));
#25343=CARTESIAN_POINT('Ctrl Pts',(0.470241067282416,4.89592445407627,12.9259319539752));
#25344=CARTESIAN_POINT('Ctrl Pts',(0.386790045311462,4.90317077886525,12.9306795818137));
#25345=CARTESIAN_POINT('Ctrl Pts',(0.348074948250218,4.9060711458306,12.9328740395691));
#25346=CARTESIAN_POINT('Ctrl Pts',(0.262941891064752,4.91143613949402,12.9376862305218));
#25347=CARTESIAN_POINT('Ctrl Pts',(0.216515177281609,4.91370172298623,12.9403018732373));
#25348=CARTESIAN_POINT('Ctrl Pts',(0.0737877311793425,4.9186399002408,12.9483268148581));
#25349=CARTESIAN_POINT('Ctrl Pts',(-0.0225651832630477,4.91914160196261,
12.9537220050758));
#25350=CARTESIAN_POINT('Ctrl Pts',(-0.275919939155246,4.91301638971006,
12.9679192321155));
#25351=CARTESIAN_POINT('Ctrl Pts',(-0.432695325324775,4.90169724137416,
12.9767176553217));
#25352=CARTESIAN_POINT('Ctrl Pts',(-0.661138657531286,4.87415720550904,
12.989679896139));
#25353=CARTESIAN_POINT('Ctrl Pts',(-0.733414702123794,4.86380668811291,
12.9938013922589));
#25354=CARTESIAN_POINT('Ctrl Pts',(-0.863827360069615,4.84215749735272,
13.001284827541));
#25355=CARTESIAN_POINT('Ctrl Pts',(-0.922041595448284,4.83141036784889,
13.004642311391));
#25356=CARTESIAN_POINT('Ctrl Pts',(-0.994035189030095,4.81677079152845,
13.0088179688936));
#25357=CARTESIAN_POINT('Ctrl Pts',(-1.00801064715348,4.81386553085616,13.009629649949));
#25358=CARTESIAN_POINT('Ctrl Pts',(-1.0362006670346,4.80787716089409,13.0112691563902));
#25359=CARTESIAN_POINT('Ctrl Pts',(-1.05041459765812,4.80479175286518,13.0120969879372));
#25360=CARTESIAN_POINT('Ctrl Pts',(-1.14907691917501,4.78291646109989,13.0178513599189));
#25361=CARTESIAN_POINT('Ctrl Pts',(-1.23302979291403,4.7619644015857,13.0227899080874));
#25362=CARTESIAN_POINT('Ctrl Pts',(-1.4757361078947,4.69454342987918,13.0371934807508));
#25363=CARTESIAN_POINT('Ctrl Pts',(-1.63275248939524,4.64226825653443,13.0466744900902));
#25364=CARTESIAN_POINT('Ctrl Pts',(-1.83826272680442,4.56212889000835,13.0592602045832));
#25365=CARTESIAN_POINT('Ctrl Pts',(-1.88934804300358,4.54121062445764,13.0624033369308));
#25366=CARTESIAN_POINT('Ctrl Pts',(-1.95708127069116,4.51213459900771,13.0665871252505));
#25367=CARTESIAN_POINT('Ctrl Pts',(-1.97405045573635,4.50473645677946,13.067636662298));
#25368=CARTESIAN_POINT('Ctrl Pts',(-2.02417614545175,4.48254527616926,13.0707407622591));
#25369=CARTESIAN_POINT('Ctrl Pts',(-2.05721118955374,4.46748065218478,13.0727916730823));
#25370=CARTESIAN_POINT('Ctrl Pts',(-2.13477061799304,4.43106931551151,13.0776230553163));
#25371=CARTESIAN_POINT('Ctrl Pts',(-2.17914642094442,4.40941513214496,13.0804001698281));
#25372=CARTESIAN_POINT('Ctrl Pts',(-2.32158540530958,4.33723327304474,13.089368980715));
#25373=CARTESIAN_POINT('Ctrl Pts',(-2.41827694264989,4.28407377385376,13.0955429661045));
#25374=CARTESIAN_POINT('Ctrl Pts',(-2.63787070061991,4.15353946241633,13.1098557616424));
#25375=CARTESIAN_POINT('Ctrl Pts',(-2.75929616954299,4.07388460897361,13.1179932892749));
#25376=CARTESIAN_POINT('Ctrl Pts',(-2.93357466086628,3.94818756273855,13.1301052844369));
#25377=CARTESIAN_POINT('Ctrl Pts',(-2.98925522652132,3.90619999069877,13.1340440641749));
#25378=CARTESIAN_POINT('Ctrl Pts',(-3.079801238083,3.83485100305548,13.1405725543417));
#25379=CARTESIAN_POINT('Ctrl Pts',(-3.11518510151981,3.80616337320029,13.1431561186991));
#25380=CARTESIAN_POINT('Ctrl Pts',(-3.23755328563427,3.70410322917328,13.152208230679));
#25381=CARTESIAN_POINT('Ctrl Pts',(-3.3223845942299,3.6282078337653,13.1586962174754));
#25382=CARTESIAN_POINT('Ctrl Pts',(-3.52503218067891,3.43383489916485,13.1747472077926));
#25383=CARTESIAN_POINT('Ctrl Pts',(-3.63959159421848,3.31216651960875,13.1843213862007));
#25384=CARTESIAN_POINT('Ctrl Pts',(-3.78664593755876,3.13912492772573,13.1972846986788));
#25385=CARTESIAN_POINT('Ctrl Pts',(-3.82471060550807,3.09263345338399,13.2007076122421));
#25386=CARTESIAN_POINT('Ctrl Pts',(-3.86712709144033,3.03884550323575,13.2045968708277));
#25387=CARTESIAN_POINT('Ctrl Pts',(-3.87232299249328,3.03222172279014,13.2050746144678));
#25388=CARTESIAN_POINT('Ctrl Pts',(-3.88189708795891,3.01995183855786,13.2059573474881));
#25389=CARTESIAN_POINT('Ctrl Pts',(-3.8862800337432,3.01430947454687,13.2063624059064));
#25390=CARTESIAN_POINT('Ctrl Pts',(-3.89514852216803,3.00284117359959,13.2071839253731));
#25391=CARTESIAN_POINT('Ctrl Pts',(-3.89963331719153,2.99701470054644,13.2076003700913));
#25392=CARTESIAN_POINT('Ctrl Pts',(-3.91471447636118,2.97733067435723,13.2090041848999));
#25393=CARTESIAN_POINT('Ctrl Pts',(-3.9252501981295,2.96342677691314,13.2099906304472));
#25394=CARTESIAN_POINT('Ctrl Pts',(-3.97258539452435,2.90026360731435,13.2144495680702));
#25395=CARTESIAN_POINT('Ctrl Pts',(-4.00853342260501,2.85037254419387,13.2179105772898));
#25396=CARTESIAN_POINT('Ctrl Pts',(-4.10085440886187,2.71704137224539,13.2270220051929));
#25397=CARTESIAN_POINT('Ctrl Pts',(-4.15561681082883,2.63252157093875,13.2326597597566));
#25398=CARTESIAN_POINT('Ctrl Pts',(-4.29131487191327,2.40828834848544,13.2473426957897));
#25399=CARTESIAN_POINT('Ctrl Pts',(-4.36803373687612,2.26616779017128,13.256385706574));
#25400=CARTESIAN_POINT('Ctrl Pts',(-4.46755004179216,2.05791080258784,13.2693972741878));
#25401=CARTESIAN_POINT('Ctrl Pts',(-4.496145655261,1.99466146271686,13.2733181836867));
#25402=CARTESIAN_POINT('Ctrl Pts',(-4.54745197937491,1.87446505715379,13.2807200633776));
#25403=CARTESIAN_POINT('Ctrl Pts',(-4.57045526740873,1.81765709190626,13.2841981554568));
#25404=CARTESIAN_POINT('Ctrl Pts',(-4.65355990534784,1.60086460416551,13.2974025853318));
#25405=CARTESIAN_POINT('Ctrl Pts',(-4.70636995203586,1.43821686912942,13.3071734417914));
#25406=CARTESIAN_POINT('Ctrl Pts',(-4.75517464728987,1.2561084876741,13.3179663082455));
#25407=CARTESIAN_POINT('Ctrl Pts',(-4.75965068753344,1.23903984464184,13.3189764473691));
#25408=CARTESIAN_POINT('Ctrl Pts',(-4.76403458795361,1.2219482424725,13.3199864568809));
#25409=CARTESIAN_POINT('Origin',(0.,0.,-3.23514056400928));
#25410=CARTESIAN_POINT('',(-4.76403458688904,1.22194824662298,15.4150234826428));
#25411=CARTESIAN_POINT('',(-4.76403458707897,1.2219482458825,15.0697260295707));
#25412=CARTESIAN_POINT('',(-4.76403458704967,1.22194824599672,-3.23514056400928));
#25413=CARTESIAN_POINT('Ctrl Pts',(-4.76403458688904,1.22194824662298,15.4150234826428));
#25414=CARTESIAN_POINT('Ctrl Pts',(-4.75134449250892,1.27142337677261,15.4121081981807));
#25415=CARTESIAN_POINT('Ctrl Pts',(-4.73788412615466,1.32069912133302,15.4091978920613));
#25416=CARTESIAN_POINT('Ctrl Pts',(-4.71333760987541,1.40534867036559,15.4041898595337));
#25417=CARTESIAN_POINT('Ctrl Pts',(-4.70261496733127,1.44082227632375,15.4020887840589));
#25418=CARTESIAN_POINT('Ctrl Pts',(-4.67604786342768,1.52525646341863,15.3970824162182));
#25419=CARTESIAN_POINT('Ctrl Pts',(-4.65983392678187,1.57409617343573,15.3941813954399));
#25420=CARTESIAN_POINT('Ctrl Pts',(-4.58916078114956,1.77630900694187,15.3821289778244));
#25421=CARTESIAN_POINT('Ctrl Pts',(-4.52787191167994,1.92718631601876,15.373033575167));
#25422=CARTESIAN_POINT('Ctrl Pts',(-4.42133328548739,2.15616773840472,15.3588763536351));
#25423=CARTESIAN_POINT('Ctrl Pts',(-4.38122830216776,2.23653430829834,15.3538373511134));
#25424=CARTESIAN_POINT('Ctrl Pts',(-4.3087138104182,2.3724019380417,15.3451709440757));
#25425=CARTESIAN_POINT('Ctrl Pts',(-4.27737562109464,2.42844875297089,15.3415514531651));
#25426=CARTESIAN_POINT('Ctrl Pts',(-4.22654342092121,2.51532145543982,15.3358643859259));
#25427=CARTESIAN_POINT('Ctrl Pts',(-4.20778850548242,2.54657165322187,15.3338026587189));
#25428=CARTESIAN_POINT('Ctrl Pts',(-4.15588271862014,2.63091999060186,15.3281926142887));
#25429=CARTESIAN_POINT('Ctrl Pts',(-4.12206287757725,2.68359808744987,15.3246395381905));
#25430=CARTESIAN_POINT('Ctrl Pts',(-3.97715955366056,2.90009619811801,15.3098204784923));
#25431=CARTESIAN_POINT('Ctrl Pts',(-3.85724497471954,3.05777948854271,15.2984922811165));
#25432=CARTESIAN_POINT('Ctrl Pts',(-3.67460024539284,3.27005186364464,15.2824660862827));
#25433=CARTESIAN_POINT('Ctrl Pts',(-3.61949106206961,3.33094742861924,15.2777706203196));
#25434=CARTESIAN_POINT('Ctrl Pts',(-3.52951770356506,3.42549710679179,15.2703306319995));
#25435=CARTESIAN_POINT('Ctrl Pts',(-3.49563657051375,3.46006512791778,15.2675771154922));
#25436=CARTESIAN_POINT('Ctrl Pts',(-3.45915328737675,3.49620512999272,15.2646642483703));
#25437=CARTESIAN_POINT('Ctrl Pts',(-3.45705422393186,3.49828070191186,15.2644968369092));
#25438=CARTESIAN_POINT('Ctrl Pts',(-3.45148020888507,3.50378241960159,15.26405275832));
#25439=CARTESIAN_POINT('Ctrl Pts',(-3.44800202238222,3.50720528768666,15.2637761458504));
#25440=CARTESIAN_POINT('Ctrl Pts',(-3.41547338250635,3.53912142066376,15.2611938274844));
#25441=CARTESIAN_POINT('Ctrl Pts',(-3.3860752804669,3.56725848424321,15.2588944710153));
#25442=CARTESIAN_POINT('Ctrl Pts',(-3.28155310678575,3.66484077526313,15.250830570676));
#25443=CARTESIAN_POINT('Ctrl Pts',(-3.20461420031283,3.73230450963938,15.2450920018536));
#25444=CARTESIAN_POINT('Ctrl Pts',(-3.02202957411019,3.88259243773808,15.2318382194647));
#25445=CARTESIAN_POINT('Ctrl Pts',(-2.91498660155145,3.96358924898163,15.2243313616186));
#25446=CARTESIAN_POINT('Ctrl Pts',(-2.74498599449902,4.0816088740256,15.2127103994135));
#25447=CARTESIAN_POINT('Ctrl Pts',(-2.68429230960297,4.12177798693677,15.2086175984317));
#25448=CARTESIAN_POINT('Ctrl Pts',(-2.56843920373896,4.1948089200395,15.2008962711094));
#25449=CARTESIAN_POINT('Ctrl Pts',(-2.5134840488733,4.22796637189551,15.1972707782827));
#25450=CARTESIAN_POINT('Ctrl Pts',(-2.40222710354667,4.292157812925,15.1899974741594));
#25451=CARTESIAN_POINT('Ctrl Pts',(-2.34593419841334,4.32318243535292,15.1863503382714));
#25452=CARTESIAN_POINT('Ctrl Pts',(-2.10367866822939,4.45057111597126,15.1707841804805));
#25453=CARTESIAN_POINT('Ctrl Pts',(-1.91227227415226,4.53610623313886,15.1587938603834));
#25454=CARTESIAN_POINT('Ctrl Pts',(-1.65089821233089,4.63341601767566,15.1428352615917));
#25455=CARTESIAN_POINT('Ctrl Pts',(-1.58528889334641,4.65627191318991,15.1388639140763));
#25456=CARTESIAN_POINT('Ctrl Pts',(-1.50908177424914,4.68102219849805,15.1342948655925));
#25457=CARTESIAN_POINT('Ctrl Pts',(-1.49893569650502,4.68428099099336,15.1336874407614));
#25458=CARTESIAN_POINT('Ctrl Pts',(-1.48219143695011,4.68959906405419,15.1326864892855));
#25459=CARTESIAN_POINT('Ctrl Pts',(-1.47559937041334,4.69167745434099,15.132292804156));
#25460=CARTESIAN_POINT('Ctrl Pts',(-1.46460517174817,4.69511831460446,15.1316368607983));
#25461=CARTESIAN_POINT('Ctrl Pts',(-1.46020547023611,4.69648850546849,15.1313745338387));
#25462=CARTESIAN_POINT('Ctrl Pts',(-1.45277328326636,4.69879164426458,15.1309316896031));
#25463=CARTESIAN_POINT('Ctrl Pts',(-1.44974181049916,4.69972784442821,15.1307511420472));
#25464=CARTESIAN_POINT('Ctrl Pts',(-1.4118654054906,4.71138496054417,15.1284963361687));
#25465=CARTESIAN_POINT('Ctrl Pts',(-1.37690297716942,4.72172112657146,15.1264258325769));
#25466=CARTESIAN_POINT('Ctrl Pts',(-1.30754614861273,4.74138966315003,15.1223413459808));
#25467=CARTESIAN_POINT('Ctrl Pts',(-1.27315880040227,4.7507388445087,15.1203273214971));
#25468=CARTESIAN_POINT('Ctrl Pts',(-1.16096478362739,4.77993632938074,15.1137869526605));
#25469=CARTESIAN_POINT('Ctrl Pts',(-1.08277254747144,4.79825326460896,15.1092763339742));
#25470=CARTESIAN_POINT('Ctrl Pts',(-0.856563816594028,4.84543245616913,
15.0963147135238));
#25471=CARTESIAN_POINT('Ctrl Pts',(-0.707623868615375,4.86941328336244,
15.0878852022365));
#25472=CARTESIAN_POINT('Ctrl Pts',(-0.510448090398453,4.89192180765791,
15.0767457586803));
#25473=CARTESIAN_POINT('Ctrl Pts',(-0.463002097236165,4.89664020013576,
15.0740670574182));
#25474=CARTESIAN_POINT('Ctrl Pts',(-0.351138624602694,4.90612436334394,
15.0677506799311));
#25475=CARTESIAN_POINT('Ctrl Pts',(-0.286681255865129,4.91031244961213,
15.0641104202797));
#25476=CARTESIAN_POINT('Ctrl Pts',(-0.1889158644417,4.91473308812075,15.0585817495178));
#25477=CARTESIAN_POINT('Ctrl Pts',(-0.155656902375431,4.91589884394543,
15.0566996799156));
#25478=CARTESIAN_POINT('Ctrl Pts',(-0.0497141779749854,4.91853600533687,
15.0506991299016));
#25479=CARTESIAN_POINT('Ctrl Pts',(0.0229910128247335,4.91873349373449,
15.0465728768188));
#25480=CARTESIAN_POINT('Ctrl Pts',(0.309195103284661,4.91316499759241,15.0302849580215));
#25481=CARTESIAN_POINT('Ctrl Pts',(0.522217801307229,4.8951075966827,15.0180524220398));
#25482=CARTESIAN_POINT('Ctrl Pts',(0.796076162255547,4.85380933256637,15.0022104074079));
#25483=CARTESIAN_POINT('Ctrl Pts',(0.858576484478969,4.8431445161373,14.9985879502636));
#25484=CARTESIAN_POINT('Ctrl Pts',(0.925706404782001,4.83034937881088,14.994692816851));
#25485=CARTESIAN_POINT('Ctrl Pts',(0.93055796281134,4.82941708150651,14.9944112869345));
#25486=CARTESIAN_POINT('Ctrl Pts',(0.939231455464921,4.82773678882183,14.9939079348186));
#25487=CARTESIAN_POINT('Ctrl Pts',(0.943053920851509,4.82699156115675,14.9936860903007));
#25488=CARTESIAN_POINT('Ctrl Pts',(0.949913265567177,4.8256458048252,14.9932879708419));
#25489=CARTESIAN_POINT('Ctrl Pts',(0.952950469987507,4.8250469476986,14.993111681854));
#25490=CARTESIAN_POINT('Ctrl Pts',(0.958421962559012,4.82396274503491,14.9927940849062));
#25491=CARTESIAN_POINT('Ctrl Pts',(0.960856452080789,4.82347842353463,14.9926527680618));
#25492=CARTESIAN_POINT('Ctrl Pts',(0.965259253631101,4.82259905715617,14.9923971862347));
#25493=CARTESIAN_POINT('Ctrl Pts',(0.967227693368259,4.82220464953539,14.9922829155089));
#25494=CARTESIAN_POINT('Ctrl Pts',(1.00836722016818,4.81393549991612,14.9898946439239));
#25495=CARTESIAN_POINT('Ctrl Pts',(1.04744144416762,4.80558486720289,14.9876250519173));
#25496=CARTESIAN_POINT('Ctrl Pts',(1.12691124076052,4.78758588715078,14.983008701684));
#25497=CARTESIAN_POINT('Ctrl Pts',(1.16729513719841,4.77790013336824,14.9806626573088));
#25498=CARTESIAN_POINT('Ctrl Pts',(1.35837900780964,4.72950290273426,14.9695490535891));
#25499=CARTESIAN_POINT('Ctrl Pts',(1.50731022357342,4.68416569096008,14.9608463206792));
#25500=CARTESIAN_POINT('Ctrl Pts',(1.78653577408412,4.58446563994996,14.9442349258733));
#25501=CARTESIAN_POINT('Ctrl Pts',(1.91713019414159,4.53140667394269,14.9363368902122));
#25502=CARTESIAN_POINT('Ctrl Pts',(2.11059342679835,4.44294255977192,14.9243510297896));
#25503=CARTESIAN_POINT('Ctrl Pts',(2.17525886145283,4.41164277019152,14.9202950287322));
#25504=CARTESIAN_POINT('Ctrl Pts',(2.29550857448917,4.35015184351033,14.9126487942917));
#25505=CARTESIAN_POINT('Ctrl Pts',(2.3512413932859,4.32028291636005,14.9090617196259));
#25506=CARTESIAN_POINT('Ctrl Pts',(2.51455424576044,4.22866218964797,14.8984147557209));
#25507=CARTESIAN_POINT('Ctrl Pts',(2.62039053303689,4.16390679449838,14.8913354672254));
#25508=CARTESIAN_POINT('Ctrl Pts',(2.85075928074599,4.01069230160558,14.8755090150239));
#25509=CARTESIAN_POINT('Ctrl Pts',(2.97385038876209,3.92029276335414,14.8667612607164));
#25510=CARTESIAN_POINT('Ctrl Pts',(3.13500080183473,3.78997825287945,14.8549379330655));
#25511=CARTESIAN_POINT('Ctrl Pts',(3.17688886294378,3.75493574335113,14.8518287712587));
#25512=CARTESIAN_POINT('Ctrl Pts',(3.24614017156926,3.69501335112484,14.8466315121843));
#25513=CARTESIAN_POINT('Ctrl Pts',(3.27382169608558,3.67050966655902,14.8445386299097));
#25514=CARTESIAN_POINT('Ctrl Pts',(3.35158639971549,3.60009272357943,14.83861234241));
#25515=CARTESIAN_POINT('Ctrl Pts',(3.40099823848978,3.55345045945065,14.8347895704619));
#25516=CARTESIAN_POINT('Ctrl Pts',(3.56882243750937,3.38832475601191,14.8215671907573));
#25517=CARTESIAN_POINT('Ctrl Pts',(3.68213777208877,3.26482771307609,14.8122090675872));
#25518=CARTESIAN_POINT('Ctrl Pts',(3.83864222729527,3.07572558306742,14.7984351931569));
#25519=CARTESIAN_POINT('Ctrl Pts',(3.88691737220398,3.01448755211031,14.7940540133454));
#25520=CARTESIAN_POINT('Ctrl Pts',(3.97700759073066,2.8944421789207,14.7855980934248));
#25521=CARTESIAN_POINT('Ctrl Pts',(4.01902464973138,2.83581127907917,14.7815260493546));
#25522=CARTESIAN_POINT('Ctrl Pts',(4.09531859930095,2.72424703808877,14.7738748249614));
#25523=CARTESIAN_POINT('Ctrl Pts',(4.12989655562918,2.67153713894641,14.7702989384917));
#25524=CARTESIAN_POINT('Ctrl Pts',(4.2323031903402,2.50868910725879,14.7593620572437));
#25525=CARTESIAN_POINT('Ctrl Pts',(4.29680831724125,2.39652851182006,14.7519791613104));
#25526=CARTESIAN_POINT('Ctrl Pts',(4.42099862334972,2.15941873270447,14.7366660212109));
#25527=CARTESIAN_POINT('Ctrl Pts',(4.47998218011592,2.0342266189149,14.7287399443678));
#25528=CARTESIAN_POINT('Ctrl Pts',(4.55704840546019,1.85098567951177,14.7173914644622));
#25529=CARTESIAN_POINT('Ctrl Pts',(4.57945725407452,1.79482855427854,14.713946849728));
#25530=CARTESIAN_POINT('Ctrl Pts',(4.61381313348214,1.70389607406004,14.7084273408619));
#25531=CARTESIAN_POINT('Ctrl Pts',(4.62641535144787,1.66937548146195,14.7063456002465));
#25532=CARTESIAN_POINT('Ctrl Pts',(4.65864474379314,1.57792217908994,14.7008651257434));
#25533=CARTESIAN_POINT('Ctrl Pts',(4.67761524571174,1.52076460861603,14.697473964864));
#25534=CARTESIAN_POINT('Ctrl Pts',(4.74513746817459,1.30409089039796,14.6847183390208));
#25535=CARTESIAN_POINT('Ctrl Pts',(4.78661698991098,1.14248893977293,14.6754028564007));
#25536=CARTESIAN_POINT('Ctrl Pts',(4.83054896227543,0.926223646075818,14.6630254441948));
#25537=CARTESIAN_POINT('Ctrl Pts',(4.84041804934139,0.873181873656372,14.6599970701756));
#25538=CARTESIAN_POINT('Ctrl Pts',(4.85603198938666,0.78084104448554,14.6547320573465));
#25539=CARTESIAN_POINT('Ctrl Pts',(4.86217717232046,0.741614819769123,14.6524977115511));
#25540=CARTESIAN_POINT('Ctrl Pts',(4.87805758351715,0.631545966343782,14.6462313082988));
#25541=CARTESIAN_POINT('Ctrl Pts',(4.88672373667603,0.560559597487248,14.6421934984164));
#25542=CARTESIAN_POINT('Ctrl Pts',(4.90015435359788,0.426260617300041,14.6345518132589));
#25543=CARTESIAN_POINT('Ctrl Pts',(4.90524669378877,0.362995268065324,14.6309509389889));
#25544=CARTESIAN_POINT('Ctrl Pts',(4.91991983002028,0.122607504312978,14.6172565010753));
#25545=CARTESIAN_POINT('Ctrl Pts',(4.92114108316411,-0.054887424198698,
14.607114536424));
#25546=CARTESIAN_POINT('Ctrl Pts',(4.90699938991099,-0.354274608169366,
14.5899570621734));
#25547=CARTESIAN_POINT('Ctrl Pts',(4.89666765233485,-0.476235119059623,
14.582954921352));
#25548=CARTESIAN_POINT('Ctrl Pts',(4.87658845447658,-0.640239170016415,
14.5735475710963));
#25549=CARTESIAN_POINT('Ctrl Pts',(4.87082212334513,-0.682724723852563,
14.5711115024601));
#25550=CARTESIAN_POINT('Ctrl Pts',(4.85846037196939,-0.765652988007717,
14.5663607394535));
#25551=CARTESIAN_POINT('Ctrl Pts',(4.85191358511333,-0.8060994299673,14.5640457722358));
#25552=CARTESIAN_POINT('Ctrl Pts',(4.82423595635871,-0.964517263815048,
14.5549774387385));
#25553=CARTESIAN_POINT('Ctrl Pts',(4.79930125580401,-1.08178287533086,14.5482612072467));
#25554=CARTESIAN_POINT('Ctrl Pts',(4.74764075214014,-1.28747716029942,14.5363786954475));
#25555=CARTESIAN_POINT('Ctrl Pts',(4.72266188258935,-1.37628297699634,14.5312144532447));
#25556=CARTESIAN_POINT('Ctrl Pts',(4.67130997176311,-1.54093639258833,14.521538699467));
#25557=CARTESIAN_POINT('Ctrl Pts',(4.64554825003911,-1.6169425208653,14.5170311507592));
#25558=CARTESIAN_POINT('Ctrl Pts',(4.59274637455384,-1.76102935970212,14.5083878893918));
#25559=CARTESIAN_POINT('Ctrl Pts',(4.56602224225133,-1.82920321063417,14.504255288613));
#25560=CARTESIAN_POINT('Ctrl Pts',(4.51047413519662,-1.96209623616906,14.4961033183088));
#25561=CARTESIAN_POINT('Ctrl Pts',(4.48175394993675,-2.02683989049321,14.4920856302962));
#25562=CARTESIAN_POINT('Ctrl Pts',(4.37145646462214,-2.26166503923959,14.4773314762783));
#25563=CARTESIAN_POINT('Ctrl Pts',(4.28151307638783,-2.42763349735151,14.4665411653619));
#25564=CARTESIAN_POINT('Ctrl Pts',(4.12428176406584,-2.68172032387355,14.4494377290776));
#25565=CARTESIAN_POINT('Ctrl Pts',(4.06316829635748,-2.77344330358308,14.4431350604432));
#25566=CARTESIAN_POINT('Ctrl Pts',(3.97431598593088,-2.89755021344921,14.4344456209673));
#25567=CARTESIAN_POINT('Ctrl Pts',(3.94916066269556,-2.93174264066341,14.4320339986259));
#25568=CARTESIAN_POINT('Ctrl Pts',(3.89864010064452,-2.9985825326546,14.4272870171358));
#25569=CARTESIAN_POINT('Ctrl Pts',(3.87329956719775,-3.03124435677622,14.4249515820252));
#25570=CARTESIAN_POINT('Ctrl Pts',(3.75878426363892,-3.17506398316356,14.4145859530099));
#25571=CARTESIAN_POINT('Ctrl Pts',(3.66521417449634,-3.28263558788164,14.4066096849645));
#25572=CARTESIAN_POINT('Ctrl Pts',(3.4597856322612,-3.49905217645652,14.3898932799596));
#25573=CARTESIAN_POINT('Ctrl Pts',(3.34715347526959,-3.6069440766278,14.3811604917817));
#25574=CARTESIAN_POINT('Ctrl Pts',(3.1756513158615,-3.75626630357179,14.3683470296151));
#25575=CARTESIAN_POINT('Ctrl Pts',(3.12069587316908,-3.80204615116858,14.3643085513225));
#25576=CARTESIAN_POINT('Ctrl Pts',(3.00816898366336,-3.89170121455556,14.3561625797643));
#25577=CARTESIAN_POINT('Ctrl Pts',(2.95058809868431,-3.93553664516097,14.3520558245999));
#25578=CARTESIAN_POINT('Ctrl Pts',(2.75733673926691,-4.07603006696622,14.3384623951906));
#25579=CARTESIAN_POINT('Ctrl Pts',(2.61772477701156,-4.16706644472577,14.3289375410327));
#25580=CARTESIAN_POINT('Ctrl Pts',(2.3621257258463,-4.31581157348355,14.3120085078497));
#25581=CARTESIAN_POINT('Ctrl Pts',(2.24796863116282,-4.3763575134295,14.3046159265916));
#25582=CARTESIAN_POINT('Ctrl Pts',(2.09462667935548,-4.45010131085714,14.2949326978781));
#25583=CARTESIAN_POINT('Ctrl Pts',(2.05747253308808,-4.46740074727395,14.2926051349198));
#25584=CARTESIAN_POINT('Ctrl Pts',(1.98102911978013,-4.50183780292758,14.2878563980824));
#25585=CARTESIAN_POINT('Ctrl Pts',(1.9417232822473,-4.51893026389814,14.285435889093));
#25586=CARTESIAN_POINT('Ctrl Pts',(1.79025517599162,-4.58245622716335,14.2761784011427));
#25587=CARTESIAN_POINT('Ctrl Pts',(1.67661061729344,-4.62524551824978,14.269377716539));
#25588=CARTESIAN_POINT('Ctrl Pts',(1.39821166820359,-4.71845723479997,14.2529295952357));
#25589=CARTESIAN_POINT('Ctrl Pts',(1.23216788117661,-4.7645142409005,14.2432907464544));
#25590=CARTESIAN_POINT('Ctrl Pts',(0.994022976208555,-4.81728620218662,
14.22954702831));
#25591=CARTESIAN_POINT('Ctrl Pts',(0.923662793841521,-4.83127052836926,
14.2254968781382));
#25592=CARTESIAN_POINT('Ctrl Pts',(0.790681066175808,-4.85468984663343,
14.217852242124));
#25593=CARTESIAN_POINT('Ctrl Pts',(0.728133919774229,-4.8644640958365,14.2142608648231));
#25594=CARTESIAN_POINT('Ctrl Pts',(0.509433634148416,-4.89432779897977,
14.2017104175261));
#25595=CARTESIAN_POINT('Ctrl Pts',(0.352520395140321,-4.90812545059303,
14.1927150911721));
#25596=CARTESIAN_POINT('Ctrl Pts',(0.0928914124104607,-4.91843893486339,
14.1778422065908));
#25597=CARTESIAN_POINT('Ctrl Pts',(-0.00953775875027473,-4.91930681469287,
14.1719782192377));
#25598=CARTESIAN_POINT('Ctrl Pts',(-0.176232658199517,-4.91551253107512,
14.1624557606317));
#25599=CARTESIAN_POINT('Ctrl Pts',(-0.24051152815045,-4.91278696288025,
14.1587889954078));
#25600=CARTESIAN_POINT('Ctrl Pts',(-0.341465524313964,-4.90652013900496,
14.153044064287));
#25601=CARTESIAN_POINT('Ctrl Pts',(-0.378185470144098,-4.9038265033064,
14.1509576793653));
#25602=CARTESIAN_POINT('Ctrl Pts',(-0.470245499078712,-4.89603312990407,
14.1457344427815));
#25603=CARTESIAN_POINT('Ctrl Pts',(-0.525535858177351,-4.89040728429077,
14.1426033702849));
#25604=CARTESIAN_POINT('Ctrl Pts',(-0.699771565341797,-4.86968958182358,
14.1327367000703));
#25605=CARTESIAN_POINT('Ctrl Pts',(-0.818267044930069,-4.85118503882439,
14.1260260387463));
#25606=CARTESIAN_POINT('Ctrl Pts',(-1.08092201190979,-4.80026996932733,
14.1110370925674));
#25607=CARTESIAN_POINT('Ctrl Pts',(-1.224535363853,-4.76565804401943,14.1027622716073));
#25608=CARTESIAN_POINT('Ctrl Pts',(-1.4350219756809,-4.70478500022798,14.0904155433134));
#25609=CARTESIAN_POINT('Ctrl Pts',(-1.50322999118492,-4.68343777668757,
14.0863801046689));
#25610=CARTESIAN_POINT('Ctrl Pts',(-1.63111898051464,-4.64033035671548,
14.0787389178572));
#25611=CARTESIAN_POINT('Ctrl Pts',(-1.6908910222866,-4.61888540529683,14.0751361497508));
#25612=CARTESIAN_POINT('Ctrl Pts',(-1.88919159463853,-4.5433741146259,14.0630703354164));
#25613=CARTESIAN_POINT('Ctrl Pts',(-2.02567973927464,-4.48418485568739,
14.0545760199992));
#25614=CARTESIAN_POINT('Ctrl Pts',(-2.25581450273617,-4.37173069560083,
14.039915868712));
#25615=CARTESIAN_POINT('Ctrl Pts',(-2.35078270411255,-4.32140592306065,
14.0337623156356));
#25616=CARTESIAN_POINT('Ctrl Pts',(-2.4718918946353,-4.25205416570508,14.0257908032886));
#25617=CARTESIAN_POINT('Ctrl Pts',(-2.49960051909974,-4.23582476344418,
14.0239583660017));
#25618=CARTESIAN_POINT('Ctrl Pts',(-2.56820626010293,-4.19473362262961,
14.0194007353132));
#25619=CARTESIAN_POINT('Ctrl Pts',(-2.60890341005437,-4.16954393542025,
14.0166786647914));
#25620=CARTESIAN_POINT('Ctrl Pts',(-2.68105442388414,-4.12341573176651,
14.0118224184637));
#25621=CARTESIAN_POINT('Ctrl Pts',(-2.71264653822793,-4.10270141552781,
14.0096857753031));
#25622=CARTESIAN_POINT('Ctrl Pts',(-2.80417192856449,-4.04117067190184,
14.0034607422161));
#25623=CARTESIAN_POINT('Ctrl Pts',(-2.86344521181984,-3.99939024292269,
13.9993843895584));
#25624=CARTESIAN_POINT('Ctrl Pts',(-3.07821041810672,-3.84078421340153,
13.9844000891049));
#25625=CARTESIAN_POINT('Ctrl Pts',(-3.22765704651937,-3.71607759864433,
13.9735408567487));
#25626=CARTESIAN_POINT('Ctrl Pts',(-3.39857898786815,-3.5553419469705,13.960351819487));
#25627=CARTESIAN_POINT('Ctrl Pts',(-3.42749312580402,-3.5274759171243,13.9580923181677));
#25628=CARTESIAN_POINT('Ctrl Pts',(-3.50722629172008,-3.44872701203439,
13.9517783021545));
#25629=CARTESIAN_POINT('Ctrl Pts',(-3.55727508185132,-3.39707934848813,
13.9477180397646));
#25630=CARTESIAN_POINT('Ctrl Pts',(-3.64913066212785,-3.29803266101072,
13.9400705646552));
#25631=CARTESIAN_POINT('Ctrl Pts',(-3.69119151542172,-3.250888972088,13.936486546888));
#25632=CARTESIAN_POINT('Ctrl Pts',(-3.88119892905612,-3.02947710740625,
13.9198979898087));
#25633=CARTESIAN_POINT('Ctrl Pts',(-4.01778910762865,-2.84583988030193,
13.9068045571363));
#25634=CARTESIAN_POINT('Ctrl Pts',(-4.18806747750911,-2.58008719510037,
13.8887524405794));
#25635=CARTESIAN_POINT('Ctrl Pts',(-4.23307218809573,-2.5055656573129,13.8837821235464));
#25636=CARTESIAN_POINT('Ctrl Pts',(-4.2949440057624,-2.39668469936246,13.8766619844641));
#25637=CARTESIAN_POINT('Ctrl Pts',(-4.31342491676308,-2.36326196377785,
13.8744951841325));
#25638=CARTESIAN_POINT('Ctrl Pts',(-4.3542885155946,-2.28728358244348,13.8696130843376));
#25639=CARTESIAN_POINT('Ctrl Pts',(-4.37644020850545,-2.2446081708195,13.8669006772187));
#25640=CARTESIAN_POINT('Ctrl Pts',(-4.48547124543402,-2.0268068973371,13.8531873992869));
#25641=CARTESIAN_POINT('Ctrl Pts',(-4.56248031474317,-1.84693614833202,
13.8422764251408));
#25642=CARTESIAN_POINT('Ctrl Pts',(-4.65571196738907,-1.58744080420424,
13.8268078632914));
#25643=CARTESIAN_POINT('Ctrl Pts',(-4.68099178131023,-1.51127033133288,
13.8223001719689));
#25644=CARTESIAN_POINT('Ctrl Pts',(-4.7257520109773,-1.36448223827827,13.8136566988981));
#25645=CARTESIAN_POINT('Ctrl Pts',(-4.74554076291879,-1.29398089287288,
13.8095240295042));
#25646=CARTESIAN_POINT('Ctrl Pts',(-4.78135935675284,-1.15447006748005,
13.8013720427921));
#25647=CARTESIAN_POINT('Ctrl Pts',(-4.79748684961141,-1.08550366564466,
13.7973544076187));
#25648=CARTESIAN_POINT('Ctrl Pts',(-4.85109117423788,-0.831668844096764,
13.7826005696829));
#25649=CARTESIAN_POINT('Ctrl Pts',(-4.87941431400663,-0.645037090594373,
13.771810524382));
#25650=CARTESIAN_POINT('Ctrl Pts',(-4.90719367347956,-0.34752809249043,
13.7547069432821));
#25651=CARTESIAN_POINT('Ctrl Pts',(-4.9137481104115,-0.237498272426668,
13.7484038677095));
#25652=CARTESIAN_POINT('Ctrl Pts',(-4.91770023727319,-0.0849072196384362,
13.7397139808591));
#25653=CARTESIAN_POINT('Ctrl Pts',(-4.91824988907269,-0.042461084205414,
13.7373023151503));
#25654=CARTESIAN_POINT('Ctrl Pts',(-4.91825010801743,0.0413238316877421,
13.7325553282673));
#25655=CARTESIAN_POINT('Ctrl Pts',(-4.91772907888801,0.0826591704296608,
13.7302199307599));
#25656=CARTESIAN_POINT('Ctrl Pts',(-4.91311046343467,0.265815186267638,
13.7198896887542));
#25657=CARTESIAN_POINT('Ctrl Pts',(-4.90339839974557,0.407427507211956,
13.7119482571227));
#25658=CARTESIAN_POINT('Ctrl Pts',(-4.87072741108792,0.698593346091473,
13.6955342622679));
#25659=CARTESIAN_POINT('Ctrl Pts',(-4.84696531171142,0.847906089698089,
13.68706901625));
#25660=CARTESIAN_POINT('Ctrl Pts',(-4.80162648412878,1.06717652952238,13.674456396872));
#25661=CARTESIAN_POINT('Ctrl Pts',(-4.78530484911705,1.13813003537015,13.670346976507));
#25662=CARTESIAN_POINT('Ctrl Pts',(-4.7662939684885,1.21311403254434,13.6659684627439));
#25663=CARTESIAN_POINT('Ctrl Pts',(-4.76516734420597,1.2175319425333,13.6657103575944));
#25664=CARTESIAN_POINT('Ctrl Pts',(-4.76403458702644,1.22194824608729,13.6654522135017));
#25665=CARTESIAN_POINT('',(-4.9182499639856,0.000107902101101913,13.389740414873));
#25666=CARTESIAN_POINT('Ctrl Pts',(-4.76403458795361,1.2219482424725,13.3199864568809));
#25667=CARTESIAN_POINT('Ctrl Pts',(-4.79152982453573,1.11475200164307,13.3263211013333));
#25668=CARTESIAN_POINT('Ctrl Pts',(-4.81540061011838,1.00665267818612,13.3326514556104));
#25669=CARTESIAN_POINT('Ctrl Pts',(-4.84333424286708,0.856206246615081,
13.3413619657047));
#25670=CARTESIAN_POINT('Ctrl Pts',(-4.8505256393311,0.814479467250247,13.3437672638303));
#25671=CARTESIAN_POINT('Ctrl Pts',(-4.86234930437609,0.740152742923929,
13.348030828943));
#25672=CARTESIAN_POINT('Ctrl Pts',(-4.86719468058729,0.707589435507746,
13.349891635032));
#25673=CARTESIAN_POINT('Ctrl Pts',(-4.87790924393894,0.630256336248681,
13.3542969718298));
#25674=CARTESIAN_POINT('Ctrl Pts',(-4.88348959718709,0.585449439817111,
13.3568385040052));
#25675=CARTESIAN_POINT('Ctrl Pts',(-4.90829832212776,0.361101322043394,
13.3695249524841));
#25676=CARTESIAN_POINT('Ctrl Pts',(-4.91824603641982,0.180673647320878,
13.3796082680788));
#25677=CARTESIAN_POINT('Ctrl Pts',(-4.9182499988158,0.000107927761981499,
13.3897403530557));
#25678=CARTESIAN_POINT('Ctrl Pts',(-4.91824999881644,0.000107898724551486,
13.3897403546851));
#25679=CARTESIAN_POINT('Ctrl Pts',(-4.91825167684014,-0.0763799386656473,
13.3940323170261));
#25680=CARTESIAN_POINT('Ctrl Pts',(-4.91646906583336,-0.15285694645591,
13.3983302366743));
#25681=CARTESIAN_POINT('Ctrl Pts',(-4.91001074095604,-0.291254482407087,
13.4061352017772));
#25682=CARTESIAN_POINT('Ctrl Pts',(-4.90594467761584,-0.35318744316204,
13.4096377748873));
#25683=CARTESIAN_POINT('Ctrl Pts',(-4.89494492677524,-0.483074502355274,
13.4170111961256));
#25684=CARTESIAN_POINT('Ctrl Pts',(-4.8877655020059,-0.550994617529353,
13.4208829302558));
#25685=CARTESIAN_POINT('Ctrl Pts',(-4.86450147179037,-0.734446094391615,
13.4313920786582));
#25686=CARTESIAN_POINT('Ctrl Pts',(-4.84571793790796,-0.849589751411313,
13.4380446593507));
#25687=CARTESIAN_POINT('Ctrl Pts',(-4.79065510034131,-1.12508000809426,
13.4541086330826));
#25688=CARTESIAN_POINT('Ctrl Pts',(-4.75039660083467,-1.28448963101816,
13.463527966129));
#25689=CARTESIAN_POINT('Ctrl Pts',(-4.68788270764438,-1.48840065142926,
13.4756982410256));
#25690=CARTESIAN_POINT('Ctrl Pts',(-4.67283171583888,-1.53499987073122,
13.4784875724753));
#25691=CARTESIAN_POINT('Ctrl Pts',(-4.65053790541573,-1.60065460487296,
13.482426666588));
#25692=CARTESIAN_POINT('Ctrl Pts',(-4.64386874711576,-1.61990155255968,
13.48358254593));
#25693=CARTESIAN_POINT('Ctrl Pts',(-4.62347926261925,-1.67758399694161,
13.4870496256959));
#25694=CARTESIAN_POINT('Ctrl Pts',(-4.60939991912805,-1.71589072615071,
13.4893558539465));
#25695=CARTESIAN_POINT('Ctrl Pts',(-4.5261082748265,-1.93408243881794,13.5025270970803));
#25696=CARTESIAN_POINT('Ctrl Pts',(-4.4468452647102,-2.10995259746291,13.5132880098638));
#25697=CARTESIAN_POINT('Ctrl Pts',(-4.31644468592308,-2.35909164841149,
13.5290526275224));
#25698=CARTESIAN_POINT('Ctrl Pts',(-4.27331709678737,-2.43634335335123,
13.5340171366736));
#25699=CARTESIAN_POINT('Ctrl Pts',(-4.18920906058899,-2.57788976488181,
13.5432837659071));
#25700=CARTESIAN_POINT('Ctrl Pts',(-4.1487717313446,-2.6424763260761,13.5475809455948));
#25701=CARTESIAN_POINT('Ctrl Pts',(-4.09953687364169,-2.71719656609823,
13.5526420140313));
#25702=CARTESIAN_POINT('Ctrl Pts',(-4.09217809235758,-2.72826652227305,
13.5533941747566));
#25703=CARTESIAN_POINT('Ctrl Pts',(-4.04436873689368,-2.79955844896837,
13.5582535958301));
#25704=CARTESIAN_POINT('Ctrl Pts',(-4.0026351141331,-2.85890852711016,13.5623704663148));
#25705=CARTESIAN_POINT('Ctrl Pts',(-3.84429597690079,-3.07381871272004,
13.5775565338341));
#25706=CARTESIAN_POINT('Ctrl Pts',(-3.71981129866037,-3.2233484383157,13.588682511825));
#25707=CARTESIAN_POINT('Ctrl Pts',(-3.53527975622997,-3.42003676189591,
13.6041182160004));
#25708=CARTESIAN_POINT('Ctrl Pts',(-3.48249813626058,-3.47376758806334,
13.6084251910664));
#25709=CARTESIAN_POINT('Ctrl Pts',(-3.41728831465045,-3.53716953412255,
13.6136134101297));
#25710=CARTESIAN_POINT('Ctrl Pts',(-3.40602131359527,-3.54802008899062,
13.6145051864753));
#25711=CARTESIAN_POINT('Ctrl Pts',(-3.38485597629069,-3.56820939165594,
13.6161716619043));
#25712=CARTESIAN_POINT('Ctrl Pts',(-3.37497027398729,-3.5775611656746,13.6169464986052));
#25713=CARTESIAN_POINT('Ctrl Pts',(-3.33637466750735,-3.61376987147128,
13.6199578093061));
#25714=CARTESIAN_POINT('Ctrl Pts',(-3.30738174804376,-3.64032342379345,
13.6221904160358));
#25715=CARTESIAN_POINT('Ctrl Pts',(-3.24587957686131,-3.69530969391984,
13.6268631931859));
#25716=CARTESIAN_POINT('Ctrl Pts',(-3.21330784644957,-3.7236676414984,13.6293020715046));
#25717=CARTESIAN_POINT('Ctrl Pts',(-3.08799235205111,-3.82990229979522,
13.6385614161177));
#25718=CARTESIAN_POINT('Ctrl Pts',(-2.99275635837726,-3.90477379187308,
13.6453458424578));
#25719=CARTESIAN_POINT('Ctrl Pts',(-2.79778048407332,-4.04673024076732,
13.6588575155489));
#25720=CARTESIAN_POINT('Ctrl Pts',(-2.69815245378672,-4.11382721956924,
13.6655802357866));
#25721=CARTESIAN_POINT('Ctrl Pts',(-2.53629175635438,-4.21442492263593,
13.67628661483));
#25722=CARTESIAN_POINT('Ctrl Pts',(-2.47562131498319,-4.25034731283924,
13.6802536849865));
#25723=CARTESIAN_POINT('Ctrl Pts',(-2.36077563782384,-4.31505291208773,
13.6876894879155));
#25724=CARTESIAN_POINT('Ctrl Pts',(-2.3067933150796,-4.34415098126529,13.6911551754821));
#25725=CARTESIAN_POINT('Ctrl Pts',(-2.20147004863784,-4.39840648330201,
13.6978662588447));
#25726=CARTESIAN_POINT('Ctrl Pts',(-2.15020660081262,-4.4236931923424,13.7011101170813));
#25727=CARTESIAN_POINT('Ctrl Pts',(-1.89814084748495,-4.54261271615078,
13.7169587793334));
#25728=CARTESIAN_POINT('Ctrl Pts',(-1.69161061391552,-4.62349651050588,
13.7296472781057));
#25729=CARTESIAN_POINT('Ctrl Pts',(-1.41878230508698,-4.70960786143244,
13.7460133686137));
#25730=CARTESIAN_POINT('Ctrl Pts',(-1.35685119317719,-4.72782237097062,
13.7497018956835));
#25731=CARTESIAN_POINT('Ctrl Pts',(-1.28983706931227,-4.74610656846844,
13.7536614541681));
#25732=CARTESIAN_POINT('Ctrl Pts',(-1.28509297043751,-4.74739331444389,
13.7539415908372));
#25733=CARTESIAN_POINT('Ctrl Pts',(-1.27739115853274,-4.7494698927789,13.7543960998104));
#25734=CARTESIAN_POINT('Ctrl Pts',(-1.27443462499064,-4.75026407907514,
13.7545705077718));
#25735=CARTESIAN_POINT('Ctrl Pts',(-1.26959724492533,-4.7515586586024,13.7548557584355));
#25736=CARTESIAN_POINT('Ctrl Pts',(-1.26771684027733,-4.75206069651287,
13.7549666150422));
#25737=CARTESIAN_POINT('Ctrl Pts',(-1.26134542427597,-4.75375771156918,
13.7553421407173));
#25738=CARTESIAN_POINT('Ctrl Pts',(-1.25685301481277,-4.7549474401786,13.7556067642878));
#25739=CARTESIAN_POINT('Ctrl Pts',(-1.24851063560456,-4.75714411084994,
13.7560978782762));
#25740=CARTESIAN_POINT('Ctrl Pts',(-1.24466111765875,-4.75815275089392,
13.7563243838259));
#25741=CARTESIAN_POINT('Ctrl Pts',(-1.23744085063474,-4.76003522352121,
13.7567490074312));
#25742=CARTESIAN_POINT('Ctrl Pts',(-1.23407038991793,-4.76091015045831,
13.7569471356054));
#25743=CARTESIAN_POINT('Ctrl Pts',(-1.22767839732198,-4.76256218319146,
13.7573227117195));
#25744=CARTESIAN_POINT('Ctrl Pts',(-1.22465704994484,-4.76333999479953,
13.7575001663877));
#25745=CARTESIAN_POINT('Ctrl Pts',(-1.2188560312492,-4.76482751711196,13.7578407431331));
#25746=CARTESIAN_POINT('Ctrl Pts',(-1.21607647457035,-4.76553767173865,
13.7580038695869));
#25747=CARTESIAN_POINT('Ctrl Pts',(-1.17810901508679,-4.77520267514886,
13.7602312663522));
#25748=CARTESIAN_POINT('Ctrl Pts',(-1.14282330999256,-4.78377010052902,
13.7622914801498));
#25749=CARTESIAN_POINT('Ctrl Pts',(-1.06132250591924,-4.80260539293934,
13.7670260945994));
#25750=CARTESIAN_POINT('Ctrl Pts',(-1.01504754666644,-4.81259831828243,
13.7696972571044));
#25751=CARTESIAN_POINT('Ctrl Pts',(-0.778096397923194,-4.86019743631449,
13.7833069896748));
#25752=CARTESIAN_POINT('Ctrl Pts',(-0.585454902308647,-4.88714610008783,
13.7941546640719));
#25753=CARTESIAN_POINT('Ctrl Pts',(-0.310146395291452,-4.90914347106024,
13.8096463835072));
#25754=CARTESIAN_POINT('Ctrl Pts',(-0.228419649536216,-4.91362439589162,
13.8142427851226));
#25755=CARTESIAN_POINT('Ctrl Pts',(-0.0791857700927101,-4.91807523946254,
13.8226508858267));
#25756=CARTESIAN_POINT('Ctrl Pts',(-0.0117180612027642,-4.91869871070011,
13.8264576754604));
#25757=CARTESIAN_POINT('Ctrl Pts',(0.124214317225545,-4.91715803250257,
13.8341474528072));
#25758=CARTESIAN_POINT('Ctrl Pts',(0.192663803526632,-4.91495196630278,
13.8380298875709));
#25759=CARTESIAN_POINT('Ctrl Pts',(0.266391232003425,-4.91103323587466,
13.8422259323727));
#25760=CARTESIAN_POINT('Ctrl Pts',(0.271737637686643,-4.91074030962273,
13.8425302921144));
#25761=CARTESIAN_POINT('Ctrl Pts',(0.407452139301232,-4.90308228582337,
13.8502582950425));
#25762=CARTESIAN_POINT('Ctrl Pts',(0.537474600852064,-4.89053713533766,
13.8577121558279));
#25763=CARTESIAN_POINT('Ctrl Pts',(0.787850148485951,-4.8562735094596,13.8721702823118));
#25764=CARTESIAN_POINT('Ctrl Pts',(0.908199539499136,-4.83521188070644,
13.8791672957652));
#25765=CARTESIAN_POINT('Ctrl Pts',(1.07806004082689,-4.79891944565424,13.8890920948371));
#25766=CARTESIAN_POINT('Ctrl Pts',(1.12830789870454,-4.78735445175538,13.8920340634327));
#25767=CARTESIAN_POINT('Ctrl Pts',(1.21961214443693,-4.76482258068863,13.8973876523161));
#25768=CARTESIAN_POINT('Ctrl Pts',(1.26072609942754,-4.75410956609177,13.8998012603206));
#25769=CARTESIAN_POINT('Ctrl Pts',(1.34240134477714,-4.73169350138373,13.9045994178986));
#25770=CARTESIAN_POINT('Ctrl Pts',(1.38296111953067,-4.71999823707557,13.9069838328906));
#25771=CARTESIAN_POINT('Ctrl Pts',(1.52760397872074,-4.67626646246126,13.9155025597058));
#25772=CARTESIAN_POINT('Ctrl Pts',(1.63076795574651,-4.64129704871887,13.9216078980534));
#25773=CARTESIAN_POINT('Ctrl Pts',(1.8831769820695,-4.54628243089763,13.9367201673611));
#25774=CARTESIAN_POINT('Ctrl Pts',(2.03079746610144,-4.48228743133347,13.9457161475407));
#25775=CARTESIAN_POINT('Ctrl Pts',(2.24679134505054,-4.37578744044238,13.9592639295677));
#25776=CARTESIAN_POINT('Ctrl Pts',(2.31769074753595,-4.33865145698193,13.9637754762328));
#25777=CARTESIAN_POINT('Ctrl Pts',(2.44790634338457,-4.26634359762335,13.9721974292407));
#25778=CARTESIAN_POINT('Ctrl Pts',(2.50745034939835,-4.23162211926783,13.9761034130744));
#25779=CARTESIAN_POINT('Ctrl Pts',(2.66219535798669,-4.13697349897558,13.9864089269786));
#25780=CARTESIAN_POINT('Ctrl Pts',(2.75610371220013,-4.07501235200957,13.992821864936));
#25781=CARTESIAN_POINT('Ctrl Pts',(2.96457023488572,-3.92696034325726,14.0074375041001));
#25782=CARTESIAN_POINT('Ctrl Pts',(3.07765815487796,-3.83897309257753,14.0156442773939));
#25783=CARTESIAN_POINT('Ctrl Pts',(3.22859322960071,-3.71057777133043,14.0269712122641));
#25784=CARTESIAN_POINT('Ctrl Pts',(3.26984242678359,-3.67427982259964,14.0301076505254));
#25785=CARTESIAN_POINT('Ctrl Pts',(3.34323108869436,-3.60748537275188,14.0357590267355));
#25786=CARTESIAN_POINT('Ctrl Pts',(3.37558320074343,-3.57723118394673,14.0382763222217));
#25787=CARTESIAN_POINT('Ctrl Pts',(3.43299790162759,-3.5220670893688,14.0427885685707));
#25788=CARTESIAN_POINT('Ctrl Pts',(3.45820889755284,-3.49731645990656,14.0447858234373));
#25789=CARTESIAN_POINT('Ctrl Pts',(3.53756531648004,-3.41771195653865,14.0511286036384));
#25790=CARTESIAN_POINT('Ctrl Pts',(3.59068931290156,-3.36185571740985,14.0554596100534));
#25791=CARTESIAN_POINT('Ctrl Pts',(3.7679623734281,-3.16646762567048,14.0702613358484));
#25792=CARTESIAN_POINT('Ctrl Pts',(3.88546620096534,-3.02112726447142,14.0806924494521));
#25793=CARTESIAN_POINT('Ctrl Pts',(4.01807730624421,-2.83652639417858,14.0934686204313));
#25794=CARTESIAN_POINT('Ctrl Pts',(4.04132615609887,-2.80330342629285,14.0957501345275));
#25795=CARTESIAN_POINT('Ctrl Pts',(4.10503251732457,-2.7098261982146,14.1021234083423));
#25796=CARTESIAN_POINT('Ctrl Pts',(4.14457086811401,-2.64895869173633,14.1062210145287));
#25797=CARTESIAN_POINT('Ctrl Pts',(4.21633100668064,-2.53294523728996,14.1139438579367));
#25798=CARTESIAN_POINT('Ctrl Pts',(4.24885390645133,-2.47800304702044,14.1175658497177));
#25799=CARTESIAN_POINT('Ctrl Pts',(4.3341246529263,-2.32733527915788,14.1274096044594));
#25800=CARTESIAN_POINT('Ctrl Pts',(4.38476603186628,-2.23046013350441,14.1336445153872));
#25801=CARTESIAN_POINT('Ctrl Pts',(4.49116297592678,-2.00927325328605,14.1476792493686));
#25802=CARTESIAN_POINT('Ctrl Pts',(4.54506679379011,-1.8841687036833,14.1554814282547));
#25803=CARTESIAN_POINT('Ctrl Pts',(4.61295638002113,-1.70666898952153,14.1663430833198));
#25804=CARTESIAN_POINT('Ctrl Pts',(4.63137469552708,-1.65603565853215,14.1694182335561));
#25805=CARTESIAN_POINT('Ctrl Pts',(4.66322840388901,-1.56377620851263,14.1749760779869));
#25806=CARTESIAN_POINT('Ctrl Pts',(4.67694753568088,-1.52225391618948,14.1774610117201));
#25807=CARTESIAN_POINT('Ctrl Pts',(4.70249312506016,-1.44133038089155,14.1822696488373));
#25808=CARTESIAN_POINT('Ctrl Pts',(4.71438258399559,-1.40195283541347,14.1845938005728));
#25809=CARTESIAN_POINT('Ctrl Pts',(4.7556809245083,-1.25870389093789,14.193000727328));
#25810=CARTESIAN_POINT('Ctrl Pts',(4.78216222984586,-1.15401968430612,14.1990541949692));
#25811=CARTESIAN_POINT('Ctrl Pts',(4.82757093079337,-0.945925394577104,
14.2109896915945));
#25812=CARTESIAN_POINT('Ctrl Pts',(4.84667113820963,-0.842611869243496,
14.2168688388425));
#25813=CARTESIAN_POINT('Ctrl Pts',(4.87453826802848,-0.659194625513001,
14.2272764926467));
#25814=CARTESIAN_POINT('Ctrl Pts',(4.88467270559163,-0.579338656424719,
14.2317977431269));
#25815=CARTESIAN_POINT('Ctrl Pts',(4.90031603341352,-0.426034303383812,
14.2404774828004));
#25816=CARTESIAN_POINT('Ctrl Pts',(4.90614382516365,-0.352640120360553,
14.2446328739957));
#25817=CARTESIAN_POINT('Ctrl Pts',(4.91390970225144,-0.216033067373404,
14.2523774234397));
#25818=CARTESIAN_POINT('Ctrl Pts',(4.916280361264,-0.152859893171549,14.2559628585982));
#25819=CARTESIAN_POINT('Ctrl Pts',(4.9199760899503,0.0498357403372268,14.2674870649977));
#25820=CARTESIAN_POINT('Ctrl Pts',(4.91658265046109,0.189373944499596,14.2754527703436));
#25821=CARTESIAN_POINT('Ctrl Pts',(4.89868946124453,0.456606728287852,14.2907784952849));
#25822=CARTESIAN_POINT('Ctrl Pts',(4.88510979815556,0.584252151718793,14.2981296696833));
#25823=CARTESIAN_POINT('Ctrl Pts',(4.85758054794787,0.772622145415723,14.3089992894859));
#25824=CARTESIAN_POINT('Ctrl Pts',(4.84744567471641,0.8338491015791,14.3125353958361));
#25825=CARTESIAN_POINT('Ctrl Pts',(4.82940046101154,0.931371209801383,14.3181672661824));
#25826=CARTESIAN_POINT('Ctrl Pts',(4.82223300428199,0.967796485959617,14.3202703654164));
#25827=CARTESIAN_POINT('Ctrl Pts',(4.80230443987185,1.06335025786377,14.3257873640336));
#25828=CARTESIAN_POINT('Ctrl Pts',(4.78886373653931,1.12233058794211,14.3291936642752));
#25829=CARTESIAN_POINT('Ctrl Pts',(4.7330112354986,1.34811195991372,14.3422659123206));
#25830=CARTESIAN_POINT('Ctrl Pts',(4.68294354155497,1.51289178801349,14.3518793025374));
#25831=CARTESIAN_POINT('Ctrl Pts',(4.59676063163994,1.75086711670799,14.3660772891082));
#25832=CARTESIAN_POINT('Ctrl Pts',(4.56730259648165,1.82633260776676,14.3706271284036));
#25833=CARTESIAN_POINT('Ctrl Pts',(4.50744455649639,1.96915777886446,14.3793492147358));
#25834=CARTESIAN_POINT('Ctrl Pts',(4.47736382856672,2.03662754716905,14.3835182675823));
#25835=CARTESIAN_POINT('Ctrl Pts',(4.4151537895079,2.16811593788381,14.3917511419207));
#25836=CARTESIAN_POINT('Ctrl Pts',(4.38312283903101,2.23216122245357,14.3958132835056));
#25837=CARTESIAN_POINT('Ctrl Pts',(4.29749198320441,2.39442287078337,14.4062479162397));
#25838=CARTESIAN_POINT('Ctrl Pts',(4.24191857735035,2.49155063080567,14.4126323139129));
#25839=CARTESIAN_POINT('Ctrl Pts',(4.11393508689775,2.69851932422035,14.4265496039859));
#25840=CARTESIAN_POINT('Ctrl Pts',(4.04033193021224,2.80752317116742,14.4340826076938));
#25841=CARTESIAN_POINT('Ctrl Pts',(3.91918160854877,2.97229436234543,14.4457707064155));
#25842=CARTESIAN_POINT('Ctrl Pts',(3.87460714634799,3.03017126784096,14.4499373391271));
#25843=CARTESIAN_POINT('Ctrl Pts',(3.80518636244167,3.11627186704895,14.456222031481));
#25844=CARTESIAN_POINT('Ctrl Pts',(3.78127862387289,3.1452385642401,14.4583514554826));
#25845=CARTESIAN_POINT('Ctrl Pts',(3.72332042997619,3.21384479995823,14.4634309502287));
#25846=CARTESIAN_POINT('Ctrl Pts',(3.68896546622392,3.2532210658755,14.4663766007021));
#25847=CARTESIAN_POINT('Ctrl Pts',(3.54451708046733,3.41355095922362,14.4785177337017));
#25848=CARTESIAN_POINT('Ctrl Pts',(3.42905137901958,3.52952389101047,14.4876572778858));
#25849=CARTESIAN_POINT('Ctrl Pts',(3.24183141359206,3.69969090859694,14.5018398398606));
#25850=CARTESIAN_POINT('Ctrl Pts',(3.17401212538648,3.75803546698278,14.506859228625));
#25851=CARTESIAN_POINT('Ctrl Pts',(3.04422743507703,3.86366791659541,14.5162764161599));
#25852=CARTESIAN_POINT('Ctrl Pts',(2.98265577040692,3.91139550659128,14.5206693664105));
#25853=CARTESIAN_POINT('Ctrl Pts',(2.86466892410699,3.99844710003593,14.5289624882789));
#25854=CARTESIAN_POINT('Ctrl Pts',(2.80851181943608,4.03808970603537,14.5328589103162));
#25855=CARTESIAN_POINT('Ctrl Pts',(2.64790614046063,4.14649369033188,14.5438701153153));
#25856=CARTESIAN_POINT('Ctrl Pts',(2.54164079857574,4.21246700050306,14.5510036427974));
#25857=CARTESIAN_POINT('Ctrl Pts',(2.31910268857065,4.33913758507798,14.565648729108));
#25858=CARTESIAN_POINT('Ctrl Pts',(2.20268208430339,4.39937994741953,14.5731563332335));
#25859=CARTESIAN_POINT('Ctrl Pts',(2.01793802303975,4.48580289828152,14.584812487278));
#25860=CARTESIAN_POINT('Ctrl Pts',(1.95120111566569,4.51523154515605,14.5889725340172));
#25861=CARTESIAN_POINT('Ctrl Pts',(1.84914731351935,4.55754838781354,14.5952502862206));
#25862=CARTESIAN_POINT('Ctrl Pts',(1.81429686836374,4.57153366199735,14.5973793125899));
#25863=CARTESIAN_POINT('Ctrl Pts',(1.73053078028478,4.60403971244273,14.6024611196625));
#25864=CARTESIAN_POINT('Ctrl Pts',(1.68147320643391,4.62218199592597,14.6054094616593));
#25865=CARTESIAN_POINT('Ctrl Pts',(1.47781971552132,4.69382490516186,14.6175552550523));
#25866=CARTESIAN_POINT('Ctrl Pts',(1.32089082730505,4.74037883982954,14.6266968022821));
#25867=CARTESIAN_POINT('Ctrl Pts',(1.07507022033003,4.80014565813485,14.6408784934936));
#25868=CARTESIAN_POINT('Ctrl Pts',(0.98764783592732,4.81889259894746,14.6458949550466));
#25869=CARTESIAN_POINT('Ctrl Pts',(0.823209273332857,4.84949204305968,14.6553078253636));
#25870=CARTESIAN_POINT('Ctrl Pts',(0.746327949929668,4.86191741828524,14.6596993964142));
#25871=CARTESIAN_POINT('Ctrl Pts',(0.601083152989585,4.88186515645548,14.6679915998785));
#25872=CARTESIAN_POINT('Ctrl Pts',(0.532793539321853,4.88978928629886,14.6718884930598));
#25873=CARTESIAN_POINT('Ctrl Pts',(0.344236739056679,4.90767192429651,14.682651746766));
#25874=CARTESIAN_POINT('Ctrl Pts',(0.22373541332353,4.91463981411025,14.6895349031257));
#25875=CARTESIAN_POINT('Ctrl Pts',(-0.0310519859282602,4.91998210022382,
14.7041082395092));
#25876=CARTESIAN_POINT('Ctrl Pts',(-0.165264155542381,4.9173037174781,14.7117966986442));
#25877=CARTESIAN_POINT('Ctrl Pts',(-0.352663529595229,4.90588224790001,
14.722526950132));
#25878=CARTESIAN_POINT('Ctrl Pts',(-0.406072135881076,4.90175047141565,
14.7255842283075));
#25879=CARTESIAN_POINT('Ctrl Pts',(-0.502774701096095,4.89267803307819,
14.7311147426369));
#25880=CARTESIAN_POINT('Ctrl Pts',(-0.546090903859773,4.88803288852975,
14.7335901841687));
#25881=CARTESIAN_POINT('Ctrl Pts',(-0.630303713928392,4.87786867006708,
14.7383966394427));
#25882=CARTESIAN_POINT('Ctrl Pts',(-0.671203866723175,4.87240915232685,
14.740728026222));
#25883=CARTESIAN_POINT('Ctrl Pts',(-0.819163543775919,4.85076048682675,
14.7491601232085));
#25884=CARTESIAN_POINT('Ctrl Pts',(-0.925750667805225,4.83155175879844,
14.7552314364843));
#25885=CARTESIAN_POINT('Ctrl Pts',(-1.18850958994432,4.77518333471985,14.7702906094161));
#25886=CARTESIAN_POINT('Ctrl Pts',(-1.34365934212007,4.73386839907784,14.7792667500666));
#25887=CARTESIAN_POINT('Ctrl Pts',(-1.57395847276817,4.66030556117216,14.792864759978));
#25888=CARTESIAN_POINT('Ctrl Pts',(-1.65078012129937,4.63365060990808,14.7974474276197));
#25889=CARTESIAN_POINT('Ctrl Pts',(-1.79118794483762,4.58099794748697,14.8059252433829));
#25890=CARTESIAN_POINT('Ctrl Pts',(-1.85495852337486,4.55554883441805,14.8098154601947));
#25891=CARTESIAN_POINT('Ctrl Pts',(-2.02075323715779,4.48532600740488,14.8200430072974));
#25892=CARTESIAN_POINT('Ctrl Pts',(-2.12182466152272,4.43840654269116,14.8263934457869));
#25893=CARTESIAN_POINT('Ctrl Pts',(-2.35139336995664,4.32220094464652,14.841099348348));
#25894=CARTESIAN_POINT('Ctrl Pts',(-2.47857510630205,4.25054550676974,14.8494603765965));
#25895=CARTESIAN_POINT('Ctrl Pts',(-2.64933455226606,4.14406457181817,14.8609638328261));
#25896=CARTESIAN_POINT('Ctrl Pts',(-2.69578934792101,4.113996184883,14.8641227379261));
#25897=CARTESIAN_POINT('Ctrl Pts',(-2.77866896370851,4.05834471960723,14.8698083265298));
#25898=CARTESIAN_POINT('Ctrl Pts',(-2.81527276189438,4.03303885567056,14.8723374111537));
#25899=CARTESIAN_POINT('Ctrl Pts',(-2.88458969773298,3.9837133272001,14.8771589419322));
#25900=CARTESIAN_POINT('Ctrl Pts',(-2.91735865944358,3.95977879275916,14.8794521699746));
#25901=CARTESIAN_POINT('Ctrl Pts',(-3.04943741624175,3.86077855671869,14.888761734365));
#25902=CARTESIAN_POINT('Ctrl Pts',(-3.14617741650998,3.78236010702591,14.8957368326135));
#25903=CARTESIAN_POINT('Ctrl Pts',(-3.30825340242307,3.64045479427342,14.9078057880056));
#25904=CARTESIAN_POINT('Ctrl Pts',(-3.37499356530957,3.57866875468029,14.9128973185698));
#25905=CARTESIAN_POINT('Ctrl Pts',(-3.49730285280509,3.4589721361504,14.9224980931795));
#25906=CARTESIAN_POINT('Ctrl Pts',(-3.55324229872355,3.40148268983198,14.9270036457929));
#25907=CARTESIAN_POINT('Ctrl Pts',(-3.65769162020997,3.28874969963707,14.9356601422778));
#25908=CARTESIAN_POINT('Ctrl Pts',(-3.70641801954624,3.23373590035625,14.9398080407918));
#25909=CARTESIAN_POINT('Ctrl Pts',(-3.79478102427495,3.12934897288139,14.9475492571313));
#25910=CARTESIAN_POINT('Ctrl Pts',(-3.83473249579089,3.08026209778686,14.9511389117518));
#25911=CARTESIAN_POINT('Ctrl Pts',(-3.95094342764352,2.93171190368531,14.9618605913808));
#25912=CARTESIAN_POINT('Ctrl Pts',(-4.02435976481273,2.83009124924692,14.9690127335073));
#25913=CARTESIAN_POINT('Ctrl Pts',(-4.17898571671349,2.59786043251403,14.9849721445177));
#25914=CARTESIAN_POINT('Ctrl Pts',(-4.25811535831989,2.46601993104681,14.9937800304174));
#25915=CARTESIAN_POINT('Ctrl Pts',(-4.34357566735924,2.30721567785916,15.0040689149052));
#25916=CARTESIAN_POINT('Ctrl Pts',(-4.35601794539661,2.28363776280585,15.0055884258566));
#25917=CARTESIAN_POINT('Ctrl Pts',(-4.38781443155689,2.22217845140705,15.0095276572629));
#25918=CARTESIAN_POINT('Ctrl Pts',(-4.40687008704669,2.18414483210621,15.0119443343971));
#25919=CARTESIAN_POINT('Ctrl Pts',(-4.44124461332515,2.11325415963933,15.0164077075403));
#25920=CARTESIAN_POINT('Ctrl Pts',(-4.45669823462681,2.08046575050416,15.0184560912733));
#25921=CARTESIAN_POINT('Ctrl Pts',(-4.5402659828963,1.89795265494197,15.029779340586));
#25922=CARTESIAN_POINT('Ctrl Pts',(-4.6011988447425,1.74505300773222,15.0389769283129));
#25923=CARTESIAN_POINT('Ctrl Pts',(-4.68729486763718,1.49292959920582,15.0539037972743));
#25924=CARTESIAN_POINT('Ctrl Pts',(-4.71722674372294,1.39547253369909,15.0596171653545));
#25925=CARTESIAN_POINT('Ctrl Pts',(-4.75094897008291,1.27213976150744,15.0668064032774));
#25926=CARTESIAN_POINT('Ctrl Pts',(-4.75759111255687,1.24706955162331,15.0682656424916));
#25927=CARTESIAN_POINT('Ctrl Pts',(-4.76403458707897,1.2219482458825,15.0697260295707));
#25928=CARTESIAN_POINT('Origin',(0.,0.,-3.23514056400928));
#25929=CARTESIAN_POINT('',(-4.76403457365963,1.22194829820076,17.1653174600137));
#25930=CARTESIAN_POINT('',(-4.76403458706411,1.22194824594044,16.8201710428097));
#25931=CARTESIAN_POINT('',(-4.76403458704967,1.22194824599672,-3.23514056400928));
#25932=CARTESIAN_POINT('',(-4.91824987842825,-5.7598872651143E-5,15.4853473318374));
#25933=CARTESIAN_POINT('Ctrl Pts',(-4.76403457365963,1.22194829820076,17.1653174600137));
#25934=CARTESIAN_POINT('Ctrl Pts',(-4.7435882878598,1.3016626466693,17.1607000675729));
#25935=CARTESIAN_POINT('Ctrl Pts',(-4.72114095238727,1.38086506133652,17.156075181965));
#25936=CARTESIAN_POINT('Ctrl Pts',(-4.67543677500989,1.52794436177981,17.1473970567574));
#25937=CARTESIAN_POINT('Ctrl Pts',(-4.65266761493952,1.59593449705834,17.1433488446468));
#25938=CARTESIAN_POINT('Ctrl Pts',(-4.60401244775245,1.73131762648301,17.1352040831917));
#25939=CARTESIAN_POINT('Ctrl Pts',(-4.57811266782932,1.79868718250882,17.131108378121));
#25940=CARTESIAN_POINT('Ctrl Pts',(-4.49588483867522,1.99927958484134,17.1187747412416));
#25941=CARTESIAN_POINT('Ctrl Pts',(-4.43515439691572,2.13061116431127,17.1105106302183));
#25942=CARTESIAN_POINT('Ctrl Pts',(-4.31389815823793,2.36510340138688,17.0954005820732));
#25943=CARTESIAN_POINT('Ctrl Pts',(-4.25522810851253,2.46910214550434,17.08856454819));
#25944=CARTESIAN_POINT('Ctrl Pts',(-4.16364361053867,2.61846769925544,17.0785667469425));
#25945=CARTESIAN_POINT('Ctrl Pts',(-4.13364592803784,2.66557173095634,17.0753866464699));
#25946=CARTESIAN_POINT('Ctrl Pts',(-4.08255611344895,2.74285859806554,17.07012742685));
#25947=CARTESIAN_POINT('Ctrl Pts',(-4.06191581932615,2.77333330500112,17.0680431022528));
#25948=CARTESIAN_POINT('Ctrl Pts',(-4.00448435002738,2.85611223367364,17.0623502732961));
#25949=CARTESIAN_POINT('Ctrl Pts',(-3.9670120848231,2.90793522441979,17.0587507978996));
#25950=CARTESIAN_POINT('Ctrl Pts',(-3.86761470075161,3.03990035527551,17.0494689412395));
#25951=CARTESIAN_POINT('Ctrl Pts',(-3.80420582253675,3.11888696519914,17.0437988562822));
#25952=CARTESIAN_POINT('Ctrl Pts',(-3.63473477380734,3.31712818357754,17.0291878548076));
#25953=CARTESIAN_POINT('Ctrl Pts',(-3.52522779067636,3.43327895638431,17.0202489123287));
#25954=CARTESIAN_POINT('Ctrl Pts',(-3.36470360389514,3.58775025085969,17.0076907505431));
#25955=CARTESIAN_POINT('Ctrl Pts',(-3.31829503152825,3.63071620766254,17.0041190290465));
#25956=CARTESIAN_POINT('Ctrl Pts',(-3.21744103329441,3.72053946305271,16.9964734427018));
#25957=CARTESIAN_POINT('Ctrl Pts',(-3.16277155953977,3.76712311986316,16.9923980728256));
#25958=CARTESIAN_POINT('Ctrl Pts',(-3.07605618755443,3.83779434337348,16.9860344504823));
#25959=CARTESIAN_POINT('Ctrl Pts',(-3.04470249900674,3.86271585271366,16.9837533197907));
#25960=CARTESIAN_POINT('Ctrl Pts',(-2.86359398858533,4.00309489417528,16.9706871672441));
#25961=CARTESIAN_POINT('Ctrl Pts',(-2.707584131138,4.11022219394695,16.9598504667024));
#25962=CARTESIAN_POINT('Ctrl Pts',(-2.48067562118521,4.24749624362917,16.944687352597));
#25963=CARTESIAN_POINT('Ctrl Pts',(-2.41464844272446,4.2853761763514,16.9403427701605));
#25964=CARTESIAN_POINT('Ctrl Pts',(-2.31702584494433,4.33840965259396,16.934024869532));
#25965=CARTESIAN_POINT('Ctrl Pts',(-2.28610579611743,4.35478213119361,16.9320389401891));
#25966=CARTESIAN_POINT('Ctrl Pts',(-2.21615766620555,4.39087006168276,16.9275816717394));
#25967=CARTESIAN_POINT('Ctrl Pts',(-2.177036001686,4.41039782873514,16.9251129085179));
#25968=CARTESIAN_POINT('Ctrl Pts',(-2.0889894083395,4.45288970521857,16.9196038272885));
#25969=CARTESIAN_POINT('Ctrl Pts',(-2.03993581364031,4.47557431221357,16.9165664810994));
#25970=CARTESIAN_POINT('Ctrl Pts',(-1.86409303583123,4.55340031043252,16.9057728605231));
#25971=CARTESIAN_POINT('Ctrl Pts',(-1.73536463069232,4.60399902460852,16.8980419356125));
#25972=CARTESIAN_POINT('Ctrl Pts',(-1.49353161245578,4.68746957899087,16.883696015127));
#25973=CARTESIAN_POINT('Ctrl Pts',(-1.3810487454063,4.72183349901057,16.8770920234809));
#25974=CARTESIAN_POINT('Ctrl Pts',(-1.20129016207633,4.76977699789816,16.8665972404686));
#25975=CARTESIAN_POINT('Ctrl Pts',(-1.13477589568856,4.78603742053143,16.8627267293476));
#25976=CARTESIAN_POINT('Ctrl Pts',(-0.991467640299607,4.81791584412069,
16.854406290497));
#25977=CARTESIAN_POINT('Ctrl Pts',(-0.914595990783938,4.83309788160964,
16.8499544940678));
#25978=CARTESIAN_POINT('Ctrl Pts',(-0.687611191202474,4.87231761713459,
16.8368325999193));
#25979=CARTESIAN_POINT('Ctrl Pts',(-0.536709200484851,4.8912401825467,16.8281363531721));
#25980=CARTESIAN_POINT('Ctrl Pts',(-0.259547906279528,4.91301308622068,
16.812221618506));
#25981=CARTESIAN_POINT('Ctrl Pts',(-0.133586471180473,4.9180502160204,16.8050111867082));
#25982=CARTESIAN_POINT('Ctrl Pts',(0.0286577518124332,4.91829993419519,
16.7957804389627));
#25983=CARTESIAN_POINT('Ctrl Pts',(0.0648851788747955,4.91795541444086,
16.7937230485191));
#25984=CARTESIAN_POINT('Ctrl Pts',(0.142601995657612,4.91635743229706,16.7893190938912));
#25985=CARTESIAN_POINT('Ctrl Pts',(0.18408611491318,4.91497895048201,16.7869742880521));
#25986=CARTESIAN_POINT('Ctrl Pts',(0.25128220393893,4.9118941312388,16.7831817213911));
#25987=CARTESIAN_POINT('Ctrl Pts',(0.277006726870557,4.91051056259284,16.7817311457572));
#25988=CARTESIAN_POINT('Ctrl Pts',(0.453643593825276,4.89961787513667,16.771775928592));
#25989=CARTESIAN_POINT('Ctrl Pts',(0.604059421862266,4.88335547473123,16.7633217649779));
#25990=CARTESIAN_POINT('Ctrl Pts',(0.851708956657628,4.84496173910409,16.7492763997331));
#25991=CARTESIAN_POINT('Ctrl Pts',(0.949445586010876,4.82676032493256,16.7437007859473));
#25992=CARTESIAN_POINT('Ctrl Pts',(1.12230603337375,4.78911488208626,16.7337450089658));
#25993=CARTESIAN_POINT('Ctrl Pts',(1.19764800332343,4.77083129624926,16.7293733458068));
#25994=CARTESIAN_POINT('Ctrl Pts',(1.33889504060652,4.73299736503347,16.7211032083921));
#25995=CARTESIAN_POINT('Ctrl Pts',(1.40488401512382,4.71383121768918,16.7172083590564));
#25996=CARTESIAN_POINT('Ctrl Pts',(1.58677921657446,4.65684183093536,16.7063769534346));
#25997=CARTESIAN_POINT('Ctrl Pts',(1.70171256068583,4.61608252210859,16.6994230385123));
#25998=CARTESIAN_POINT('Ctrl Pts',(1.96775292364144,4.51044783243746,16.6830540132048));
#25999=CARTESIAN_POINT('Ctrl Pts',(2.11735888099621,4.44218221295468,16.6736332160375));
#26000=CARTESIAN_POINT('Ctrl Pts',(2.31096876311112,4.34183063695612,16.6611928660984));
#26001=CARTESIAN_POINT('Ctrl Pts',(2.35826316329169,4.31632538758996,16.6581338423023));
#26002=CARTESIAN_POINT('Ctrl Pts',(2.43408567861289,4.27381701620875,16.6532004235577));
#26003=CARTESIAN_POINT('Ctrl Pts',(2.4628757389652,4.25729116918938,16.6513205233435));
#26004=CARTESIAN_POINT('Ctrl Pts',(2.54398585504326,4.20963481331582,16.6460037671551));
#26005=CARTESIAN_POINT('Ctrl Pts',(2.59589841320415,4.17782250143452,16.6425756591444));
#26006=CARTESIAN_POINT('Ctrl Pts',(2.68730752117895,4.11944477087858,16.6364801888386));
#26007=CARTESIAN_POINT('Ctrl Pts',(2.72703403811147,4.09325449034184,16.6338105800471));
#26008=CARTESIAN_POINT('Ctrl Pts',(2.9525842303575,3.93981602122527,16.6185157831822));
#26009=CARTESIAN_POINT('Ctrl Pts',(3.12987152550727,3.80050087641063,16.6059362661294));
#26010=CARTESIAN_POINT('Ctrl Pts',(3.34768553528662,3.6037276353272,16.5893819934988));
#26011=CARTESIAN_POINT('Ctrl Pts',(3.39742467396146,3.55687457749323,16.5855205639085));
#26012=CARTESIAN_POINT('Ctrl Pts',(3.500637767178,3.45550954527971,16.5773241025328));
#26013=CARTESIAN_POINT('Ctrl Pts',(3.55385106149317,3.40075777402751,16.5729877385427));
#26014=CARTESIAN_POINT('Ctrl Pts',(3.71281058769227,3.2293954028356,16.5596776202371));
#26015=CARTESIAN_POINT('Ctrl Pts',(3.81425112626018,3.10892980361486,16.5506736484283));
#26016=CARTESIAN_POINT('Ctrl Pts',(3.98691091419381,2.88269056516686,16.5343820819906));
#26017=CARTESIAN_POINT('Ctrl Pts',(4.06013100732523,2.77861482064724,16.5271034824382));
#26018=CARTESIAN_POINT('Ctrl Pts',(4.14883680849413,2.64152195570325,16.517813771439));
#26019=CARTESIAN_POINT('Ctrl Pts',(4.16810533262779,2.61101188760507,16.5157646508863));
#26020=CARTESIAN_POINT('Ctrl Pts',(4.20892156697231,2.54477944597455,16.5113571641546));
#26021=CARTESIAN_POINT('Ctrl Pts',(4.23035412696273,2.50898927829548,16.5090006358365));
#26022=CARTESIAN_POINT('Ctrl Pts',(4.26438376551111,2.45048735718644,16.5051850200385));
#26023=CARTESIAN_POINT('Ctrl Pts',(4.27726072637742,2.42794107745536,16.5037231157302));
#26024=CARTESIAN_POINT('Ctrl Pts',(4.30891673555707,2.37148104417662,16.5000821332972));
#26025=CARTESIAN_POINT('Ctrl Pts',(4.32747452750783,2.337445189415,16.4979049400579));
#26026=CARTESIAN_POINT('Ctrl Pts',(4.41888705791368,2.16496950380238,16.486951248353));
#26027=CARTESIAN_POINT('Ctrl Pts',(4.48550950147534,2.02332903777803,16.4782073795908));
#26028=CARTESIAN_POINT('Ctrl Pts',(4.58441777519533,1.7840404206516,16.4636757489455));
#26029=CARTESIAN_POINT('Ctrl Pts',(4.62059686826783,1.6881264086129,16.4579128179635));
#26030=CARTESIAN_POINT('Ctrl Pts',(4.67562500319894,1.52718191597249,16.4483122508563));
#26031=CARTESIAN_POINT('Ctrl Pts',(4.69617571387768,1.462767002805,16.444488033603));
#26032=CARTESIAN_POINT('Ctrl Pts',(4.73900726484476,1.31829285946753,16.4359430998373));
#26033=CARTESIAN_POINT('Ctrl Pts',(4.76060021522881,1.23805140158652,16.431218850975));
#26034=CARTESIAN_POINT('Ctrl Pts',(4.80401732184332,1.05872030433921,16.4207003602173));
#26035=CARTESIAN_POINT('Ctrl Pts',(4.82482910460444,0.959424280793805,16.4149025206396));
#26036=CARTESIAN_POINT('Ctrl Pts',(4.87128567225963,0.69769805528553,16.399689803974));
#26037=CARTESIAN_POINT('Ctrl Pts',(4.89188283033444,0.534499647991539,16.3902705957283));
#26038=CARTESIAN_POINT('Ctrl Pts',(4.90698776454125,0.334598155320559,16.3788655219691));
#26039=CARTESIAN_POINT('Ctrl Pts',(4.90931034472373,0.298591395049708,16.3768166078053));
#26040=CARTESIAN_POINT('Ctrl Pts',(4.91346376696336,0.220901438333412,16.372409024554));
#26041=CARTESIAN_POINT('Ctrl Pts',(4.91516084216039,0.179213791346714,16.3700521953385));
#26042=CARTESIAN_POINT('Ctrl Pts',(4.91985951689027,0.0112235388383775,
16.3605775728024));
#26043=CARTESIAN_POINT('Ctrl Pts',(4.91852459017969,-0.115152817134032,
16.3535007286764));
#26044=CARTESIAN_POINT('Ctrl Pts',(4.9038677968834,-0.413484588303955,16.3367669739928));
#26045=CARTESIAN_POINT('Ctrl Pts',(4.88636740155251,-0.585065426077207,
16.3271183933113));
#26046=CARTESIAN_POINT('Ctrl Pts',(4.84895669978049,-0.82575776687166,16.3133918929845));
#26047=CARTESIAN_POINT('Ctrl Pts',(4.83648887165774,-0.895897431022879,
16.3093692487406));
#26048=CARTESIAN_POINT('Ctrl Pts',(4.80822870795427,-1.03701674010458,16.3012201523235));
#26049=CARTESIAN_POINT('Ctrl Pts',(4.79237693190637,-1.10796669787156,16.2970942599748));
#26050=CARTESIAN_POINT('Ctrl Pts',(4.75599208485935,-1.255383278971,16.2884546484954));
#26051=CARTESIAN_POINT('Ctrl Pts',(4.73517344310343,-1.33175830351492,16.2839402716194));
#26052=CARTESIAN_POINT('Ctrl Pts',(4.66202769413637,-1.57664434632021,16.269336817161));
#26053=CARTESIAN_POINT('Ctrl Pts',(4.60247506198401,-1.74285192690166,16.2592213224859));
#26054=CARTESIAN_POINT('Ctrl Pts',(4.51083855416828,-1.96090028637332,16.245719189578));
#26055=CARTESIAN_POINT('Ctrl Pts',(4.48654229213352,-2.01587022889027,16.2422953972963));
#26056=CARTESIAN_POINT('Ctrl Pts',(4.44577518726742,-2.10371491977322,16.2367966414425));
#26057=CARTESIAN_POINT('Ctrl Pts',(4.42993266430623,-2.13687391039157,16.2347149593188));
#26058=CARTESIAN_POINT('Ctrl Pts',(4.3869916370064,-2.22422069827699,16.2292140017611));
#26059=CARTESIAN_POINT('Ctrl Pts',(4.35926096315105,-2.27809071909811,16.2258024405227));
#26060=CARTESIAN_POINT('Ctrl Pts',(4.26508296230659,-2.45302236526538,16.2146366750122));
#26061=CARTESIAN_POINT('Ctrl Pts',(4.19453205498405,-2.5717994959412,16.2069138435397));
#26062=CARTESIAN_POINT('Ctrl Pts',(4.04837820845451,-2.79581062715771,16.1919234728479));
#26063=CARTESIAN_POINT('Ctrl Pts',(3.9734322173684,-2.90133745138393,16.1846639198916));
#26064=CARTESIAN_POINT('Ctrl Pts',(3.8559172536894,-3.05369582828456,16.1738165299351));
#26065=CARTESIAN_POINT('Ctrl Pts',(3.8164653572522,-3.10286128419825,16.1702562155462));
#26066=CARTESIAN_POINT('Ctrl Pts',(3.72986585881353,-3.20663157720159,16.1626042228905));
#26067=CARTESIAN_POINT('Ctrl Pts',(3.68243982414509,-3.26098484747825,16.158510899697));
#26068=CARTESIAN_POINT('Ctrl Pts',(3.53613864565559,-3.42139232428936,16.1461595840663));
#26069=CARTESIAN_POINT('Ctrl Pts',(3.4337537384426,-3.52413625334683,16.1378752065714));
#26070=CARTESIAN_POINT('Ctrl Pts',(3.24054661756337,-3.70159620424662,16.1228595923853));
#26071=CARTESIAN_POINT('Ctrl Pts',(3.15129741141974,-3.77786734671018,16.1161384551606));
#26072=CARTESIAN_POINT('Ctrl Pts',(3.01487609011523,-3.88625006958355,16.106194969443));
#26073=CARTESIAN_POINT('Ctrl Pts',(2.96973631982194,-3.92085242529157,16.1029557193361));
#26074=CARTESIAN_POINT('Ctrl Pts',(2.89443945789357,-3.97652554281347,16.0976394198877));
#26075=CARTESIAN_POINT('Ctrl Pts',(2.86462842573123,-3.99805442530318,16.0955568086521));
#26076=CARTESIAN_POINT('Ctrl Pts',(2.78345115854087,-4.05530477842046,16.0899434630986));
#26077=CARTESIAN_POINT('Ctrl Pts',(2.73164012147523,-4.09038379453623,16.0864212140372));
#26078=CARTESIAN_POINT('Ctrl Pts',(2.56205194291797,-4.2005450275659,16.075058118365));
#26079=CARTESIAN_POINT('Ctrl Pts',(2.44174233374725,-4.2716019761059,16.0672479771617));
#26080=CARTESIAN_POINT('Ctrl Pts',(2.20797088217651,-4.39656405884317,16.052390475707));
#26081=CARTESIAN_POINT('Ctrl Pts',(2.09515036031063,-4.45143295539299,16.0453523220755));
#26082=CARTESIAN_POINT('Ctrl Pts',(1.92278636543803,-4.52725429192827,16.0347360508165));
#26083=CARTESIAN_POINT('Ctrl Pts',(1.8647353205005,-4.55147238913325,16.031183282393));
#26084=CARTESIAN_POINT('Ctrl Pts',(1.73894397586434,-4.60114019700116,16.0235261849199));
#26085=CARTESIAN_POINT('Ctrl Pts',(1.67107423019433,-4.6262217863785,16.0194201141789));
#26086=CARTESIAN_POINT('Ctrl Pts',(1.46401687848547,-4.69758962382259,16.0069596016588));
#26087=CARTESIAN_POINT('Ctrl Pts',(1.32329034517427,-4.73915556268299,15.9985780448355));
#26088=CARTESIAN_POINT('Ctrl Pts',(1.03597241981382,-4.81022234858021,15.9816365264345));
#26089=CARTESIAN_POINT('Ctrl Pts',(0.889467350789513,-4.83945517934842,
15.9730847673));
#26090=CARTESIAN_POINT('Ctrl Pts',(0.70141699179698,-4.86814860996931,15.9622593411364));
#26091=CARTESIAN_POINT('Ctrl Pts',(0.660899351644574,-4.87381460365856,
15.9599359281631));
#26092=CARTESIAN_POINT('Ctrl Pts',(0.590544755488948,-4.88275952430427,
15.9559191038084));
#26093=CARTESIAN_POINT('Ctrl Pts',(0.560739917416643,-4.88627203971508,
15.95422279412));
#26094=CARTESIAN_POINT('Ctrl Pts',(0.487118180101782,-4.89426591007949,
15.9500435444097));
#26095=CARTESIAN_POINT('Ctrl Pts',(0.443269559174345,-4.89843189866882,
15.9475638632177));
#26096=CARTESIAN_POINT('Ctrl Pts',(0.313284914341319,-4.9090218544607,15.9402325057621));
#26097=CARTESIAN_POINT('Ctrl Pts',(0.227028880546364,-4.91376648383623,
15.9353924780907));
#26098=CARTESIAN_POINT('Ctrl Pts',(-0.0365325744302362,-4.92130905522521,
15.9206200951733));
#26099=CARTESIAN_POINT('Ctrl Pts',(-0.213900343096126,-4.91679398930186,
15.9106975143877));
#26100=CARTESIAN_POINT('Ctrl Pts',(-0.460607304799696,-4.89713703937088,
15.8967515953338));
#26101=CARTESIAN_POINT('Ctrl Pts',(-0.530451703672448,-4.89006453078622,
15.892787875185));
#26102=CARTESIAN_POINT('Ctrl Pts',(-0.658589957239961,-4.87431151112026,
15.8854787596094));
#26103=CARTESIAN_POINT('Ctrl Pts',(-0.716925410791389,-4.86607349977366,
15.8821370114024));
#26104=CARTESIAN_POINT('Ctrl Pts',(-0.847858006018463,-4.84517787668112,
15.8746003395477));
#26105=CARTESIAN_POINT('Ctrl Pts',(-0.920346955213649,-4.83193265534748,
15.8704024784265));
#26106=CARTESIAN_POINT('Ctrl Pts',(-1.12290585404446,-4.79019731283169,
15.8585964258754));
#26107=CARTESIAN_POINT('Ctrl Pts',(-1.25215603505651,-4.75804715886603,
15.8509732999942));
#26108=CARTESIAN_POINT('Ctrl Pts',(-1.47968191145142,-4.69153735138861,
15.8374065955496));
#26109=CARTESIAN_POINT('Ctrl Pts',(-1.57847415540036,-4.65922751077476,
15.8314653952655));
#26110=CARTESIAN_POINT('Ctrl Pts',(-1.71445520406705,-4.60993328013733,
15.823234635117));
#26111=CARTESIAN_POINT('Ctrl Pts',(-1.75256755089303,-4.59557923804063,
15.8209219108523));
#26112=CARTESIAN_POINT('Ctrl Pts',(-1.82736811057167,-4.56634164153953,
15.8163734182383));
#26113=CARTESIAN_POINT('Ctrl Pts',(-1.86406359717801,-4.55148515873302,
15.8141373284263));
#26114=CARTESIAN_POINT('Ctrl Pts',(-1.94702277317141,-4.51672684505237,
15.8090663729141));
#26115=CARTESIAN_POINT('Ctrl Pts',(-1.9931682454743,-4.49655417854281,15.8062344214535));
#26116=CARTESIAN_POINT('Ctrl Pts',(-2.14482728339731,-4.42746245754207,
15.7968755671675));
#26117=CARTESIAN_POINT('Ctrl Pts',(-2.24891555050614,-4.37550990738065,
15.7903679324805));
#26118=CARTESIAN_POINT('Ctrl Pts',(-2.46571693545719,-4.25751826434365,
15.7765368063815));
#26119=CARTESIAN_POINT('Ctrl Pts',(-2.57783869583992,-4.19058097097493,
15.7692160868953));
#26120=CARTESIAN_POINT('Ctrl Pts',(-2.74606615784336,-4.08083932879514,
15.7578982510804));
#26121=CARTESIAN_POINT('Ctrl Pts',(-2.80413702840918,-4.04115631341736,
15.7539271637776));
#26122=CARTESIAN_POINT('Ctrl Pts',(-2.91876646743411,-3.95916292443407,
15.7459484051873));
#26123=CARTESIAN_POINT('Ctrl Pts',(-2.97530464690947,-3.91685216198046,
15.7419415772266));
#26124=CARTESIAN_POINT('Ctrl Pts',(-3.19637668403009,-3.74386192769029,
15.7259737959945));
#26125=CARTESIAN_POINT('Ctrl Pts',(-3.35337317468545,-3.60391623962902,
15.7139433117501));
#26126=CARTESIAN_POINT('Ctrl Pts',(-3.5659548858786,-3.38846844618353,15.6966263948497));
#26127=CARTESIAN_POINT('Ctrl Pts',(-3.62910069246196,-3.32075008508508,
15.6913371069472));
#26128=CARTESIAN_POINT('Ctrl Pts',(-3.71401907751841,-3.22436550940211,
15.6840295361575));
#26129=CARTESIAN_POINT('Ctrl Pts',(-3.73744487410673,-3.19718258707085,
15.681991967582));
#26130=CARTESIAN_POINT('Ctrl Pts',(-3.77925657675769,-3.14757737940318,
15.6783168435665));
#26131=CARTESIAN_POINT('Ctrl Pts',(-3.79774562588185,-3.12524428041842,
15.6766776752659));
#26132=CARTESIAN_POINT('Ctrl Pts',(-3.84299504239359,-3.06959252811821,
15.6726287855334));
#26133=CARTESIAN_POINT('Ctrl Pts',(-3.86952076263997,-3.03608601609949,
15.6702222072373));
#26134=CARTESIAN_POINT('Ctrl Pts',(-3.94507841544602,-2.93804485393541,
15.6632621057545));
#26135=CARTESIAN_POINT('Ctrl Pts',(-3.99295627561725,-2.87263843868657,
15.658718981789));
#26136=CARTESIAN_POINT('Ctrl Pts',(-4.14693457146008,-2.65099512142812,
15.6435969156073));
#26137=CARTESIAN_POINT('Ctrl Pts',(-4.2456509195922,-2.48983708204874,15.6330335546013));
#26138=CARTESIAN_POINT('Ctrl Pts',(-4.36776085066296,-2.26201236352936,
15.618465678188));
#26139=CARTESIAN_POINT('Ctrl Pts',(-4.39935770089278,-2.19992873914243,
15.6145318228235));
#26140=CARTESIAN_POINT('Ctrl Pts',(-4.44531558208509,-2.10467484944113,
15.6085433777263));
#26141=CARTESIAN_POINT('Ctrl Pts',(-4.46064739747598,-2.07198253390992,
15.6064963644958));
#26142=CARTESIAN_POINT('Ctrl Pts',(-4.51144252121119,-1.96049372621244,
15.5995420269483));
#26143=CARTESIAN_POINT('Ctrl Pts',(-4.54518857288801,-1.88093324009851,
15.5946234704278));
#26144=CARTESIAN_POINT('Ctrl Pts',(-4.62129635660792,-1.68747214795738,
15.5827605665497));
#26145=CARTESIAN_POINT('Ctrl Pts',(-4.66156740531742,-1.57280998657092,
15.5758079286257));
#26146=CARTESIAN_POINT('Ctrl Pts',(-4.73468799479361,-1.33702366023405,
15.5616764419799));
#26147=CARTESIAN_POINT('Ctrl Pts',(-4.76723228708275,-1.21589455173432,
15.5545025313147));
#26148=CARTESIAN_POINT('Ctrl Pts',(-4.8040386929305,-1.05451724675543,15.5450850947102));
#26149=CARTESIAN_POINT('Ctrl Pts',(-4.81248539205324,-1.01527277102387,
15.5428058482511));
#26150=CARTESIAN_POINT('Ctrl Pts',(-4.82703502764815,-0.943407084268541,
15.5386537341665));
#26151=CARTESIAN_POINT('Ctrl Pts',(-4.83329002077137,-0.91081923959383,
15.5367788889788));
#26152=CARTESIAN_POINT('Ctrl Pts',(-4.84757269053403,-0.832113664071977,
15.5322667976335));
#26153=CARTESIAN_POINT('Ctrl Pts',(-4.85527270506987,-0.785939662971163,
15.5296328733288));
#26154=CARTESIAN_POINT('Ctrl Pts',(-4.89954812040739,-0.494886787815442,
15.513091253198));
#26155=CARTESIAN_POINT('Ctrl Pts',(-4.91824709472654,-0.247649462345353,
15.4992917658497));
#26156=CARTESIAN_POINT('Ctrl Pts',(-4.91824999966148,-5.77046521768598E-5,
15.4853475479531));
#26157=CARTESIAN_POINT('Ctrl Pts',(-4.91824999966286,-5.75870754615866E-5,
15.4853475413313));
#26158=CARTESIAN_POINT('Ctrl Pts',(-4.91825044579516,0.0380445423567261,
15.4832016524643));
#26159=CARTESIAN_POINT('Ctrl Pts',(-4.91780812100187,0.0761452482382754,
15.4810533571179));
#26160=CARTESIAN_POINT('Ctrl Pts',(-4.91608020393543,0.150517373830886,
15.4768534137325));
#26161=CARTESIAN_POINT('Ctrl Pts',(-4.91483575734356,0.186787336092719,
15.4748021578625));
#26162=CARTESIAN_POINT('Ctrl Pts',(-4.91004881726367,0.292235419018164,
15.4688279896373));
#26163=CARTESIAN_POINT('Ctrl Pts',(-4.90544620961724,0.361356150664063,
15.4648986567023));
#26164=CARTESIAN_POINT('Ctrl Pts',(-4.8773692316182,0.680998301980589,15.4466526714679));
#26165=CARTESIAN_POINT('Ctrl Pts',(-4.83615212048835,0.929579899055647,
15.4322266241013));
#26166=CARTESIAN_POINT('Ctrl Pts',(-4.77215806660131,1.18994245846746,15.4169086953599));
#26167=CARTESIAN_POINT('Ctrl Pts',(-4.76813656803685,1.20595576894076,15.4159658272421));
#26168=CARTESIAN_POINT('Ctrl Pts',(-4.76403458688904,1.22194824662298,15.4150234826428));
#26169=CARTESIAN_POINT('Ctrl Pts',(-4.76403458707897,1.2219482458825,15.0697260295707));
#26170=CARTESIAN_POINT('Ctrl Pts',(-4.7673671792485,1.20895540071595,15.0704813479208));
#26171=CARTESIAN_POINT('Ctrl Pts',(-4.77064662770679,1.19594888736934,15.0712369728154));
#26172=CARTESIAN_POINT('Ctrl Pts',(-4.79107250321357,1.1135174566575,15.0760230610723));
#26173=CARTESIAN_POINT('Ctrl Pts',(-4.80675611995235,1.04373957717661,15.0800618850286));
#26174=CARTESIAN_POINT('Ctrl Pts',(-4.83555882569426,0.901125677627058,
15.0883009312144));
#26175=CARTESIAN_POINT('Ctrl Pts',(-4.84856673912676,0.828285605891197,
15.0925008639847));
#26176=CARTESIAN_POINT('Ctrl Pts',(-4.88477809217167,0.595249235037764,
15.1059221267969));
#26177=CARTESIAN_POINT('Ctrl Pts',(-4.90171972039349,0.434190427839137,
15.1151779879791));
#26178=CARTESIAN_POINT('Ctrl Pts',(-4.91573024887108,0.181793679350151,
15.1296489402847));
#26179=CARTESIAN_POINT('Ctrl Pts',(-4.91825122801099,0.090872538481914,
15.1348540807445));
#26180=CARTESIAN_POINT('Ctrl Pts',(-4.91824918374074,-0.0604592894478811,
15.143493192483));
#26181=CARTESIAN_POINT('Ctrl Pts',(-4.91713599127383,-0.120847541397437,
15.1469340051527));
#26182=CARTESIAN_POINT('Ctrl Pts',(-4.91354321669377,-0.218298561487058,
15.1524708947497));
#26183=CARTESIAN_POINT('Ctrl Pts',(-4.91175551922442,-0.255380037915821,
15.1545737137732));
#26184=CARTESIAN_POINT('Ctrl Pts',(-4.90585243390948,-0.354482955583493,
15.1601843174804));
#26185=CARTESIAN_POINT('Ctrl Pts',(-4.9009808828241,-0.416452633304532,
15.163683848214));
#26186=CARTESIAN_POINT('Ctrl Pts',(-4.89015599235757,-0.527231673687728,
15.1699385341009));
#26187=CARTESIAN_POINT('Ctrl Pts',(-4.88464288816208,-0.576075306459741,
15.1726958606277));
#26188=CARTESIAN_POINT('Ctrl Pts',(-4.85024570391863,-0.84463418520304,
15.1878744642066));
#26189=CARTESIAN_POINT('Ctrl Pts',(-4.80726966967169,-1.06228403116591,
15.2002543327913));
#26190=CARTESIAN_POINT('Ctrl Pts',(-4.73186070209481,-1.34292123599112,
15.2166419593025));
#26191=CARTESIAN_POINT('Ctrl Pts',(-4.7125569356201,-1.40916646885443,15.220541099801));
#26192=CARTESIAN_POINT('Ctrl Pts',(-4.66873095703343,-1.54857526382148,
15.2288209528956));
#26193=CARTESIAN_POINT('Ctrl Pts',(-4.64386774934535,-1.62161223100499,
15.2332030337889));
#26194=CARTESIAN_POINT('Ctrl Pts',(-4.57988380257849,-1.79600836484919,
15.2437819088672));
#26195=CARTESIAN_POINT('Ctrl Pts',(-4.5391027516234,-1.89671492966034,15.249987034683));
#26196=CARTESIAN_POINT('Ctrl Pts',(-4.42297189926609,-2.15824492923478,
15.2663604701842));
#26197=CARTESIAN_POINT('Ctrl Pts',(-4.34218936948808,-2.3164831052719,15.2765370511216));
#26198=CARTESIAN_POINT('Ctrl Pts',(-4.23508158134163,-2.50090864033163,
15.2886677095506));
#26199=CARTESIAN_POINT('Ctrl Pts',(-4.21679879528527,-2.5316137123602,15.2906965105245));
#26200=CARTESIAN_POINT('Ctrl Pts',(-4.17555173856853,-2.59919949546296,
15.2951809884637));
#26201=CARTESIAN_POINT('Ctrl Pts',(-4.15243010350678,-2.63598077267938,
15.2976343079277));
#26202=CARTESIAN_POINT('Ctrl Pts',(-4.06477627685243,-2.77140222810852,
15.3067256094917));
#26203=CARTESIAN_POINT('Ctrl Pts',(-3.99719139061608,-2.86801987967851,
15.3133299542669));
#26204=CARTESIAN_POINT('Ctrl Pts',(-3.82029020601668,-3.10249728604743,
15.3297857502547));
#26205=CARTESIAN_POINT('Ctrl Pts',(-3.70692863390716,-3.23709527693757,
15.3396276142171));
#26206=CARTESIAN_POINT('Ctrl Pts',(-3.53724083509185,-3.41794012191709,
15.3536010014379));
#26207=CARTESIAN_POINT('Ctrl Pts',(-3.48672688122618,-3.46945570646042,
15.3576746710699));
#26208=CARTESIAN_POINT('Ctrl Pts',(-3.38271318222823,-3.5709652030561,15.3659035803204));
#26209=CARTESIAN_POINT('Ctrl Pts',(-3.32919354032112,-3.62091302792393,
15.3700581174756));
#26210=CARTESIAN_POINT('Ctrl Pts',(-3.21518148216237,-3.722650747756,15.378752555278));
#26211=CARTESIAN_POINT('Ctrl Pts',(-3.15450569920082,-3.7742037796569,15.3832930931403));
#26212=CARTESIAN_POINT('Ctrl Pts',(-2.95460073767163,-3.93586305381782,
15.3979834017141));
#26213=CARTESIAN_POINT('Ctrl Pts',(-2.81065602117549,-4.0399128899484,15.4081599051578));
#26214=CARTESIAN_POINT('Ctrl Pts',(-2.6112183019896,-4.16824703972006,15.4216976837862));
#26215=CARTESIAN_POINT('Ctrl Pts',(-2.56044948534168,-4.1996241451417,15.4250974312394));
#26216=CARTESIAN_POINT('Ctrl Pts',(-2.47718487449013,-4.24901365017875,
15.4305938947043));
#26217=CARTESIAN_POINT('Ctrl Pts',(-2.4450343811341,-4.2675952029147,15.4326970976503));
#26218=CARTESIAN_POINT('Ctrl Pts',(-2.3578198533458,-4.31669218837916,15.4383529135941));
#26219=CARTESIAN_POINT('Ctrl Pts',(-2.30237525024915,-4.346517486669,15.441896957845));
#26220=CARTESIAN_POINT('Ctrl Pts',(-2.15919220207879,-4.42003123344747,
15.4509406281462));
#26221=CARTESIAN_POINT('Ctrl Pts',(-2.07069265300085,-4.46217650934667,
15.4564287188405));
#26222=CARTESIAN_POINT('Ctrl Pts',(-1.84022477623791,-4.5635960396736,15.4705345015754));
#26223=CARTESIAN_POINT('Ctrl Pts',(-1.69662993561883,-4.61890486656072,
15.4791491452054));
#26224=CARTESIAN_POINT('Ctrl Pts',(-1.48124303189271,-4.69046437340751,
15.4919342909448));
#26225=CARTESIAN_POINT('Ctrl Pts',(-1.41129915791689,-4.71198169349157,
15.4960649485231));
#26226=CARTESIAN_POINT('Ctrl Pts',(-1.27147059754913,-4.75160534828729,
15.5042917464087));
#26227=CARTESIAN_POINT('Ctrl Pts',(-1.20161528881772,-4.76974961611879,
15.5083865791224));
#26228=CARTESIAN_POINT('Ctrl Pts',(-1.09237083612256,-4.79557257324288,
15.5147719883428));
#26229=CARTESIAN_POINT('Ctrl Pts',(-1.0532438879321,-4.80431760361842,15.5170553243316));
#26230=CARTESIAN_POINT('Ctrl Pts',(-0.845639032286988,-4.84806008755224,
15.5291527548139));
#26231=CARTESIAN_POINT('Ctrl Pts',(-0.675518662393738,-4.87467595624735,
15.5390090397132));
#26232=CARTESIAN_POINT('Ctrl Pts',(-0.41532894800091,-4.90149925482032,
15.5539739518092));
#26233=CARTESIAN_POINT('Ctrl Pts',(-0.326067346606616,-4.9082454545971,
15.5590874225721));
#26234=CARTESIAN_POINT('Ctrl Pts',(-0.20015466054073,-4.91431151804329,
15.566259597224));
#26235=CARTESIAN_POINT('Ctrl Pts',(-0.163619804365508,-4.9156635544516,
15.5683357904989));
#26236=CARTESIAN_POINT('Ctrl Pts',(-0.0850297787411345,-4.91769476640752,
15.5727896936212));
#26237=CARTESIAN_POINT('Ctrl Pts',(-0.0429739913079264,-4.91824208104107,
15.5751655642479));
#26238=CARTESIAN_POINT('Ctrl Pts',(0.130860436831612,-4.91827445918214,
15.5849657903678));
#26239=CARTESIAN_POINT('Ctrl Pts',(0.26258614695643,-4.91300288791975,15.5923452386219));
#26240=CARTESIAN_POINT('Ctrl Pts',(0.556500497176249,-4.88938504559556,
15.6088637019004));
#26241=CARTESIAN_POINT('Ctrl Pts',(0.718307034272635,-4.86824538256003,
15.617995528561));
#26242=CARTESIAN_POINT('Ctrl Pts',(0.950265436641775,-4.82612265793943,
15.6312774598904));
#26243=CARTESIAN_POINT('Ctrl Pts',(1.02147105341181,-4.81155494976111,15.6353805237688));
#26244=CARTESIAN_POINT('Ctrl Pts',(1.16314485910006,-4.77928367709257,15.6436064374179));
#26245=CARTESIAN_POINT('Ctrl Pts',(1.23359596254363,-4.76158579300629,15.6477282634757));
#26246=CARTESIAN_POINT('Ctrl Pts',(1.34278903712325,-4.73156951539523,15.6541707451116));
#26247=CARTESIAN_POINT('Ctrl Pts',(1.38181438432096,-4.7203200589366,15.6564841327815));
#26248=CARTESIAN_POINT('Ctrl Pts',(1.59824846751835,-4.65501662899941,15.6693764117313));
#26249=CARTESIAN_POINT('Ctrl Pts',(1.77262811341739,-4.59144494174076,15.6800043778367));
#26250=CARTESIAN_POINT('Ctrl Pts',(2.0143853402445,-4.48747961276533,15.6950525320857));
#26251=CARTESIAN_POINT('Ctrl Pts',(2.08503515713005,-4.45509261122537,15.6994888398838));
#26252=CARTESIAN_POINT('Ctrl Pts',(2.18672109186782,-4.40552925153686,15.7059222591322));
#26253=CARTESIAN_POINT('Ctrl Pts',(2.21838552095762,-4.38967001522657,15.7079325094514));
#26254=CARTESIAN_POINT('Ctrl Pts',(2.28909508573001,-4.35329437694503,15.7124356598538));
#26255=CARTESIAN_POINT('Ctrl Pts',(2.32804116160241,-4.33259190966291,15.7149259578911));
#26256=CARTESIAN_POINT('Ctrl Pts',(2.41455409409214,-4.2851010728453,15.7204871184703));
#26257=CARTESIAN_POINT('Ctrl Pts',(2.46196408668838,-4.25803893694308,15.7235549349799));
#26258=CARTESIAN_POINT('Ctrl Pts',(2.63003253349694,-4.15835807641385,15.734522543836));
#26259=CARTESIAN_POINT('Ctrl Pts',(2.74801020215947,-4.08135432525978,15.7423962010869));
#26260=CARTESIAN_POINT('Ctrl Pts',(2.95670166819914,-3.93198578830688,15.7567884762859));
#26261=CARTESIAN_POINT('Ctrl Pts',(3.04847089222512,-3.86127203462677,15.7632945543163));
#26262=CARTESIAN_POINT('Ctrl Pts',(3.19071832002026,-3.74342723460587,15.7737156669957));
#26263=CARTESIAN_POINT('Ctrl Pts',(3.2428492033759,-3.69835906323116,15.7776113691402));
#26264=CARTESIAN_POINT('Ctrl Pts',(3.35349425194547,-3.59856567043365,15.7860569344498));
#26265=CARTESIAN_POINT('Ctrl Pts',(3.41165303401627,-3.54347596879543,15.7906090578309));
#26266=CARTESIAN_POINT('Ctrl Pts',(3.58243005550648,-3.37360749458785,15.8043334953769));
#26267=CARTESIAN_POINT('Ctrl Pts',(3.6907908299207,-3.25470348638313,15.8135355739758));
#26268=CARTESIAN_POINT('Ctrl Pts',(3.86246463666822,-3.04670533583653,15.8289727572797));
#26269=CARTESIAN_POINT('Ctrl Pts',(3.92898810858171,-2.96042215141192,15.8352023341882));
#26270=CARTESIAN_POINT('Ctrl Pts',(4.01719555139649,-2.83779811045146,15.8438006088084));
#26271=CARTESIAN_POINT('Ctrl Pts',(4.04135843959987,-2.80328026305817,15.8461940105383));
#26272=CARTESIAN_POINT('Ctrl Pts',(4.08903458912901,-2.733274770066,15.8509919695881));
#26273=CARTESIAN_POINT('Ctrl Pts',(4.11253665094254,-2.6977837554911,15.8533962169968));
#26274=CARTESIAN_POINT('Ctrl Pts',(4.19486897770873,-2.56987520200002,15.8619709286034));
#26275=CARTESIAN_POINT('Ctrl Pts',(4.25106905789913,-2.47580222080044,15.8681123108124));
#26276=CARTESIAN_POINT('Ctrl Pts',(4.39529968355737,-2.21496251478525,15.8848132716383));
#26277=CARTESIAN_POINT('Ctrl Pts',(4.47695752579596,-2.04488839144273,15.8953578798361));
#26278=CARTESIAN_POINT('Ctrl Pts',(4.57591083515631,-1.8042616788985,15.9100200634002));
#26279=CARTESIAN_POINT('Ctrl Pts',(4.60171786414726,-1.73738675011734,15.9140678863104));
#26280=CARTESIAN_POINT('Ctrl Pts',(4.65110125234697,-1.60058794024769,15.9223035262967));
#26281=CARTESIAN_POINT('Ctrl Pts',(4.67458411911539,-1.53064945490793,15.9264909433591));
#26282=CARTESIAN_POINT('Ctrl Pts',(4.72047378807687,-1.38305413975603,15.9352867638508));
#26283=CARTESIAN_POINT('Ctrl Pts',(4.74255756535897,-1.3053195374849,15.9398959508243));
#26284=CARTESIAN_POINT('Ctrl Pts',(4.80534587506586,-1.06161605077907,15.9542780411933));
#26285=CARTESIAN_POINT('Ctrl Pts',(4.83932417531062,-0.894046472751399,
15.9640738624175));
#26286=CARTESIAN_POINT('Ctrl Pts',(4.8735909931958,-0.664142973584231,15.9773450401738));
#26287=CARTESIAN_POINT('Ctrl Pts',(4.88152441693511,-0.603070938608932,
15.9808539082257));
#26288=CARTESIAN_POINT('Ctrl Pts',(4.89239866330379,-0.504971558861152,
15.9864584760367));
#26289=CARTESIAN_POINT('Ctrl Pts',(4.89607053501034,-0.468032385667622,
15.9885613412932));
#26290=CARTESIAN_POINT('Ctrl Pts',(4.90466492962352,-0.370349364947041,
15.9941036103659));
#26291=CARTESIAN_POINT('Ctrl Pts',(4.90887726347913,-0.309549463126548,
15.9975352377085));
#26292=CARTESIAN_POINT('Ctrl Pts',(4.92007393286105,-0.0883972189620109,
16.0099800895553));
#26293=CARTESIAN_POINT('Ctrl Pts',(4.92033841521507,0.0721939115846496,
16.0189488196257));
#26294=CARTESIAN_POINT('Ctrl Pts',(4.9072628802798,0.348468797282983,16.0344585550179));
#26295=CARTESIAN_POINT('Ctrl Pts',(4.89767106532848,0.464195142065669,16.0409789490285));
#26296=CARTESIAN_POINT('Ctrl Pts',(4.87584682986917,0.648137322021266,16.0514275529925));
#26297=CARTESIAN_POINT('Ctrl Pts',(4.86625284933039,0.716622187511607,16.0553364248338));
#26298=CARTESIAN_POINT('Ctrl Pts',(4.84258948784879,0.863001978962626,16.0637401463363));
#26299=CARTESIAN_POINT('Ctrl Pts',(4.82807724816486,0.940805633373073,16.0682368995086));
#26300=CARTESIAN_POINT('Ctrl Pts',(4.75927755919565,1.2659235725187,16.0871685825962));
#26301=CARTESIAN_POINT('Ctrl Pts',(4.68781299996906,1.50920270665969,16.1017021244908));
#26302=CARTESIAN_POINT('Ctrl Pts',(4.57989217346329,1.79341993720486,16.1190363631025));
#26303=CARTESIAN_POINT('Ctrl Pts',(4.56111023762814,1.84066316217621,16.1219290363049));
#26304=CARTESIAN_POINT('Ctrl Pts',(4.52701154763958,1.92270490866688,16.126968888265));
#26305=CARTESIAN_POINT('Ctrl Pts',(4.51201765572754,1.95763235060485,16.1291193650016));
#26306=CARTESIAN_POINT('Ctrl Pts',(4.46414217061016,2.06568280218006,16.1357917419951));
#26307=CARTESIAN_POINT('Ctrl Pts',(4.42987634105798,2.13817834113984,16.1402977371673));
#26308=CARTESIAN_POINT('Ctrl Pts',(4.33651308950098,2.32381668509506,16.1519569010382));
#26309=CARTESIAN_POINT('Ctrl Pts',(4.27475685666113,2.43555408431862,16.1590949877117));
#26310=CARTESIAN_POINT('Ctrl Pts',(4.15208084351505,2.63844511184313,16.1723886385792));
#26311=CARTESIAN_POINT('Ctrl Pts',(4.09232529351868,2.73020901066254,16.1785356288839));
#26312=CARTESIAN_POINT('Ctrl Pts',(3.99294446486412,2.87222134831729,16.1883061347029));
#26313=CARTESIAN_POINT('Ctrl Pts',(3.95531564077455,2.9238226765734,16.1919127672559));
#26314=CARTESIAN_POINT('Ctrl Pts',(3.87281408773291,3.03245071618966,16.1996348579622));
#26315=CARTESIAN_POINT('Ctrl Pts',(3.82766259158011,3.08924670808085,16.2037518540514));
#26316=CARTESIAN_POINT('Ctrl Pts',(3.75536082003134,3.17617537883206,16.2101841428276));
#26317=CARTESIAN_POINT('Ctrl Pts',(3.72906607709961,3.20700656263263,16.2124921725685));
#26318=CARTESIAN_POINT('Ctrl Pts',(3.57852526645503,3.37916400938806,16.2255336669809));
#26319=CARTESIAN_POINT('Ctrl Pts',(3.44662999478166,3.51359263992373,16.2363179473873));
#26320=CARTESIAN_POINT('Ctrl Pts',(3.25092111880429,3.69141025697158,16.2514368860352));
#26321=CARTESIAN_POINT('Ctrl Pts',(3.19329766425957,3.74136980701012,16.2557896868606));
#26322=CARTESIAN_POINT('Ctrl Pts',(3.10739882921164,3.81241336888809,16.2621286920996));
#26323=CARTESIAN_POINT('Ctrl Pts',(3.0800216708668,3.83456512910313,16.2641275597924));
#26324=CARTESIAN_POINT('Ctrl Pts',(3.01747302870874,3.88407321297097,16.2686446926175));
#26325=CARTESIAN_POINT('Ctrl Pts',(2.98216290201278,3.91124950521013,16.2711601899426));
#26326=CARTESIAN_POINT('Ctrl Pts',(2.90209662525436,3.97115752468188,16.2767944459938));
#26327=CARTESIAN_POINT('Ctrl Pts',(2.8571463767045,4.00361980805408,16.2799100303992));
#26328=CARTESIAN_POINT('Ctrl Pts',(2.69131544716929,4.11916459078317,16.2912531348665));
#26329=CARTESIAN_POINT('Ctrl Pts',(2.56728351967133,4.19758874222412,16.2994528432359));
#26330=CARTESIAN_POINT('Ctrl Pts',(2.34376594762202,4.32529899085836,16.3138932853996));
#26331=CARTESIAN_POINT('Ctrl Pts',(2.24577168014551,4.37698061405129,16.3201173327044));
#26332=CARTESIAN_POINT('Ctrl Pts',(2.08437675005714,4.45525140051145,16.3302385459353));
#26333=CARTESIAN_POINT('Ctrl Pts',(2.02201684702941,4.48389776952965,16.3341187629346));
#26334=CARTESIAN_POINT('Ctrl Pts',(1.8843220364278,4.54369409019706,16.3426291220493));
#26335=CARTESIAN_POINT('Ctrl Pts',(1.80877082889211,4.57429485104697,16.3472620295794));
#26336=CARTESIAN_POINT('Ctrl Pts',(1.58235888337296,4.65951257839769,16.3610490374727));
#26337=CARTESIAN_POINT('Ctrl Pts',(1.42954923481427,4.70864154935364,16.37023178492));
#26338=CARTESIAN_POINT('Ctrl Pts',(1.17025626710656,4.7782170357044,16.385597916378));
#26339=CARTESIAN_POINT('Ctrl Pts',(1.06500290883647,4.80277284323968,16.3917767760565));
#26340=CARTESIAN_POINT('Ctrl Pts',(0.91864851863792,4.83186948335065,16.400268478949));
#26341=CARTESIAN_POINT('Ctrl Pts',(0.878171926498472,4.83938962410504,16.4026064539316));
#26342=CARTESIAN_POINT('Ctrl Pts',(0.804813406509809,4.85206820583883,16.4068227350261));
#26343=CARTESIAN_POINT('Ctrl Pts',(0.771964585679908,4.85740272158678,16.4087032539633));
#26344=CARTESIAN_POINT('Ctrl Pts',(0.693052811795507,4.86939696443003,16.4132060363756));
#26345=CARTESIAN_POINT('Ctrl Pts',(0.646944421803848,4.87573706904295,16.4158250411155));
#26346=CARTESIAN_POINT('Ctrl Pts',(0.504869292626538,4.89322214301878,16.4238686767958));
#26347=CARTESIAN_POINT('Ctrl Pts',(0.408658490960322,4.9021948525179,16.4292791304113));
#26348=CARTESIAN_POINT('Ctrl Pts',(0.156016665095246,4.9182667785227,16.443460878629));
#26349=CARTESIAN_POINT('Ctrl Pts',(-0.000596170775789447,4.9207406136419,
16.4522286612861));
#26350=CARTESIAN_POINT('Ctrl Pts',(-0.228838237714226,4.91344824948127,
16.4650928524501));
#26351=CARTESIAN_POINT('Ctrl Pts',(-0.300558463776009,4.90958298568872,
16.4691470686148));
#26352=CARTESIAN_POINT('Ctrl Pts',(-0.435830583027537,4.89931740790259,
16.4768258812867));
#26353=CARTESIAN_POINT('Ctrl Pts',(-0.499392842118374,4.89324698291994,
16.4804474715297));
#26354=CARTESIAN_POINT('Ctrl Pts',(-0.635825294570917,4.87753113609829,
16.4882548990247));
#26355=CARTESIAN_POINT('Ctrl Pts',(-0.708633967692077,4.86748616222254,
16.4924423925208));
#26356=CARTESIAN_POINT('Ctrl Pts',(-0.915856476843084,4.83414878672588,
16.504425014285));
#26357=CARTESIAN_POINT('Ctrl Pts',(-1.04956320196758,4.80689133539,16.5122360962206));
#26358=CARTESIAN_POINT('Ctrl Pts',(-1.27845798040773,4.75022212984519,16.5257307199666));
#26359=CARTESIAN_POINT('Ctrl Pts',(-1.3742074236622,4.7234118381211,16.5314132189931));
#26360=CARTESIAN_POINT('Ctrl Pts',(-1.50812317232462,4.68149776540023,16.5393980527388));
#26361=CARTESIAN_POINT('Ctrl Pts',(-1.54701351207227,4.66879064493385,16.5417213444778));
#26362=CARTESIAN_POINT('Ctrl Pts',(-1.61733021741208,4.64484011230029,16.5459281650604));
#26363=CARTESIAN_POINT('Ctrl Pts',(-1.64880918460329,4.63375927317048,16.5478138303745));
#26364=CARTESIAN_POINT('Ctrl Pts',(-1.72424316887052,4.60633990630413,16.5523414308717));
#26365=CARTESIAN_POINT('Ctrl Pts',(-1.76808215225237,4.58969142707244,16.5549800415298));
#26366=CARTESIAN_POINT('Ctrl Pts',(-1.90298793269132,4.53623926683041,16.5631334486788));
#26367=CARTESIAN_POINT('Ctrl Pts',(-1.99319548371995,4.49733273347707,16.5686336625195));
#26368=CARTESIAN_POINT('Ctrl Pts',(-2.22112832413141,4.39081944415703,16.5827279988945));
#26369=CARTESIAN_POINT('Ctrl Pts',(-2.35696414470608,4.31942423390621,16.5913191375308));
#26370=CARTESIAN_POINT('Ctrl Pts',(-2.55131572875492,4.20537173537503,16.6040130836264));
#26371=CARTESIAN_POINT('Ctrl Pts',(-2.61258326118298,4.16758586320101,16.6080760674647));
#26372=CARTESIAN_POINT('Ctrl Pts',(-2.72662504582345,4.09374891572072,16.6157657741928));
#26373=CARTESIAN_POINT('Ctrl Pts',(-2.77956911217855,4.05798715645921,16.6193894513888));
#26374=CARTESIAN_POINT('Ctrl Pts',(-2.89174462314117,3.97899123865249,16.6271889694607));
#26375=CARTESIAN_POINT('Ctrl Pts',(-2.95073629188274,3.93544323171193,16.6313664136608));
#26376=CARTESIAN_POINT('Ctrl Pts',(-3.11583855531148,3.80776386669652,16.6432816121659));
#26377=CARTESIAN_POINT('Ctrl Pts',(-3.21947860345625,3.72054737041113,16.6510350791738));
#26378=CARTESIAN_POINT('Ctrl Pts',(-3.39408055564127,3.56084914488801,16.664576788578));
#26379=CARTESIAN_POINT('Ctrl Pts',(-3.46664763810893,3.49024124729134,16.6703634733672));
#26380=CARTESIAN_POINT('Ctrl Pts',(-3.56536507833701,3.3880707126168,16.678447641838));
#26381=CARTESIAN_POINT('Ctrl Pts',(-3.59337878763188,3.35834486715548,16.6807670427508));
#26382=CARTESIAN_POINT('Ctrl Pts',(-3.64361961303344,3.30368499378094,16.6849714183618));
#26383=CARTESIAN_POINT('Ctrl Pts',(-3.66596911359085,3.2788670160264,16.6868585089227));
#26384=CARTESIAN_POINT('Ctrl Pts',(-3.71915048020074,3.21858829610938,16.6913929455595));
#26385=CARTESIAN_POINT('Ctrl Pts',(-3.74973039223268,3.18290951097868,16.6940369490131));
#26386=CARTESIAN_POINT('Ctrl Pts',(-3.84292225891082,3.07097155732226,16.7022207793294));
#26387=CARTESIAN_POINT('Ctrl Pts',(-3.90375430148599,2.99326249140501,16.7077459105216));
#26388=CARTESIAN_POINT('Ctrl Pts',(-4.05256254632287,2.79091021575616,16.7218170709338));
#26389=CARTESIAN_POINT('Ctrl Pts',(-4.1371523699694,2.66390926434112,16.7303602423759));
#26390=CARTESIAN_POINT('Ctrl Pts',(-4.25279560296228,2.47145680855265,16.7430078317623));
#26391=CARTESIAN_POINT('Ctrl Pts',(-4.28852688842939,2.40892220036228,16.7470730553598));
#26392=CARTESIAN_POINT('Ctrl Pts',(-4.35334480409,2.28946601436645,16.7547655542114));
#26393=CARTESIAN_POINT('Ctrl Pts',(-4.3827202092115,2.23271786570329,16.7583897737235));
#26394=CARTESIAN_POINT('Ctrl Pts',(-4.44339073612706,2.10969917772394,16.7661873305752));
#26395=CARTESIAN_POINT('Ctrl Pts',(-4.47432722370128,2.04326885194887,16.7703622578942));
#26396=CARTESIAN_POINT('Ctrl Pts',(-4.55807085702216,1.85241413428989,16.7822606351142));
#26397=CARTESIAN_POINT('Ctrl Pts',(-4.60724946439388,1.72647041144817,16.7899997377937));
#26398=CARTESIAN_POINT('Ctrl Pts',(-4.68417348698489,1.50266621206,16.8035435174551));
#26399=CARTESIAN_POINT('Ctrl Pts',(-4.71418893700768,1.40567066878571,16.8093465351146));
#26400=CARTESIAN_POINT('Ctrl Pts',(-4.74905764439672,1.2792622310191,16.8168082304702));
#26401=CARTESIAN_POINT('Ctrl Pts',(-4.75667563174419,1.25063875536686,16.8184911850632));
#26402=CARTESIAN_POINT('Ctrl Pts',(-4.76403458706411,1.22194824594044,16.8201710428097));
#26403=CARTESIAN_POINT('Origin',(0.,0.,-3.23514056400928));
#26404=CARTESIAN_POINT('',(-4.76403456361785,1.22194833735086,18.9152905258446));
#26405=CARTESIAN_POINT('',(-4.76403458707798,1.22194824588636,18.5697043142649));
#26406=CARTESIAN_POINT('',(-4.76403458704967,1.22194824599672,-3.23514056400928));
#26407=CARTESIAN_POINT('Ctrl Pts',(-4.76403456361784,1.22194833735086,18.9152905258446));
#26408=CARTESIAN_POINT('Ctrl Pts',(-4.74331547396517,1.30272626896624,18.9105214132134));
#26409=CARTESIAN_POINT('Ctrl Pts',(-4.72054074812226,1.38298175666518,18.9057455795195));
#26410=CARTESIAN_POINT('Ctrl Pts',(-4.67259489281969,1.53690982447573,18.8965178438601));
#26411=CARTESIAN_POINT('Ctrl Pts',(-4.6477009457191,1.61062437622381,18.8920680814749));
#26412=CARTESIAN_POINT('Ctrl Pts',(-4.60234199617997,1.73511486013049,18.8845088175739));
#26413=CARTESIAN_POINT('Ctrl Pts',(-4.58275874947153,1.78619645364731,18.8813941071591));
#26414=CARTESIAN_POINT('Ctrl Pts',(-4.56084535866196,1.84062174824491,18.8780640956766));
#26415=CARTESIAN_POINT('Ctrl Pts',(-4.55935896037133,1.84430059271013,18.8778389494523));
#26416=CARTESIAN_POINT('Ctrl Pts',(-4.55577765380504,1.85313355836085,18.8772982372327));
#26417=CARTESIAN_POINT('Ctrl Pts',(-4.55367844734684,1.85828593449496,18.8769827247596));
#26418=CARTESIAN_POINT('Ctrl Pts',(-4.54880708197402,1.8701845872421,18.8762538510388));
#26419=CARTESIAN_POINT('Ctrl Pts',(-4.54602864822168,1.87692828562131,18.8758405728594));
#26420=CARTESIAN_POINT('Ctrl Pts',(-4.52668380042765,1.92358634667714,18.8729799660891));
#26421=CARTESIAN_POINT('Ctrl Pts',(-4.50960680919958,1.96328733180964,18.8705395254828));
#26422=CARTESIAN_POINT('Ctrl Pts',(-4.4323985011956,2.13645868988737,18.859853968443));
#26423=CARTESIAN_POINT('Ctrl Pts',(-4.36684822964812,2.26743239048121,18.8516633598902));
#26424=CARTESIAN_POINT('Ctrl Pts',(-4.24397687663926,2.48778185527467,18.8375288983511));
#26425=CARTESIAN_POINT('Ctrl Pts',(-4.1894267834232,2.57858513362137,18.8315944357521));
#26426=CARTESIAN_POINT('Ctrl Pts',(-4.0864211867594,2.73813863991214,18.8209185600211));
#26427=CARTESIAN_POINT('Ctrl Pts',(-4.03905337544367,2.80754143841542,18.816185992228));
#26428=CARTESIAN_POINT('Ctrl Pts',(-3.98492200464019,2.88264688888495,18.8109547034095));
#26429=CARTESIAN_POINT('Ctrl Pts',(-3.97989429229864,2.88958438030849,18.8104704363744));
#26430=CARTESIAN_POINT('Ctrl Pts',(-3.97132223061989,2.90134773059473,18.8096474979743));
#26431=CARTESIAN_POINT('Ctrl Pts',(-3.96778714744651,2.90618032229719,18.8093089003546));
#26432=CARTESIAN_POINT('Ctrl Pts',(-3.96028652085849,2.91639476493261,18.808592113452));
#26433=CARTESIAN_POINT('Ctrl Pts',(-3.95631881224679,2.92177500981004,18.8082139076738));
#26434=CARTESIAN_POINT('Ctrl Pts',(-3.94637763523444,2.93519794726404,18.807268695356));
#26435=CARTESIAN_POINT('Ctrl Pts',(-3.94039054269775,2.94323050406777,18.8067015819093));
#26436=CARTESIAN_POINT('Ctrl Pts',(-3.92175019846475,2.96808041841473,18.8049424998919));
#26437=CARTESIAN_POINT('Ctrl Pts',(-3.90901353788586,2.98483486073109,18.803749873941));
#26438=CARTESIAN_POINT('Ctrl Pts',(-3.84500654484156,3.06792049441307,18.7978020625483));
#26439=CARTESIAN_POINT('Ctrl Pts',(-3.79215405127514,3.13301434695902,18.79303457245));
#26440=CARTESIAN_POINT('Ctrl Pts',(-3.61644844325143,3.33845227855855,18.7776223797244));
#26441=CARTESIAN_POINT('Ctrl Pts',(-3.48727028426456,3.47316972420027,18.7669363710144));
#26442=CARTESIAN_POINT('Ctrl Pts',(-3.30668401638911,3.64124275027415,18.7528282260749));
#26443=CARTESIAN_POINT('Ctrl Pts',(-3.26186191996734,3.68144874324259,18.749389119728));
#26444=CARTESIAN_POINT('Ctrl Pts',(-3.20734839953662,3.72857073295407,18.7452831735555));
#26445=CARTESIAN_POINT('Ctrl Pts',(-3.19835607152841,3.73628718212743,18.7446083207139));
#26446=CARTESIAN_POINT('Ctrl Pts',(-3.15849923618768,3.77023959109998,18.7416280449013));
#26447=CARTESIAN_POINT('Ctrl Pts',(-3.1273389504335,3.79612633309031,18.7393267383424));
#26448=CARTESIAN_POINT('Ctrl Pts',(-3.06391563619396,3.84750495440327,18.7347020173427));
#26449=CARTESIAN_POINT('Ctrl Pts',(-3.03164559625151,3.87298314280356,18.7323790773355));
#26450=CARTESIAN_POINT('Ctrl Pts',(-2.83739336582278,4.02243567776609,18.7185591414124));
#26451=CARTESIAN_POINT('Ctrl Pts',(-2.66814404746926,4.13664104667713,18.7071771348875));
#26452=CARTESIAN_POINT('Ctrl Pts',(-2.42070239545599,4.2820881300412,18.6910796324424));
#26453=CARTESIAN_POINT('Ctrl Pts',(-2.34805937958714,4.32234841519318,18.6864165131972));
#26454=CARTESIAN_POINT('Ctrl Pts',(-2.21036581048511,4.39416512528423,18.6776722299491));
#26455=CARTESIAN_POINT('Ctrl Pts',(-2.14557111528362,4.42616409519408,18.6735952422316));
#26456=CARTESIAN_POINT('Ctrl Pts',(-2.03375504054126,4.47835223370126,18.6666142786657));
#26457=CARTESIAN_POINT('Ctrl Pts',(-1.98708035219212,4.49925659514901,18.663716171536));
#26458=CARTESIAN_POINT('Ctrl Pts',(-1.84899445025305,4.55853374101028,18.6551847448496));
#26459=CARTESIAN_POINT('Ctrl Pts',(-1.75673991932869,4.59487484331288,18.6495385595352));
#26460=CARTESIAN_POINT('Ctrl Pts',(-1.51187559547353,4.68287925285433,18.6346799291894));
#26461=CARTESIAN_POINT('Ctrl Pts',(-1.35771565104458,4.72987671766496,18.6254498601078));
#26462=CARTESIAN_POINT('Ctrl Pts',(-1.1460382011886,4.78320543242144,18.6129692926602));
#26463=CARTESIAN_POINT('Ctrl Pts',(-1.09030700296731,4.7962160588261,18.6097015638274));
#26464=CARTESIAN_POINT('Ctrl Pts',(-1.03008590310075,4.80917094919228,18.6061925521158));
#26465=CARTESIAN_POINT('Ctrl Pts',(-1.02580940221503,4.81008495316844,18.6059434846124));
#26466=CARTESIAN_POINT('Ctrl Pts',(-1.01791645631458,4.81176088449988,18.60548401379));
#26467=CARTESIAN_POINT('Ctrl Pts',(-1.01430036120518,4.81252444138505,18.6052735964848));
#26468=CARTESIAN_POINT('Ctrl Pts',(-0.973546885426587,4.82108177197463,
18.6029031641354));
#26469=CARTESIAN_POINT('Ctrl Pts',(-0.936321102980405,4.8284496291812,18.6007470353921));
#26470=CARTESIAN_POINT('Ctrl Pts',(-0.873978816667656,4.8400405466355,18.5971527857277));
#26471=CARTESIAN_POINT('Ctrl Pts',(-0.84890835220697,4.84450060201537,18.595711964562));
#26472=CARTESIAN_POINT('Ctrl Pts',(-0.75974656572301,4.85964916895445,18.5906021171547));
#26473=CARTESIAN_POINT('Ctrl Pts',(-0.695478952343455,4.86926216912934,
18.5869450359429));
#26474=CARTESIAN_POINT('Ctrl Pts',(-0.46170684271573,4.89950642840237,18.5737031774756));
#26475=CARTESIAN_POINT('Ctrl Pts',(-0.291348085244922,4.9125811092282,18.5641647883729));
#26476=CARTESIAN_POINT('Ctrl Pts',(-0.0157370415834658,4.91934444192025,
18.5486954685866));
#26477=CARTESIAN_POINT('Ctrl Pts',(0.0892350633911437,4.91856016626208,
18.5427958008881));
#26478=CARTESIAN_POINT('Ctrl Pts',(0.260461738125204,4.91179737069259,18.5331257181379));
#26479=CARTESIAN_POINT('Ctrl Pts',(0.326762435415399,4.90783250641799,18.529370049241));
#26480=CARTESIAN_POINT('Ctrl Pts',(0.472998047124371,4.8961109909255,18.5210536235431));
#26481=CARTESIAN_POINT('Ctrl Pts',(0.552864285732227,4.88773678226556,18.5164898330699));
#26482=CARTESIAN_POINT('Ctrl Pts',(0.824786360210946,4.85247469201418,18.500864979913));
#26483=CARTESIAN_POINT('Ctrl Pts',(1.01543957466489,4.81618774613089,18.4897549361265));
#26484=CARTESIAN_POINT('Ctrl Pts',(1.24466147200319,4.75834083312858,18.4762344179359));
#26485=CARTESIAN_POINT('Ctrl Pts',(1.28573712979467,4.74740663127209,18.4738054610475));
#26486=CARTESIAN_POINT('Ctrl Pts',(1.3531652380119,4.72851818362406,18.4698094694641));
#26487=CARTESIAN_POINT('Ctrl Pts',(1.37960178212249,4.72087272733882,18.4682405394414));
#26488=CARTESIAN_POINT('Ctrl Pts',(1.44748601296393,4.70062166242236,18.4642068063837));
#26489=CARTESIAN_POINT('Ctrl Pts',(1.48883406622992,4.68768951107477,18.461745031288));
#26490=CARTESIAN_POINT('Ctrl Pts',(1.5634335450985,4.66327092548179,18.4572970454119));
#26491=CARTESIAN_POINT('Ctrl Pts',(1.59674276797096,4.65197084403027,18.4553087456745));
#26492=CARTESIAN_POINT('Ctrl Pts',(1.70303869251309,4.61463399606859,18.4489516084091));
#26493=CARTESIAN_POINT('Ctrl Pts',(1.77553287830717,4.58722911197688,18.4445974415642));
#26494=CARTESIAN_POINT('Ctrl Pts',(2.01205070919356,4.49137140570089,18.4302796294759));
#26495=CARTESIAN_POINT('Ctrl Pts',(2.1730122675289,4.41574260694886,18.4203507765915));
#26496=CARTESIAN_POINT('Ctrl Pts',(2.40802001438941,4.28935494795731,18.4053577676388));
#26497=CARTESIAN_POINT('Ctrl Pts',(2.48535059699469,4.24501571294973,18.4003396591303));
#26498=CARTESIAN_POINT('Ctrl Pts',(2.6188505417372,4.16357162525271,18.3915056740083));
#26499=CARTESIAN_POINT('Ctrl Pts',(2.67554303374626,4.1273691595809,18.3876978955025));
#26500=CARTESIAN_POINT('Ctrl Pts',(2.80870470490234,4.03843851125573,18.3786104040157));
#26501=CARTESIAN_POINT('Ctrl Pts',(2.8844575039534,3.98468472016957,18.3733239310374));
#26502=CARTESIAN_POINT('Ctrl Pts',(3.06187679492681,3.85107708833363,18.3606481070797));
#26503=CARTESIAN_POINT('Ctrl Pts',(3.16200656322906,3.76929680170268,18.3532500156859));
#26504=CARTESIAN_POINT('Ctrl Pts',(3.31872804282334,3.63065140726908,18.3412729665813));
#26505=CARTESIAN_POINT('Ctrl Pts',(3.37735521158827,3.57617915700307,18.3366955264814));
#26506=CARTESIAN_POINT('Ctrl Pts',(3.4539620199916,3.50143671904021,18.3305885758325));
#26507=CARTESIAN_POINT('Ctrl Pts',(3.47314083462827,3.48241374425074,18.3290487354499));
#26508=CARTESIAN_POINT('Ctrl Pts',(3.52230078270599,3.43284316368129,18.3250739371256));
#26509=CARTESIAN_POINT('Ctrl Pts',(3.55204178645288,3.40206028665405,18.3226419928334));
#26510=CARTESIAN_POINT('Ctrl Pts',(3.60566526651638,3.34508846188033,18.3182089382677));
#26511=CARTESIAN_POINT('Ctrl Pts',(3.6296736743275,3.31902212690641,18.3162059213692));
#26512=CARTESIAN_POINT('Ctrl Pts',(3.70718304469727,3.23302196203446,18.3096738867691));
#26513=CARTESIAN_POINT('Ctrl Pts',(3.75949794688644,3.17203602794524,18.3051607434742));
#26514=CARTESIAN_POINT('Ctrl Pts',(3.90592101805128,2.99263026832876,18.2921708848987));
#26515=CARTESIAN_POINT('Ctrl Pts',(3.99609099271128,2.87111680554166,18.2837160468752));
#26516=CARTESIAN_POINT('Ctrl Pts',(4.10717053216583,2.70603261900159,18.2725475403385));
#26517=CARTESIAN_POINT('Ctrl Pts',(4.13324426754204,2.66603715400445,18.2698652807778));
#26518=CARTESIAN_POINT('Ctrl Pts',(4.20082947598973,2.55899061532629,18.2627426117146));
#26519=CARTESIAN_POINT('Ctrl Pts',(4.24131742945594,2.49131040234965,18.2582965546766));
#26520=CARTESIAN_POINT('Ctrl Pts',(4.31382091614593,2.36321849553766,18.2499735081212));
#26521=CARTESIAN_POINT('Ctrl Pts',(4.34623819659401,2.30305578580205,18.2461006861971));
#26522=CARTESIAN_POINT('Ctrl Pts',(4.42995226050839,2.13962565086336,18.2356685670212));
#26523=CARTESIAN_POINT('Ctrl Pts',(4.47888849303855,2.03519833781208,18.2290945535841));
#26524=CARTESIAN_POINT('Ctrl Pts',(4.57932783599482,1.79965482994503,18.2144561737728));
#26525=CARTESIAN_POINT('Ctrl Pts',(4.62896087317258,1.6678495450905,18.2063895953891));
#26526=CARTESIAN_POINT('Ctrl Pts',(4.68984673460836,1.48239076888442,18.1952324246198));
#26527=CARTESIAN_POINT('Ctrl Pts',(4.70596263479696,1.43040572405521,18.1921258050919));
#26528=CARTESIAN_POINT('Ctrl Pts',(4.73352063901732,1.33599952324321,18.1865251339607));
#26529=CARTESIAN_POINT('Ctrl Pts',(4.74526343128659,1.29367205803261,18.1840287758328));
#26530=CARTESIAN_POINT('Ctrl Pts',(4.76531565313282,1.21744307507194,18.1795617109125));
#26531=CARTESIAN_POINT('Ctrl Pts',(4.77383411874656,1.18359990946682,18.1775887127222));
#26532=CARTESIAN_POINT('Ctrl Pts',(4.79963766521207,1.07627129349993,18.1713592553093));
#26533=CARTESIAN_POINT('Ctrl Pts',(4.81559158360528,1.00247669492993,18.1671167038135));
#26534=CARTESIAN_POINT('Ctrl Pts',(4.86546509040271,0.74300260833375,18.1522907914608));
#26535=CARTESIAN_POINT('Ctrl Pts',(4.89039143466943,0.555765186730222,18.141749493902));
#26536=CARTESIAN_POINT('Ctrl Pts',(4.90750993087085,0.327346215257011,18.1288740250851));
#26537=CARTESIAN_POINT('Ctrl Pts',(4.91002895502809,0.287097376274816,18.1266049962327));
#26538=CARTESIAN_POINT('Ctrl Pts',(4.91566931740542,0.174847546183887,18.1202728968596));
#26539=CARTESIAN_POINT('Ctrl Pts',(4.91770352577797,0.102802612872553,18.1162040803201));
#26540=CARTESIAN_POINT('Ctrl Pts',(4.91854814053675,-0.0323307908643089,
18.108553928296));
#26541=CARTESIAN_POINT('Ctrl Pts',(4.91772908478377,-0.0954024630838392,
18.1049758597525));
#26542=CARTESIAN_POINT('Ctrl Pts',(4.91144360896867,-0.29041258890819,18.0938830156863));
#26543=CARTESIAN_POINT('Ctrl Pts',(4.90187712319243,-0.422158403298321,
18.0863450969728));
#26544=CARTESIAN_POINT('Ctrl Pts',(4.87016907421694,-0.702190421400551,
18.0702208916673));
#26545=CARTESIAN_POINT('Ctrl Pts',(4.84652652849525,-0.850175949269935,
18.0616376116439));
#26546=CARTESIAN_POINT('Ctrl Pts',(4.81106144783633,-1.02152114834946,18.0516583772163));
#26547=CARTESIAN_POINT('Ctrl Pts',(4.80576589326066,-1.04615099265636,18.0502229965166));
#26548=CARTESIAN_POINT('Ctrl Pts',(4.79137211451767,-1.11068042316063,18.0464604968913));
#26549=CARTESIAN_POINT('Ctrl Pts',(4.78196467346111,-1.15050930574099,18.04413634206));
#26550=CARTESIAN_POINT('Ctrl Pts',(4.76167176661313,-1.23187181011136,18.039386944299));
#26551=CARTESIAN_POINT('Ctrl Pts',(4.75073731035936,-1.27338966353862,18.0369623998446));
#26552=CARTESIAN_POINT('Ctrl Pts',(4.70694968965091,-1.43122915536108,18.0277304060125));
#26553=CARTESIAN_POINT('Ctrl Pts',(4.67035597288275,-1.54646951223147,18.0209588269278));
#26554=CARTESIAN_POINT('Ctrl Pts',(4.5713079954746,-1.82266235687388,18.0045203401299));
#26555=CARTESIAN_POINT('Ctrl Pts',(4.50455618028888,-1.98189998903594,17.9948621162993));
#26556=CARTESIAN_POINT('Ctrl Pts',(4.39840505843221,-2.20189937047227,17.9810987840984));
#26557=CARTESIAN_POINT('Ctrl Pts',(4.36582559194621,-2.26580993034484,17.9770486861306));
#26558=CARTESIAN_POINT('Ctrl Pts',(4.30188458165883,-2.38473880885627,17.9694040638177));
#26559=CARTESIAN_POINT('Ctrl Pts',(4.27083545710979,-2.43990871305937,17.9658126475643));
#26560=CARTESIAN_POINT('Ctrl Pts',(4.13969760851285,-2.66274539497912,17.9511112104505));
#26561=CARTESIAN_POINT('Ctrl Pts',(4.03073247449989,-2.82497842561231,17.9399400865834));
#26562=CARTESIAN_POINT('Ctrl Pts',(3.84296214492703,-3.07147543978423,17.9222038630931));
#26563=CARTESIAN_POINT('Ctrl Pts',(3.77034326363936,-3.16019486555355,17.9156492440026));
#26564=CARTESIAN_POINT('Ctrl Pts',(3.66859948150952,-3.27599198151733,17.906880747125));
#26565=CARTESIAN_POINT('Ctrl Pts',(3.64215089276217,-3.30537177268705,17.9046367138011));
#26566=CARTESIAN_POINT('Ctrl Pts',(3.58485493361127,-3.36749483388145,17.8998519211714));
#26567=CARTESIAN_POINT('Ctrl Pts',(3.55390672259805,-3.4001402063459,17.8973127737319));
#26568=CARTESIAN_POINT('Ctrl Pts',(3.38477137782874,-3.57371824985804,17.8836595478276));
#26569=CARTESIAN_POINT('Ctrl Pts',(3.23864219654943,-3.70666125076684,17.8726437104261));
#26570=CARTESIAN_POINT('Ctrl Pts',(2.99748624658588,-3.90087966654925,17.8552760713994));
#26571=CARTESIAN_POINT('Ctrl Pts',(2.9076686646918,-3.96828028925259,17.8489682732907));
#26572=CARTESIAN_POINT('Ctrl Pts',(2.759741980571,-4.07156635191415,17.8387890463593));
#26573=CARTESIAN_POINT('Ctrl Pts',(2.70305491952036,-4.10941873285273,17.8349353588157));
#26574=CARTESIAN_POINT('Ctrl Pts',(2.57847922797815,-4.18891006080834,17.8265588309162));
#26575=CARTESIAN_POINT('Ctrl Pts',(2.51032891672712,-4.23010297089548,17.8220336571834));
#26576=CARTESIAN_POINT('Ctrl Pts',(2.20981143096148,-4.40192752907998,17.8023096676312));
#26577=CARTESIAN_POINT('Ctrl Pts',(1.96804312816243,-4.51520067131362,17.7870002676973));
#26578=CARTESIAN_POINT('Ctrl Pts',(1.67796740621951,-4.62336031206839,17.7693733263332));
#26579=CARTESIAN_POINT('Ctrl Pts',(1.63744705691092,-4.63786614560272,17.7669278800102));
#26580=CARTESIAN_POINT('Ctrl Pts',(1.56334019641478,-4.66330328921069,17.7624882526341));
#26581=CARTESIAN_POINT('Ctrl Pts',(1.52981644233962,-4.67440817830512,17.7604920822536));
#26582=CARTESIAN_POINT('Ctrl Pts',(1.42125980145311,-4.70907511160374,17.7540622424194));
#26583=CARTESIAN_POINT('Ctrl Pts',(1.34578002100625,-4.73119902290545,17.7496437052549));
#26584=CARTESIAN_POINT('Ctrl Pts',(1.09064828138368,-4.79938095386135,17.7348287658821));
#26585=CARTESIAN_POINT('Ctrl Pts',(0.908931080695871,-4.83708748441574,
17.7244695065817));
#26586=CARTESIAN_POINT('Ctrl Pts',(0.6415110163948,-4.87697254075507,17.7092703142488));
#26587=CARTESIAN_POINT('Ctrl Pts',(0.557192399668656,-4.88732380145958,
17.7044855069337));
#26588=CARTESIAN_POINT('Ctrl Pts',(0.405523652805788,-4.9019670964302,17.6958748820173));
#26589=CARTESIAN_POINT('Ctrl Pts',(0.338272845491704,-4.90706655697591,
17.6920555763784));
#26590=CARTESIAN_POINT('Ctrl Pts',(0.172236881465047,-4.91622713863244,
17.6826149510968));
#26591=CARTESIAN_POINT('Ctrl Pts',(0.0733940364577686,-4.91869573819681,
17.6769848701628));
#26592=CARTESIAN_POINT('Ctrl Pts',(-0.186919709866415,-4.91734843654965,
17.6621198124596));
#26593=CARTESIAN_POINT('Ctrl Pts',(-0.348245052206564,-4.90856187094722,
17.652866874697));
#26594=CARTESIAN_POINT('Ctrl Pts',(-0.588161850295145,-4.88360604887743,
17.6390758512608));
#26595=CARTESIAN_POINT('Ctrl Pts',(-0.667267735593434,-4.87342758288902,
17.6345243973836));
#26596=CARTESIAN_POINT('Ctrl Pts',(-0.783357993448415,-4.85561065178102,
17.6278484082831));
#26597=CARTESIAN_POINT('Ctrl Pts',(-0.820557540131678,-4.84946284958733,
17.6257098797528));
#26598=CARTESIAN_POINT('Ctrl Pts',(-0.906748443653881,-4.83419830280463,
17.6207575078797));
#26599=CARTESIAN_POINT('Ctrl Pts',(-0.955679237668195,-4.82476354321358,
17.6179472489411));
#26600=CARTESIAN_POINT('Ctrl Pts',(-1.19056360995287,-4.7757600391135,17.6044422090022));
#26601=CARTESIAN_POINT('Ctrl Pts',(-1.37426212397276,-4.72617502712813,
17.593829082158));
#26602=CARTESIAN_POINT('Ctrl Pts',(-1.65926931602333,-4.63121726488516,
17.5769773768778));
#26603=CARTESIAN_POINT('Ctrl Pts',(-1.76270571193812,-4.59284401591475,
17.5707792420145));
#26604=CARTESIAN_POINT('Ctrl Pts',(-1.92772432370149,-4.525228346797,17.560716817535));
#26605=CARTESIAN_POINT('Ctrl Pts',(-1.99014251309905,-4.49812686564716,
17.5568693643289));
#26606=CARTESIAN_POINT('Ctrl Pts',(-2.12484940903831,-4.43628532535048,
17.5484669222303));
#26607=CARTESIAN_POINT('Ctrl Pts',(-2.19689130411521,-4.40105451918029,
17.5439093998879));
#26608=CARTESIAN_POINT('Ctrl Pts',(-2.39074871964318,-4.30030560310476,
17.5314601469033));
#26609=CARTESIAN_POINT('Ctrl Pts',(-2.51071303830721,-4.23138595886653,
17.523549789167));
#26610=CARTESIAN_POINT('Ctrl Pts',(-2.73969921218768,-4.08666284233317,
17.5080429013634));
#26611=CARTESIAN_POINT('Ctrl Pts',(-2.84887643505824,-4.0113175666439,17.500453336624));
#26612=CARTESIAN_POINT('Ctrl Pts',(-2.98742940470873,-3.90718657077729,
17.4905904903077));
#26613=CARTESIAN_POINT('Ctrl Pts',(-3.01967781271314,-3.88231726084807,
17.4882778697887));
#26614=CARTESIAN_POINT('Ctrl Pts',(-3.08547956492844,-3.83025634968345,
17.4835258138457));
#26615=CARTESIAN_POINT('Ctrl Pts',(-3.11899113042396,-3.80301751728287,
17.4810871931756));
#26616=CARTESIAN_POINT('Ctrl Pts',(-3.26659537985682,-3.67977850965094,
17.4702502282586));
#26617=CARTESIAN_POINT('Ctrl Pts',(-3.37664721603989,-3.57905990043224,
17.4619086555512));
#26618=CARTESIAN_POINT('Ctrl Pts',(-3.55581846051312,-3.39945240288033,
17.4476952892152));
#26619=CARTESIAN_POINT('Ctrl Pts',(-3.62730180408219,-3.32307131481538,
17.441833947363));
#26620=CARTESIAN_POINT('Ctrl Pts',(-3.72253557251001,-3.21457527778905,
17.433718105896));
#26621=CARTESIAN_POINT('Ctrl Pts',(-3.74841219452511,-3.1843635631397,17.4314796364833));
#26622=CARTESIAN_POINT('Ctrl Pts',(-3.81981495270167,-3.09892228062133,
17.4252054426908));
#26623=CARTESIAN_POINT('Ctrl Pts',(-3.86450588523843,-3.04300832763046,
17.4211639666958));
#26624=CARTESIAN_POINT('Ctrl Pts',(-3.95185751092409,-2.92869126635205,
17.4130184227654));
#26625=CARTESIAN_POINT('Ctrl Pts',(-3.99448221434602,-2.87028256374707,
17.4089151258923));
#26626=CARTESIAN_POINT('Ctrl Pts',(-4.12768848864678,-2.67903291247003,
17.3956550985692));
#26627=CARTESIAN_POINT('Ctrl Pts',(-4.21304875382387,-2.54268532526417,
17.3864635392939));
#26628=CARTESIAN_POINT('Ctrl Pts',(-4.33756876230242,-2.32024684315445,
17.3718707430376));
#26629=CARTESIAN_POINT('Ctrl Pts',(-4.38119174835607,-2.23678501058983,
17.3664808507323));
#26630=CARTESIAN_POINT('Ctrl Pts',(-4.4492827431028,-2.0968649473384,17.3575964777399));
#26631=CARTESIAN_POINT('Ctrl Pts',(-4.47513550988072,-2.04110799178625,
17.3540947494371));
#26632=CARTESIAN_POINT('Ctrl Pts',(-4.51476971886499,-1.95125300532157,
17.3485179449188));
#26633=CARTESIAN_POINT('Ctrl Pts',(-4.52922523739406,-1.91745995938972,
17.3464356708467));
#26634=CARTESIAN_POINT('Ctrl Pts',(-4.56599999550418,-1.82875376661715,
17.3410078714906));
#26635=CARTESIAN_POINT('Ctrl Pts',(-4.58770773675193,-1.77359356809547,
17.3376695546362));
#26636=CARTESIAN_POINT('Ctrl Pts',(-4.66912518485959,-1.55520389979611,
17.3245684348376));
#26637=CARTESIAN_POINT('Ctrl Pts',(-4.7211625410511,-1.38924944582241,17.314860470125));
#26638=CARTESIAN_POINT('Ctrl Pts',(-4.78429915932931,-1.14286976385979,
17.3005925636965));
#26639=CARTESIAN_POINT('Ctrl Pts',(-4.8023725282632,-1.06437196637666,17.2960684497278));
#26640=CARTESIAN_POINT('Ctrl Pts',(-4.83320912146336,-0.913594176086029,
17.2874005955588));
#26641=CARTESIAN_POINT('Ctrl Pts',(-4.84629817455614,-0.841402738694301,
17.2832600223409));
#26642=CARTESIAN_POINT('Ctrl Pts',(-4.86882359396789,-0.699099860195667,
17.275106050713));
#26643=CARTESIAN_POINT('Ctrl Pts',(-4.878371930121,-0.629023815874242,17.2710944068513));
#26644=CARTESIAN_POINT('Ctrl Pts',(-4.90762283464867,-0.373225186314052,
17.2564529353761));
#26645=CARTESIAN_POINT('Ctrl Pts',(-4.91825449348514,-0.186627823734712,
17.245770479597));
#26646=CARTESIAN_POINT('Ctrl Pts',(-4.91824955815441,0.0184161788696644,
17.2340334398973));
#26647=CARTESIAN_POINT('Ctrl Pts',(-4.918147005371,0.0367138400748713,17.2329861343362));
#26648=CARTESIAN_POINT('Ctrl Pts',(-4.91683555630391,0.153957453619647,
17.2262762700073));
#26649=CARTESIAN_POINT('Ctrl Pts',(-4.91274285224247,0.252849349144806,
17.2206199253197));
#26650=CARTESIAN_POINT('Ctrl Pts',(-4.90276274421755,0.392115347569802,
17.2126747798129));
#26651=CARTESIAN_POINT('Ctrl Pts',(-4.89935277553649,0.432642360882363,
17.2103652473645));
#26652=CARTESIAN_POINT('Ctrl Pts',(-4.89127973198438,0.516174812108789,
17.2056123643494));
#26653=CARTESIAN_POINT('Ctrl Pts',(-4.88655116919175,0.559170441647649,
17.2031698603842));
#26654=CARTESIAN_POINT('Ctrl Pts',(-4.86682792173742,0.71906825582968,17.1940902140146));
#26655=CARTESIAN_POINT('Ctrl Pts',(-4.84819988177671,0.835482873806668,
17.1874866343439));
#26656=CARTESIAN_POINT('Ctrl Pts',(-4.80750001899003,1.04197008281173,17.1756954892456));
#26657=CARTESIAN_POINT('Ctrl Pts',(-4.78703320865461,1.13228305424205,17.1705112504368));
#26658=CARTESIAN_POINT('Ctrl Pts',(-4.76403457365963,1.22194829820076,17.1653174600137));
#26659=CARTESIAN_POINT('',(-4.91824992201636,-7.83730597753569E-6,16.8896169247543));
#26660=CARTESIAN_POINT('Ctrl Pts',(-4.76403458706411,1.22194824594044,16.8201710428097));
#26661=CARTESIAN_POINT('Ctrl Pts',(-4.76683376815824,1.21103502143015,16.820810022915));
#26662=CARTESIAN_POINT('Ctrl Pts',(-4.76959547071965,1.20011209781449,16.8214485515573));
#26663=CARTESIAN_POINT('Ctrl Pts',(-4.78039081463275,1.1567890969395,16.8239770185866));
#26664=CARTESIAN_POINT('Ctrl Pts',(-4.78813206739585,1.12431698757102,16.8258632257805));
#26665=CARTESIAN_POINT('Ctrl Pts',(-4.80595938298161,1.04601132814585,16.830393427176));
#26666=CARTESIAN_POINT('Ctrl Pts',(-4.81572122274099,1.00010721898561,16.8330340899698));
#26667=CARTESIAN_POINT('Ctrl Pts',(-4.8738428179346,0.706180720126455,16.8498689318998));
#26668=CARTESIAN_POINT('Ctrl Pts',(-4.90368400624962,0.454882822490331,
16.863950195434));
#26669=CARTESIAN_POINT('Ctrl Pts',(-4.91686092655596,0.134970651184922,
16.8819877004013));
#26670=CARTESIAN_POINT('Ctrl Pts',(-4.91825010759213,0.0674847396381241,
16.8857975340099));
#26671=CARTESIAN_POINT('Ctrl Pts',(-4.91824999999375,-7.84079902334413E-6,
16.8896167897774));
#26672=CARTESIAN_POINT('Ctrl Pts',(-4.91824999999374,-7.84493095884421E-6,
16.8896167900112));
#26673=CARTESIAN_POINT('Ctrl Pts',(-4.9182499406561,-0.0372086038747788,
16.8917218986356));
#26674=CARTESIAN_POINT('Ctrl Pts',(-4.91782781161351,-0.074408016725493,
16.8938296531246));
#26675=CARTESIAN_POINT('Ctrl Pts',(-4.91603513617609,-0.1533922633977,16.8983118618922));
#26676=CARTESIAN_POINT('Ctrl Pts',(-4.9145537589959,-0.195171630419358,
16.9006868621136));
#26677=CARTESIAN_POINT('Ctrl Pts',(-4.90029915421615,-0.490732554241179,
16.9175211677159));
#26678=CARTESIAN_POINT('Ctrl Pts',(-4.86840743386882,-0.743206820677955,
16.9320965060318));
#26679=CARTESIAN_POINT('Ctrl Pts',(-4.80771245688787,-1.03791829214628,
16.9492782213025));
#26680=CARTESIAN_POINT('Ctrl Pts',(-4.79761805181208,-1.08362102737906,
16.9519467852207));
#26681=CARTESIAN_POINT('Ctrl Pts',(-4.77921665046172,-1.16162959670902,
16.9565063199693));
#26682=CARTESIAN_POINT('Ctrl Pts',(-4.77123052301745,-1.19400772017509,
16.9584001692723));
#26683=CARTESIAN_POINT('Ctrl Pts',(-4.75269895615327,-1.26598368377879,
16.9626119081756));
#26684=CARTESIAN_POINT('Ctrl Pts',(-4.74198667733389,-1.30553607717061,
16.9649273551055));
#26685=CARTESIAN_POINT('Ctrl Pts',(-4.70373745743341,-1.44007540284274,
16.972815135504));
#26686=CARTESIAN_POINT('Ctrl Pts',(-4.67383033374763,-1.5343642451736,16.9783635396721));
#26687=CARTESIAN_POINT('Ctrl Pts',(-4.59589210317195,-1.75659305285647,
16.991563184021));
#26688=CARTESIAN_POINT('Ctrl Pts',(-4.54533292936468,-1.88355827876789,
16.9992047563436));
#26689=CARTESIAN_POINT('Ctrl Pts',(-4.45953232575029,-2.07536994975504,
17.011003276141));
#26690=CARTESIAN_POINT('Ctrl Pts',(-4.42800903348103,-2.14180411217169,
17.0151380531904));
#26691=CARTESIAN_POINT('Ctrl Pts',(-4.36635535599447,-2.26455277884726,
17.0228823151365));
#26692=CARTESIAN_POINT('Ctrl Pts',(-4.33659445330829,-2.32103572121766,
17.0264884724047));
#26693=CARTESIAN_POINT('Ctrl Pts',(-4.27101249070263,-2.43983597970989,
17.034172033163));
#26694=CARTESIAN_POINT('Ctrl Pts',(-4.23490783685697,-2.50197976732081,
17.0382507954912));
#26695=CARTESIAN_POINT('Ctrl Pts',(-4.11573940102004,-2.69711972231305,
17.0512601399769));
#26696=CARTESIAN_POINT('Ctrl Pts',(-4.02767305029983,-2.82694434760437,
17.0602234027118));
#26697=CARTESIAN_POINT('Ctrl Pts',(-3.87563938326855,-3.02950686859028,
17.0747218469415));
#26698=CARTESIAN_POINT('Ctrl Pts',(-3.81546241605834,-3.10495397510474,
17.0802456993313));
#26699=CARTESIAN_POINT('Ctrl Pts',(-3.72304455923327,-3.21407618460228,
17.0884108157213));
#26700=CARTESIAN_POINT('Ctrl Pts',(-3.6924818841511,-3.2491420556541,17.091062784323));
#26701=CARTESIAN_POINT('Ctrl Pts',(-3.63921215664185,-3.30853818230312,
17.0956013388401));
#26702=CARTESIAN_POINT('Ctrl Pts',(-3.61674716605781,-3.33308115549669,
17.0974907567837));
#26703=CARTESIAN_POINT('Ctrl Pts',(-3.5659185569494,-3.38749233372036,17.1017099586851));
#26704=CARTESIAN_POINT('Ctrl Pts',(-3.53742522617143,-3.41723605835062,
17.1040372356401));
#26705=CARTESIAN_POINT('Ctrl Pts',(-3.44025786187565,-3.51614972297263,
17.1118560223275));
#26706=CARTESIAN_POINT('Ctrl Pts',(-3.36990173456311,-3.58363582195775,
17.1173245850347));
#26707=CARTESIAN_POINT('Ctrl Pts',(-3.19585635448023,-3.7409204623283,17.1304732700751));
#26708=CARTESIAN_POINT('Ctrl Pts',(-3.09032675873492,-3.82855901390511,
17.1381433476802));
#26709=CARTESIAN_POINT('Ctrl Pts',(-2.92272617665242,-3.95629545377406,
17.1499754693926));
#26710=CARTESIAN_POINT('Ctrl Pts',(-2.86318442822054,-3.99959708141711,
17.1541151588609));
#26711=CARTESIAN_POINT('Ctrl Pts',(-2.75025028128185,-4.07791360674584,
17.1618632466984));
#26712=CARTESIAN_POINT('Ctrl Pts',(-2.69710440767758,-4.11325706668356,
17.1654682887335));
#26713=CARTESIAN_POINT('Ctrl Pts',(-2.5827538493258,-4.18613402094023,17.1731460026015));
#26714=CARTESIAN_POINT('Ctrl Pts',(-2.52138470493362,-4.22338187911524,
17.1772200161051));
#26715=CARTESIAN_POINT('Ctrl Pts',(-2.32215406245505,-4.33841384702664,
17.1903090314727));
#26716=CARTESIAN_POINT('Ctrl Pts',(-2.18134637949275,-4.41089118817675,
17.1993576022221));
#26717=CARTESIAN_POINT('Ctrl Pts',(-1.95014230137425,-4.51611516796321,
17.2138991803865));
#26718=CARTESIAN_POINT('Ctrl Pts',(-1.86185296493187,-4.55322466860793,
17.2193808066606));
#26719=CARTESIAN_POINT('Ctrl Pts',(-1.7293007192413,-4.60443812702757,17.2274944796773));
#26720=CARTESIAN_POINT('Ctrl Pts',(-1.68583069876612,-4.62053095975743,
17.2301371210996));
#26721=CARTESIAN_POINT('Ctrl Pts',(-1.61081791436717,-4.64710155229553,
17.2346639004896));
#26722=CARTESIAN_POINT('Ctrl Pts',(-1.57938453761665,-4.65787845487469,
17.236550844341));
#26723=CARTESIAN_POINT('Ctrl Pts',(-1.51395306982043,-4.67957306199701,
17.2404568802906));
#26724=CARTESIAN_POINT('Ctrl Pts',(-1.4799404065659,-4.69044074283164,17.2424751156509));
#26725=CARTESIAN_POINT('Ctrl Pts',(-1.36899914505102,-4.72456164860013,
17.2490238181737));
#26726=CARTESIAN_POINT('Ctrl Pts',(-1.29161781384732,-4.7463001480696,17.2535384293322));
#26727=CARTESIAN_POINT('Ctrl Pts',(-1.06690019192772,-4.80352648084476,
17.2665458857707));
#26728=CARTESIAN_POINT('Ctrl Pts',(-0.918412913925084,-4.83411423142414,
17.2750167009667));
#26729=CARTESIAN_POINT('Ctrl Pts',(-0.693717780619998,-4.86967244115822,
17.2877856464014));
#26730=CARTESIAN_POINT('Ctrl Pts',(-0.618420010849212,-4.87980640884685,
17.2920559518669));
#26731=CARTESIAN_POINT('Ctrl Pts',(-0.479811557003569,-4.89520127430561,
17.2999156178035));
#26732=CARTESIAN_POINT('Ctrl Pts',(-0.416575485034823,-4.90098759465092,
17.3035008947515));
#26733=CARTESIAN_POINT('Ctrl Pts',(-0.283783852069842,-4.91054984057586,
17.3110360203917));
#26734=CARTESIAN_POINT('Ctrl Pts',(-0.214224289609376,-4.91407578469857,
17.3149867284281));
#26735=CARTESIAN_POINT('Ctrl Pts',(0.0316490666192468,-4.9213084551853,
17.3289745817257));
#26736=CARTESIAN_POINT('Ctrl Pts',(0.208061245372728,-4.91701002417909,
17.3390577479166));
#26737=CARTESIAN_POINT('Ctrl Pts',(0.473134295322018,-4.89625837344953,
17.3542785133904));
#26738=CARTESIAN_POINT('Ctrl Pts',(0.562203186402082,-4.88683229051902,
17.3594038428411));
#26739=CARTESIAN_POINT('Ctrl Pts',(0.695508503642364,-4.869031778393,17.3670809849684));
#26740=CARTESIAN_POINT('Ctrl Pts',(0.739968372798642,-4.86247358796272,
17.3696424493637));
#26741=CARTESIAN_POINT('Ctrl Pts',(0.816961916429679,-4.8500359546179,17.3740778249231));
#26742=CARTESIAN_POINT('Ctrl Pts',(0.849537729134805,-4.84443610856278,
17.3759542768317));
#26743=CARTESIAN_POINT('Ctrl Pts',(0.924028911228534,-4.83085644665498,
17.380243488437));
#26744=CARTESIAN_POINT('Ctrl Pts',(0.965901988871422,-4.82265869019897,
17.3826533743843));
#26745=CARTESIAN_POINT('Ctrl Pts',(1.15754598477091,-4.78254320035006,17.3936901389126));
#26746=CARTESIAN_POINT('Ctrl Pts',(1.30588318341657,-4.74418615847176,17.4022556708684));
#26747=CARTESIAN_POINT('Ctrl Pts',(1.55149358910475,-4.66828166653712,17.4166582271282));
#26748=CARTESIAN_POINT('Ctrl Pts',(1.64979873095074,-4.63445250261479,17.4224834675145));
#26749=CARTESIAN_POINT('Ctrl Pts',(1.78412862038106,-4.58341022674273,17.4305624585805));
#26750=CARTESIAN_POINT('Ctrl Pts',(1.82112686985034,-4.56883586284299,17.4328003118664));
#26751=CARTESIAN_POINT('Ctrl Pts',(1.92449369557707,-4.52666247356809,17.4390912820081));
#26752=CARTESIAN_POINT('Ctrl Pts',(1.99043948193806,-4.49805509581903,17.443150255538));
#26753=CARTESIAN_POINT('Ctrl Pts',(2.12251660826238,-4.43728637121658,17.4513824667194));
#26754=CARTESIAN_POINT('Ctrl Pts',(2.18860126062016,-4.40506656505984,17.4555551712934));
#26755=CARTESIAN_POINT('Ctrl Pts',(2.35543568900626,-4.31904460113421,17.4662362924335));
#26756=CARTESIAN_POINT('Ctrl Pts',(2.45507863244366,-4.26319269916226,17.4727566710008));
#26757=CARTESIAN_POINT('Ctrl Pts',(2.65854114989443,-4.13964718219351,17.4863744119855));
#26758=CARTESIAN_POINT('Ctrl Pts',(2.76193070440002,-4.07139517776031,17.4934693498927));
#26759=CARTESIAN_POINT('Ctrl Pts',(2.90480001019544,-3.96913200708307,17.503508931808));
#26760=CARTESIAN_POINT('Ctrl Pts',(2.94648649402665,-3.93828508282532,17.5064679586548));
#26761=CARTESIAN_POINT('Ctrl Pts',(3.02155255881747,-3.88087899931883,17.5118477848604));
#26762=CARTESIAN_POINT('Ctrl Pts',(3.05508941652167,-3.85453374436886,17.514270603834));
#26763=CARTESIAN_POINT('Ctrl Pts',(3.12101101783324,-3.80134739514397,17.5190692926702));
#26764=CARTESIAN_POINT('Ctrl Pts',(3.1534025737818,-3.77452037383418,17.5214451056121));
#26765=CARTESIAN_POINT('Ctrl Pts',(3.3137768020608,-3.63819126262147,17.5333117882414));
#26766=CARTESIAN_POINT('Ctrl Pts',(3.43642015488624,-3.52258004292693,17.5427264075202));
#26767=CARTESIAN_POINT('Ctrl Pts',(3.63043402176212,-3.31989564739133,17.5584486293972));
#26768=CARTESIAN_POINT('Ctrl Pts',(3.70518304087935,-3.2362596602761,17.5647374046495));
#26769=CARTESIAN_POINT('Ctrl Pts',(3.82603544698187,-3.09135814463713,17.5753584560345));
#26770=CARTESIAN_POINT('Ctrl Pts',(3.87368404362773,-3.03143764009383,17.5796765181378));
#26771=CARTESIAN_POINT('Ctrl Pts',(3.96172553014344,-2.91525409557114,17.5879231331634));
#26772=CARTESIAN_POINT('Ctrl Pts',(4.00236673547217,-2.85920198433273,17.5918485108084));
#26773=CARTESIAN_POINT('Ctrl Pts',(4.16357885728932,-2.62668358152558,17.607930666373));
#26774=CARTESIAN_POINT('Ctrl Pts',(4.2737686847842,-2.44330806048286,17.6201624882223));
#26775=CARTESIAN_POINT('Ctrl Pts',(4.41900557269763,-2.16153706332632,17.6383032501186));
#26776=CARTESIAN_POINT('Ctrl Pts',(4.4634271657228,-2.06825314382132,17.6442072384528));
#26777=CARTESIAN_POINT('Ctrl Pts',(4.52066950472716,-1.93759612130531,17.6523202728613));
#26778=CARTESIAN_POINT('Ctrl Pts',(4.53602732433491,-1.90136468831857,17.6545536972916));
#26779=CARTESIAN_POINT('Ctrl Pts',(4.56865922260557,-1.82173472271906,17.6594250612977));
#26780=CARTESIAN_POINT('Ctrl Pts',(4.58575322658706,-1.77826654584235,17.6620608270097));
#26781=CARTESIAN_POINT('Ctrl Pts',(4.67110681286416,-1.55180208258173,17.6756908288605));
#26782=CARTESIAN_POINT('Ctrl Pts',(4.72904111056056,-1.36510076895345,17.6865919334457));
#26783=CARTESIAN_POINT('Ctrl Pts',(4.79531409463303,-1.09584082731927,17.702145695313));
#26784=CARTESIAN_POINT('Ctrl Pts',(4.81291427397403,-1.01575607806269,17.7067502313632));
#26785=CARTESIAN_POINT('Ctrl Pts',(4.84264007347487,-0.86229104156598,17.7155533783299));
#26786=CARTESIAN_POINT('Ctrl Pts',(4.85511936876258,-0.789002195977594,
17.7197486097811));
#26787=CARTESIAN_POINT('Ctrl Pts',(4.87629931738731,-0.644954579899805,
17.7279883213161));
#26788=CARTESIAN_POINT('Ctrl Pts',(4.88513226089707,-0.574233470319792,
17.7320308799801));
#26789=CARTESIAN_POINT('Ctrl Pts',(4.91143611162197,-0.318565151268578,
17.7466468501595));
#26790=CARTESIAN_POINT('Ctrl Pts',(4.91996296057207,-0.13285780833357,17.7572721194808));
#26791=CARTESIAN_POINT('Ctrl Pts',(4.91665743448756,0.174546046984221,17.7748699046814));
#26792=CARTESIAN_POINT('Ctrl Pts',(4.91083499096335,0.296119722934534,17.78183025779));
#26793=CARTESIAN_POINT('Ctrl Pts',(4.89711999655882,0.457159542235371,17.7910245076019));
#26794=CARTESIAN_POINT('Ctrl Pts',(4.89324494839363,0.496923583102964,17.7932925183525));
#26795=CARTESIAN_POINT('Ctrl Pts',(4.8839192052753,0.581883330872484,17.7981315823567));
#26796=CARTESIAN_POINT('Ctrl Pts',(4.87832465690898,0.627059505105819,17.800700969163));
#26797=CARTESIAN_POINT('Ctrl Pts',(4.84446634353182,0.872482049445226,17.8146571088486));
#26798=CARTESIAN_POINT('Ctrl Pts',(4.80449932921346,1.07091867939412,17.8259411428385));
#26799=CARTESIAN_POINT('Ctrl Pts',(4.73170926027818,1.34409326716187,17.8418007628503));
#26800=CARTESIAN_POINT('Ctrl Pts',(4.70908366565301,1.42133391690607,17.846321445072));
#26801=CARTESIAN_POINT('Ctrl Pts',(4.66215288266024,1.56809828555493,17.8550003432272));
#26802=CARTESIAN_POINT('Ctrl Pts',(4.63816140783909,1.63769970446574,17.8591554630706));
#26803=CARTESIAN_POINT('Ctrl Pts',(4.59068015969314,1.76602232320095,17.8668998894089));
#26804=CARTESIAN_POINT('Ctrl Pts',(4.56760247114469,1.82487992197727,17.8704854749731));
#26805=CARTESIAN_POINT('Ctrl Pts',(4.49607581716378,1.99743773762816,17.8811038852354));
#26806=CARTESIAN_POINT('Ctrl Pts',(4.44446930119099,2.10977422106515,17.8881560886962));
#26807=CARTESIAN_POINT('Ctrl Pts',(4.33066635607802,2.33474499407003,17.9025769022562));
#26808=CARTESIAN_POINT('Ctrl Pts',(4.26817112610533,2.44712495697199,17.9099414526203));
#26809=CARTESIAN_POINT('Ctrl Pts',(4.16377178777008,2.61866587745628,17.9214172275421));
#26810=CARTESIAN_POINT('Ctrl Pts',(4.12484134023941,2.67956910444376,17.9255397127467));
#26811=CARTESIAN_POINT('Ctrl Pts',(4.06368723121824,2.77074652813486,17.9317779096321));
#26812=CARTESIAN_POINT('Ctrl Pts',(4.04243603938053,2.80166042879257,17.9339046950502));
#26813=CARTESIAN_POINT('Ctrl Pts',(3.99055209179637,2.87531596733622,17.9390000711915));
#26814=CARTESIAN_POINT('Ctrl Pts',(3.95958351300881,2.91781534820298,17.9419641157484));
#26815=CARTESIAN_POINT('Ctrl Pts',(3.85164963431727,3.06105348419405,17.9520539573294));
#26816=CARTESIAN_POINT('Ctrl Pts',(3.77147373167813,3.15931000356964,17.9591486651954));
#26817=CARTESIAN_POINT('Ctrl Pts',(3.67885148202854,3.26426244049555,17.966990730186));
#26818=CARTESIAN_POINT('Ctrl Pts',(3.67007218314261,3.27413006424849,17.9677307086419));
#26819=CARTESIAN_POINT('Ctrl Pts',(3.59480914259729,3.3580399981993,17.974046507965));
#26820=CARTESIAN_POINT('Ctrl Pts',(3.52613253760364,3.43008374717459,17.9796255430893));
#26821=CARTESIAN_POINT('Ctrl Pts',(3.42767627175922,3.52728326266153,17.9874058734882));
#26822=CARTESIAN_POINT('Ctrl Pts',(3.39971208030225,3.55424388418456,17.9895924650558));
#26823=CARTESIAN_POINT('Ctrl Pts',(3.31968490090331,3.62959041573985,17.9957878358959));
#26824=CARTESIAN_POINT('Ctrl Pts',(3.26688866224574,3.67718271812721,17.9998024868162));
#26825=CARTESIAN_POINT('Ctrl Pts',(3.15658337492318,3.77236437169542,18.0080539049934));
#26826=CARTESIAN_POINT('Ctrl Pts',(3.09898499484218,3.81982242759822,18.0122906958888));
#26827=CARTESIAN_POINT('Ctrl Pts',(2.91522586072174,3.96433753227178,18.0255969663952));
#26828=CARTESIAN_POINT('Ctrl Pts',(2.78542134979614,4.05659225731117,18.0346990137211));
#26829=CARTESIAN_POINT('Ctrl Pts',(2.53883343977273,4.21442310591339,18.0514591181867));
#26830=CARTESIAN_POINT('Ctrl Pts',(2.42340241549888,4.28184057684926,18.0591068381778));
#26831=CARTESIAN_POINT('Ctrl Pts',(2.26994530141025,4.36327165692594,18.0689899881626));
#26832=CARTESIAN_POINT('Ctrl Pts',(2.23429288528658,4.38163515034634,18.0712667101102));
#26833=CARTESIAN_POINT('Ctrl Pts',(2.15793752984839,4.41978921011624,18.0760996048673));
#26834=CARTESIAN_POINT('Ctrl Pts',(2.1171779461716,4.43945814876808,18.0786542264437));
#26835=CARTESIAN_POINT('Ctrl Pts',(1.82178945993727,4.57700732524579,18.0970107340914));
#26836=CARTESIAN_POINT('Ctrl Pts',(1.55775593073986,4.67346891892216,18.1126164539261));
#26837=CARTESIAN_POINT('Ctrl Pts',(1.21518105367392,4.7663451239606,18.132605222575));
#26838=CARTESIAN_POINT('Ctrl Pts',(1.1429911810417,4.78416991990166,18.1368012423489));
#26839=CARTESIAN_POINT('Ctrl Pts',(1.00088054385737,4.81585903080965,18.1450411897316));
#26840=CARTESIAN_POINT('Ctrl Pts',(0.931007274864338,4.82985355512137,18.1490831887826));
#26841=CARTESIAN_POINT('Ctrl Pts',(0.675138795852732,4.87534114974747,18.1638618958698));
#26842=CARTESIAN_POINT('Ctrl Pts',(0.487678907423868,4.89764547904067,18.1746524893051));
#26843=CARTESIAN_POINT('Ctrl Pts',(0.217569672574943,4.91411929470162,18.1901427464503));
#26844=CARTESIAN_POINT('Ctrl Pts',(0.135621870931243,4.91706333516054,18.1948335576079));
#26845=CARTESIAN_POINT('Ctrl Pts',(0.0261654859623787,4.91825713912549,
18.2010800027011));
#26846=CARTESIAN_POINT('Ctrl Pts',(-0.00130966417450025,4.91832656650228,
18.2026463293252));
#26847=CARTESIAN_POINT('Ctrl Pts',(-0.0721610569434313,4.91791190180704,
18.2066805765205));
#26848=CARTESIAN_POINT('Ctrl Pts',(-0.115533158525906,4.91708418068861,
18.2091454304341));
#26849=CARTESIAN_POINT('Ctrl Pts',(-0.200277612567998,4.91434499723206,
18.2139497184883));
#26850=CARTESIAN_POINT('Ctrl Pts',(-0.241648012259479,4.91248451985136,
18.2162894408996));
#26851=CARTESIAN_POINT('Ctrl Pts',(-0.428192851919074,4.90173314014378,
18.2268254952407));
#26852=CARTESIAN_POINT('Ctrl Pts',(-0.572954456015661,4.88692756742573,
18.234965135289));
#26853=CARTESIAN_POINT('Ctrl Pts',(-0.8251215528175,4.84977680641163,18.2492443373602));
#26854=CARTESIAN_POINT('Ctrl Pts',(-0.932831791129876,4.83021586158297,
18.2553757115236));
#26855=CARTESIAN_POINT('Ctrl Pts',(-1.07974663329832,4.79843732273243,18.2638240311053));
#26856=CARTESIAN_POINT('Ctrl Pts',(-1.11958474696796,4.78929885288586,18.2661235377934));
#26857=CARTESIAN_POINT('Ctrl Pts',(-1.23011524343585,4.76248976315965,18.272530900512));
#26858=CARTESIAN_POINT('Ctrl Pts',(-1.30053531215792,4.7437432471703,18.2766445992081));
#26859=CARTESIAN_POINT('Ctrl Pts',(-1.43163980041649,4.70570310229431,18.2843724967017));
#26860=CARTESIAN_POINT('Ctrl Pts',(-1.49241678125781,4.68678207765478,18.2879833130826));
#26861=CARTESIAN_POINT('Ctrl Pts',(-1.67404645381293,4.62634601525868,18.2988666118654));
#26862=CARTESIAN_POINT('Ctrl Pts',(-1.79366451009108,4.58129631463873,18.3061601185073));
#26863=CARTESIAN_POINT('Ctrl Pts',(-2.02526796087638,4.48360878631622,18.320540452009));
#26864=CARTESIAN_POINT('Ctrl Pts',(-2.13729393060609,4.4313014779321,18.3276210574031));
#26865=CARTESIAN_POINT('Ctrl Pts',(-2.29331750090348,4.35115643869589,18.3376438546885));
#26866=CARTESIAN_POINT('Ctrl Pts',(-2.33902781134628,4.32675588354676,18.3406004004621));
#26867=CARTESIAN_POINT('Ctrl Pts',(-2.42162253848157,4.28097465134513,18.3459764118893));
#26868=CARTESIAN_POINT('Ctrl Pts',(-2.45863090798584,4.25982790719744,18.3483978925117));
#26869=CARTESIAN_POINT('Ctrl Pts',(-2.53162015050201,4.21685345518621,18.3531964877128));
#26870=CARTESIAN_POINT('Ctrl Pts',(-2.56760511129622,4.19503965350301,18.355573534135));
#26871=CARTESIAN_POINT('Ctrl Pts',(-2.69572357476784,4.11510909626707,18.3640867998924));
#26872=CARTESIAN_POINT('Ctrl Pts',(-2.78620115859185,4.05439663183011,18.3701939158534));
#26873=CARTESIAN_POINT('Ctrl Pts',(-3.0050329793175,3.8967684326096,18.3853058414909));
#26874=CARTESIAN_POINT('Ctrl Pts',(-3.1307909095399,3.79646877866635,18.3942996292456));
#26875=CARTESIAN_POINT('Ctrl Pts',(-3.3115468559155,3.63720557891296,18.4078520372935));
#26876=CARTESIAN_POINT('Ctrl Pts',(-3.37037875960248,3.58275785010503,18.4123705090721));
#26877=CARTESIAN_POINT('Ctrl Pts',(-3.47725622901403,3.47888176194091,18.4207977421602));
#26878=CARTESIAN_POINT('Ctrl Pts',(-3.52564438744697,3.42983391802385,18.4247020309548));
#26879=CARTESIAN_POINT('Ctrl Pts',(-3.64996375012111,3.29840805285166,18.4349797245579));
#26880=CARTESIAN_POINT('Ctrl Pts',(-3.72413812139249,3.21442464593867,18.4413663654025));
#26881=CARTESIAN_POINT('Ctrl Pts',(-3.88680478978675,3.0170508958023,18.4559859940373));
#26882=CARTESIAN_POINT('Ctrl Pts',(-3.97332244634148,2.90216405837288,18.4642234223075));
#26883=CARTESIAN_POINT('Ctrl Pts',(-4.08582384968827,2.73829394405004,18.4755854740975));
#26884=CARTESIAN_POINT('Ctrl Pts',(-4.11620112735012,2.69241501361351,18.4787264154735));
#26885=CARTESIAN_POINT('Ctrl Pts',(-4.16965373116222,2.60866560610713,18.4843846522103));
#26886=CARTESIAN_POINT('Ctrl Pts',(-4.19299889058817,2.57097429925913,18.4869043138299));
#26887=CARTESIAN_POINT('Ctrl Pts',(-4.23678707074901,2.49809407446726,18.4917227343884));
#26888=CARTESIAN_POINT('Ctrl Pts',(-4.25730911779791,2.46295712550303,18.494022203581));
#26889=CARTESIAN_POINT('Ctrl Pts',(-4.33845233361514,2.31998224504474,18.503293824949));
#26890=CARTESIAN_POINT('Ctrl Pts',(-4.39543153582698,2.21012863082383,18.5102254462793));
#26891=CARTESIAN_POINT('Ctrl Pts',(-4.48710867158797,2.01577597990305,18.5222647591752));
#26892=CARTESIAN_POINT('Ctrl Pts',(-4.5237077260229,1.93224361286819,18.5273701829613));
#26893=CARTESIAN_POINT('Ctrl Pts',(-4.58812028931384,1.77335235877483,18.5369886671671));
#26894=CARTESIAN_POINT('Ctrl Pts',(-4.61645121734951,1.69823566531507,18.5414979919757));
#26895=CARTESIAN_POINT('Ctrl Pts',(-4.66718204829661,1.55306119512076,18.5501600731409));
#26896=CARTESIAN_POINT('Ctrl Pts',(-4.68987399224164,1.48312815289078,18.5543097715015));
#26897=CARTESIAN_POINT('Ctrl Pts',(-4.72916248407022,1.35211241555791,18.5620517758427));
#26898=CARTESIAN_POINT('Ctrl Pts',(-4.74616410155201,1.29116691226652,18.5656404041838));
#26899=CARTESIAN_POINT('Ctrl Pts',(-4.76267050742994,1.22725719054281,18.5693926742232));
#26900=CARTESIAN_POINT('Ctrl Pts',(-4.76335365943198,1.2246029924092,18.5695484879206));
#26901=CARTESIAN_POINT('Ctrl Pts',(-4.76403458707798,1.22194824588636,18.5697043142649));
#26902=CARTESIAN_POINT('Origin',(0.,0.,-3.23514056400928));
#26903=CARTESIAN_POINT('',(-4.76403458704968,1.22194824599669,20.6652050067296));
#26904=CARTESIAN_POINT('',(-4.76403459893337,1.2219481996655,20.3200311864783));
#26905=CARTESIAN_POINT('',(-4.76403458704967,1.22194824599672,-3.23514056400928));
#26906=CARTESIAN_POINT('',(-4.91824999838119,-0.000126187989179228,18.9851405640093));
#26907=CARTESIAN_POINT('Ctrl Pts',(-4.91824999838119,-0.000126187989179228,
18.9851405640093));
#26908=CARTESIAN_POINT('Ctrl Pts',(-4.91824608488009,-0.152657161176494,
18.9937788711624));
#26909=CARTESIAN_POINT('Ctrl Pts',(-4.91114211048955,-0.305153403297447,
19.0024171783155));
#26910=CARTESIAN_POINT('Ctrl Pts',(-4.89697369991277,-0.456981011490179,
19.0110554854686));
#26911=CARTESIAN_POINT('Ctrl Pts',(-4.8948411352829,-0.479833411575278,
19.012355684118));
#26912=CARTESIAN_POINT('Ctrl Pts',(-4.89254862248211,-0.50267067097549,
19.0136558827675));
#26913=CARTESIAN_POINT('Ctrl Pts',(-4.89009638484907,-0.525490636820512,
19.0149560814169));
#26914=CARTESIAN_POINT('Ctrl Pts',(-4.87471295583977,-0.668645329433346,
19.023112515097));
#26915=CARTESIAN_POINT('Ctrl Pts',(-4.85303617925358,-0.81115080021202,
19.0312689487771));
#26916=CARTESIAN_POINT('Ctrl Pts',(-4.82514522750803,-0.95244768672954,
19.0394253824572));
#26917=CARTESIAN_POINT('Ctrl Pts',(-4.79725995235747,-1.09371581534719,
19.0475801560731));
#26918=CARTESIAN_POINT('Ctrl Pts',(-4.76316308993429,-1.23377552232594,
19.055734929689));
#26919=CARTESIAN_POINT('Ctrl Pts',(-4.72298502473125,-1.37207708189603,
19.0638897033048));
#26920=CARTESIAN_POINT('Ctrl Pts',(-4.68280553468754,-1.51038354607481,
19.0720447661147));
#26921=CARTESIAN_POINT('Ctrl Pts',(-4.63654450007743,-1.6469314157073,19.0801998289245));
#26922=CARTESIAN_POINT('Ctrl Pts',(-4.58438247970837,-1.78118509488568,
19.0883548917343));
#26923=CARTESIAN_POINT('Ctrl Pts',(-4.53222351863791,-1.91543090009581,
19.0965094762503));
#26924=CARTESIAN_POINT('Ctrl Pts',(-4.47416438629209,-2.04738247246663,
19.1046640607664));
#26925=CARTESIAN_POINT('Ctrl Pts',(-4.41043417222228,-2.17652325395205,
19.1128186452824));
#26926=CARTESIAN_POINT('Ctrl Pts',(-4.34668828913151,-2.30569578661922,
19.1209752347242));
#26927=CARTESIAN_POINT('Ctrl Pts',(-4.27726868611204,-2.43205584716965,
19.1291318241661));
#26928=CARTESIAN_POINT('Ctrl Pts',(-4.20245116332172,-2.55511003332458,
19.137288413608));
#26929=CARTESIAN_POINT('Ctrl Pts',(-4.15165287706674,-2.63865920122057,
19.142826431306));
#26930=CARTESIAN_POINT('Ctrl Pts',(-4.09836717013825,-2.72068488610154,
19.148364449004));
#26931=CARTESIAN_POINT('Ctrl Pts',(-4.04269200790494,-2.80103987685316,
19.153902466702));
#26932=CARTESIAN_POINT('Ctrl Pts',(-3.96069321462759,-2.91938730524201,
19.1620589003821));
#26933=CARTESIAN_POINT('Ctrl Pts',(-3.87347869980731,-3.03415367771113,
19.1702153340622));
#26934=CARTESIAN_POINT('Ctrl Pts',(-3.78138560526144,-3.14488568422153,
19.1783717677423));
#26935=CARTESIAN_POINT('Ctrl Pts',(-3.68931125425647,-3.25559515364702,
19.1865265413582));
#26936=CARTESIAN_POINT('Ctrl Pts',(-3.59236051820411,-3.36227163805237,
19.1946813149741));
#26937=CARTESIAN_POINT('Ctrl Pts',(-3.49091089889729,-3.46449479123004,
19.2028360885901));
#26938=CARTESIAN_POINT('Ctrl Pts',(-3.38945768186793,-3.5667215695622,19.2109911513999));
#26939=CARTESIAN_POINT('Ctrl Pts',(-3.28350549537999,-3.66449446050219,
19.2191462142097));
#26940=CARTESIAN_POINT('Ctrl Pts',(-3.17346914021325,-3.75742953075825,
19.2273012770195));
#26941=CARTESIAN_POINT('Ctrl Pts',(-3.06343923867039,-3.85035915037949,
19.2354558615355));
#26942=CARTESIAN_POINT('Ctrl Pts',(-2.94932590394392,-3.93845130177503,
19.2436104460516));
#26943=CARTESIAN_POINT('Ctrl Pts',(-2.83157744438321,-4.02136198805333,
19.2517650305676));
#26944=CARTESIAN_POINT('Ctrl Pts',(-2.71380003461238,-4.10429305915703,
19.2599216200095));
#26945=CARTESIAN_POINT('Ctrl Pts',(-2.59238598769989,-4.18203992660568,
19.2680782094514));
#26946=CARTESIAN_POINT('Ctrl Pts',(-2.46781355110926,-4.25430127511693,
19.2762347988933));
#26947=CARTESIAN_POINT('Ctrl Pts',(-2.38323354822555,-4.30336401509966,
19.2817728165912));
#26948=CARTESIAN_POINT('Ctrl Pts',(-2.29719817246742,-4.34989888010521,
19.2873108342892));
#26949=CARTESIAN_POINT('Ctrl Pts',(-2.20986388044963,-4.39382347078079,
19.2928488519872));
#26950=CARTESIAN_POINT('Ctrl Pts',(-2.08123728521461,-4.4585159348193,19.3010052856673));
#26951=CARTESIAN_POINT('Ctrl Pts',(-1.94974394926948,-4.51756840679982,
19.3091617193473));
#26952=CARTESIAN_POINT('Ctrl Pts',(-1.81589680404786,-4.57074412536392,
19.3173181530274));
#26953=CARTESIAN_POINT('Ctrl Pts',(-1.68207690049345,-4.62390902117027,
19.3254729266433));
#26954=CARTESIAN_POINT('Ctrl Pts',(-1.54590445416985,-4.67119942620531,
19.3336277002592));
#26955=CARTESIAN_POINT('Ctrl Pts',(-1.40791206646716,-4.71242683503905,
19.3417824738751));
#26956=CARTESIAN_POINT('Ctrl Pts',(-1.26991478512027,-4.75365570592641,
19.3499375366849));
#26957=CARTESIAN_POINT('Ctrl Pts',(-1.13009775278517,-4.78882105098862,
19.3580925994948));
#26958=CARTESIAN_POINT('Ctrl Pts',(-0.989008902720726,-4.8177841849588,
19.3662476623046));
#26959=CARTESIAN_POINT('Ctrl Pts',(-0.847928327506779,-4.84674562024334,
19.3744022468206));
#26960=CARTESIAN_POINT('Ctrl Pts',(-0.705576411790162,-4.86950550582432,
19.3825568313366));
#26961=CARTESIAN_POINT('Ctrl Pts',(-0.56251140560929,-4.88597625670239,
19.3907114158526));
#26962=CARTESIAN_POINT('Ctrl Pts',(-0.419411224768708,-4.90245105715954,
19.3988680052945));
#26963=CARTESIAN_POINT('Ctrl Pts',(-0.275597935685257,-4.91263359460003,
19.4070245947364));
#26964=CARTESIAN_POINT('Ctrl Pts',(-0.131635658229963,-4.91648808764776,
19.4151811841783));
#26965=CARTESIAN_POINT('Ctrl Pts',(-0.0338906820886804,-4.91910514357135,
19.4207192018763));
#26966=CARTESIAN_POINT('Ctrl Pts',(0.0639228656633244,-4.9188061130699,
19.4262572195743));
#26967=CARTESIAN_POINT('Ctrl Pts',(0.161628174145175,-4.91559349375256,
19.4317952372723));
#26968=CARTESIAN_POINT('Ctrl Pts',(0.30552927960976,-4.91086192411335,19.4399516709524));
#26969=CARTESIAN_POINT('Ctrl Pts',(0.449249364441852,-4.89980619885904,
19.4481081046325));
#26970=CARTESIAN_POINT('Ctrl Pts',(0.592224736858196,-4.88246381692207,
19.4562645383126));
#26971=CARTESIAN_POINT('Ctrl Pts',(0.735171009755496,-4.86512496464875,
19.4644193119285));
#26972=CARTESIAN_POINT('Ctrl Pts',(0.877372540617288,-4.84150204851488,
19.4725740855444));
#26973=CARTESIAN_POINT('Ctrl Pts',(1.0182714523604,-4.81168435288599,19.4807288591603));
#26974=CARTESIAN_POINT('Ctrl Pts',(1.15917536082229,-4.78186559982778,19.4888839219701));
#26975=CARTESIAN_POINT('Ctrl Pts',(1.2987762295882,-4.74585169328947,19.4970389847799));
#26976=CARTESIAN_POINT('Ctrl Pts',(1.43652655403386,-4.70378300116572,19.5051940475897));
#26977=CARTESIAN_POINT('Ctrl Pts',(1.5742687994334,-4.66171677636759,19.5133486321057));
#26978=CARTESIAN_POINT('Ctrl Pts',(1.71016039788062,-4.61359657508639,19.5215032166218));
#26979=CARTESIAN_POINT('Ctrl Pts',(1.84366923352164,-4.5596125734393,19.5296578011378));
#26980=CARTESIAN_POINT('Ctrl Pts',(1.97721089429562,-4.50561529902248,19.5378143905797));
#26981=CARTESIAN_POINT('Ctrl Pts',(2.10836831117959,-4.44575146869014,19.5459709800216));
#26982=CARTESIAN_POINT('Ctrl Pts',(2.23662899856581,-4.38025955683844,19.5541275694634));
#26983=CARTESIAN_POINT('Ctrl Pts',(2.32371318513178,-4.33579300994492,19.5596655871614));
#26984=CARTESIAN_POINT('Ctrl Pts',(2.40946242741656,-4.28873297392088,19.5652036048594));
#26985=CARTESIAN_POINT('Ctrl Pts',(2.49372265869397,-4.23916623453436,19.5707416225574));
#26986=CARTESIAN_POINT('Ctrl Pts',(2.61782175439267,-4.16616397188512,19.5788980562375));
#26987=CARTESIAN_POINT('Ctrl Pts',(2.73873619268232,-4.08769493048598,19.5870544899176));
#26988=CARTESIAN_POINT('Ctrl Pts',(2.85598892375259,-4.00406172903247,19.5952109235977));
#26989=CARTESIAN_POINT('Ctrl Pts',(2.97321779058655,-3.92044554929322,19.6033656972135));
#26990=CARTESIAN_POINT('Ctrl Pts',(3.08678616468886,-3.83166750048702,19.6115204708294));
#26991=CARTESIAN_POINT('Ctrl Pts',(3.19624687824738,-3.73807289332269,19.6196752444453));
#26992=CARTESIAN_POINT('Ctrl Pts',(3.30571147362727,-3.64447496699906,19.6278303072551));
#26993=CARTESIAN_POINT('Ctrl Pts',(3.41106786021718,-3.54606035513149,19.635985370065));
#26994=CARTESIAN_POINT('Ctrl Pts',(3.51190241865963,-3.44321426349169,19.6441404328748));
#26995=CARTESIAN_POINT('Ctrl Pts',(3.61273106316279,-3.34037420376746,19.6522950173908));
#26996=CARTESIAN_POINT('Ctrl Pts',(3.70903817649805,-3.23310342386507,19.6604496019068));
#26997=CARTESIAN_POINT('Ctrl Pts',(3.80044748254855,-3.12182350476295,19.6686041864228));
#26998=CARTESIAN_POINT('Ctrl Pts',(3.89187926293657,-3.01051622583752,19.6767607758647));
#26999=CARTESIAN_POINT('Ctrl Pts',(3.9784106171142,-2.89519809660406,19.6849173653066));
#27000=CARTESIAN_POINT('Ctrl Pts',(4.05970561433167,-2.77632371806025,19.6930739547485));
#27001=CARTESIAN_POINT('Ctrl Pts',(4.11490186229257,-2.69561248245065,19.6986119724465));
#27002=CARTESIAN_POINT('Ctrl Pts',(4.16768504855189,-2.61326252925448,19.7041499901445));
#27003=CARTESIAN_POINT('Ctrl Pts',(4.21796140497238,-2.52942377799043,19.7096880078425));
#27004=CARTESIAN_POINT('Ctrl Pts',(4.29200879686997,-2.40594544119271,19.7178444415226));
#27005=CARTESIAN_POINT('Ctrl Pts',(4.36064416866912,-2.27919025359464,19.7260008752027));
#27006=CARTESIAN_POINT('Ctrl Pts',(4.42359339549742,-2.14965218903235,19.7341573088828));
#27007=CARTESIAN_POINT('Ctrl Pts',(4.48652981038342,-2.0201404891181,19.7423120824987));
#27008=CARTESIAN_POINT('Ctrl Pts',(4.54378224285713,-1.88784734295421,19.7504668561146));
#27009=CARTESIAN_POINT('Ctrl Pts',(4.59512323347547,-1.75328991660646,19.7586216297305));
#27010=CARTESIAN_POINT('Ctrl Pts',(4.64646604480694,-1.61872771842889,19.7667766925403));
#27011=CARTESIAN_POINT('Ctrl Pts',(4.69189687200536,-1.481901390683,19.7749317553501));
#27012=CARTESIAN_POINT('Ctrl Pts',(4.73123680249645,-1.3433470814362,19.78308681816));
#27013=CARTESIAN_POINT('Ctrl Pts',(4.77057442570357,-1.20480089838923,19.791241402676));
#27014=CARTESIAN_POINT('Ctrl Pts',(4.80382177640447,-1.06452725877274,19.799395987192));
#27015=CARTESIAN_POINT('Ctrl Pts',(4.83085013715846,-0.923076386230346,
19.807550571708));
#27016=CARTESIAN_POINT('Ctrl Pts',(4.85788514323695,-0.781590735887049,
19.8157071611499));
#27017=CARTESIAN_POINT('Ctrl Pts',(4.8786980409756,-0.638927603040939,19.8238637505918));
#27018=CARTESIAN_POINT('Ctrl Pts',(4.89321133906314,-0.495646904321914,
19.8320203400337));
#27019=CARTESIAN_POINT('Ctrl Pts',(4.90306532303982,-0.398364694528591,
19.8375583577317));
#27020=CARTESIAN_POINT('Ctrl Pts',(4.91001632217392,-0.300797983227913,
19.8430963754297));
#27021=CARTESIAN_POINT('Ctrl Pts',(4.91405372330819,-0.203123280154853,
19.8486343931277));
#27022=CARTESIAN_POINT('Ctrl Pts',(4.92000003774551,-0.0592672505635319,
19.8567908268078));
#27023=CARTESIAN_POINT('Ctrl Pts',(4.91962617282005,0.0848769552514978,
19.8649472604878));
#27024=CARTESIAN_POINT('Ctrl Pts',(4.91292774772659,0.228744416583424,19.8731036941679));
#27025=CARTESIAN_POINT('Ctrl Pts',(4.90623068595148,0.372582596831178,19.8812584677838));
#27026=CARTESIAN_POINT('Ctrl Pts',(4.89321164750471,0.516143810896978,19.8894132413997));
#27027=CARTESIAN_POINT('Ctrl Pts',(4.8739183255403,0.658865098834713,19.8975680150156));
#27028=CARTESIAN_POINT('Ctrl Pts',(4.85462431937398,0.801591448118389,19.9057230778255));
#27029=CARTESIAN_POINT('Ctrl Pts',(4.8290556255634,0.943477479570301,19.9138781406353));
#27030=CARTESIAN_POINT('Ctrl Pts',(4.79731164903516,1.0839667912494,19.9220332034451));
#27031=CARTESIAN_POINT('Ctrl Pts',(4.76556953428877,1.22444786324089,19.9301877879611));
#27032=CARTESIAN_POINT('Ctrl Pts',(4.72765293609565,1.36353205314515,19.9383423724771));
#27033=CARTESIAN_POINT('Ctrl Pts',(4.68371207112699,1.50067461405839,19.9464969569931));
#27034=CARTESIAN_POINT('Ctrl Pts',(4.63976040264311,1.63785089351007,19.954653546435));
#27035=CARTESIAN_POINT('Ctrl Pts',(4.5897816096453,1.77308427118075,19.9628101358769));
#27036=CARTESIAN_POINT('Ctrl Pts',(4.53397552910476,1.90584599692084,19.9709667253188));
#27037=CARTESIAN_POINT('Ctrl Pts',(4.4960852976679,1.99598621937554,19.9765047430168));
#27038=CARTESIAN_POINT('Ctrl Pts',(4.45550977342207,2.08498737877925,19.9820427607148));
#27039=CARTESIAN_POINT('Ctrl Pts',(4.41232408519324,2.17268940019591,19.9875807784128));
#27040=CARTESIAN_POINT('Ctrl Pts',(4.34871988217752,2.30185759002574,19.9957372120929));
#27041=CARTESIAN_POINT('Ctrl Pts',(4.27942791172819,2.42825503729542,20.003893645773));
#27042=CARTESIAN_POINT('Ctrl Pts',(4.20471460494752,2.55138357630542,20.0120500794531));
#27043=CARTESIAN_POINT('Ctrl Pts',(4.13001650443106,2.67448705518656,20.020204853069));
#27044=CARTESIAN_POINT('Ctrl Pts',(4.04989944227893,2.79432266716495,20.0283596266849));
#27045=CARTESIAN_POINT('Ctrl Pts',(3.96467463882862,2.91041888234824,20.0365144003008));
#27046=CARTESIAN_POINT('Ctrl Pts',(3.8794468130386,3.02651921466863,20.0446694631106));
#27047=CARTESIAN_POINT('Ctrl Pts',(3.78911107848246,3.13887961288154,20.0528245259204));
#27048=CARTESIAN_POINT('Ctrl Pts',(3.69402092720471,3.24705904656408,20.0609795887303));
#27049=CARTESIAN_POINT('Ctrl Pts',(3.59893635295717,3.35523213553099,20.0691341732463));
#27050=CARTESIAN_POINT('Ctrl Pts',(3.49909814150301,3.45922449983493,20.0772887577623));
#27051=CARTESIAN_POINT('Ctrl Pts',(3.39489882765871,3.55862965373773,20.0854433422783));
#27052=CARTESIAN_POINT('Ctrl Pts',(3.29067389486332,3.65805924787609,20.0935999317202));
#27053=CARTESIAN_POINT('Ctrl Pts',(3.18208595918008,3.75289914670456,20.1017565211621));
#27054=CARTESIAN_POINT('Ctrl Pts',(3.06956347473226,3.84278065170127,20.109913110604));
#27055=CARTESIAN_POINT('Ctrl Pts',(2.99316493650366,3.90380681575401,20.115451128302));
#27056=CARTESIAN_POINT('Ctrl Pts',(2.91495334929489,3.96254800376763,20.1209891459999));
#27057=CARTESIAN_POINT('Ctrl Pts',(2.83507127093721,4.01889959456646,20.1265271636979));
#27058=CARTESIAN_POINT('Ctrl Pts',(2.71742035144111,4.10189463686951,20.134683597378));
#27059=CARTESIAN_POINT('Ctrl Pts',(2.59610049447723,4.17973539837199,20.1428400310581));
#27060=CARTESIAN_POINT('Ctrl Pts',(2.471583999316,4.25211189843648,20.1509964647382));
#27061=CARTESIAN_POINT('Ctrl Pts',(2.34709284677197,4.32447366784274,20.159151238354));
#27062=CARTESIAN_POINT('Ctrl Pts',(2.21940664308317,4.39137322638844,20.1673060119699));
#27063=CARTESIAN_POINT('Ctrl Pts',(2.08902427446046,4.45254541169598,20.1754607855858));
#27064=CARTESIAN_POINT('Ctrl Pts',(1.95863728206862,4.51371976636173,20.1836158483956));
#27065=CARTESIAN_POINT('Ctrl Pts',(1.82555423475462,4.56916619584048,20.1917709112055));
#27066=CARTESIAN_POINT('Ctrl Pts',(1.69029654645842,4.61866654431025,20.1999259740153));
#27067=CARTESIAN_POINT('Ctrl Pts',(1.55504679101553,4.66816398958828,20.2080805585313));
#27068=CARTESIAN_POINT('Ctrl Pts',(1.41762296433932,4.71171593743785,20.2162351430473));
#27069=CARTESIAN_POINT('Ctrl Pts',(1.27856423732369,4.74915324595205,20.2243897275633));
#27070=CARTESIAN_POINT('Ctrl Pts',(1.13947132065162,4.78659975898541,20.2325463170052));
#27071=CARTESIAN_POINT('Ctrl Pts',(0.99874302363769,4.81792854136317,20.2407029064471));
#27072=CARTESIAN_POINT('Ctrl Pts',(0.856931980002171,4.84302081805866,20.248859495889));
#27073=CARTESIAN_POINT('Ctrl Pts',(0.760647610778716,4.8600575309413,20.254397513587));
#27074=CARTESIAN_POINT('Ctrl Pts',(0.663864374974099,4.87422032763894,20.259935531285));
#27075=CARTESIAN_POINT('Ctrl Pts',(0.566757510333805,4.88548554260272,20.265473548983));
#27076=CARTESIAN_POINT('Ctrl Pts',(0.423737797413014,4.90207703503818,20.2736299826631));
#27077=CARTESIAN_POINT('Ctrl Pts',(0.279962296446916,4.91238708678347,20.2817864163432));
#27078=CARTESIAN_POINT('Ctrl Pts',(0.135994049873843,4.91636946139109,20.2899428500233));
#27079=CARTESIAN_POINT('Ctrl Pts',(-0.00794489510218649,4.9203510254732,
20.2980976236392));
#27080=CARTESIAN_POINT('Ctrl Pts',(-0.152076173126647,4.91800747237844,
20.3062523972551));
#27081=CARTESIAN_POINT('Ctrl Pts',(-0.295834837797911,4.90934464172613,
20.314407170871));
#27082=CARTESIAN_POINT('Ctrl Pts',(-0.439598600603923,4.90068150386259,
20.3225622336808));
#27083=CARTESIAN_POINT('Ctrl Pts',(-0.582989389381103,4.88569865639613,
20.3307172964906));
#27084=CARTESIAN_POINT('Ctrl Pts',(-0.725444965208518,4.86445399453563,
20.3388723593005));
#27085=CARTESIAN_POINT('Ctrl Pts',(-0.867892186027029,4.84321057867296,
20.3470269438165));
#27086=CARTESIAN_POINT('Ctrl Pts',(-1.00940397279177,4.81570613345958,20.3551815283325));
#27087=CARTESIAN_POINT('Ctrl Pts',(-1.14942594378057,4.78205008989493,20.3633361128485));
#27088=CARTESIAN_POINT('Ctrl Pts',(-1.2894823412537,4.74838577149136,20.3714927022904));
#27089=CARTESIAN_POINT('Ctrl Pts',(-1.4280478654554,4.70856691052756,20.3796492917323));
#27090=CARTESIAN_POINT('Ctrl Pts',(-1.56458040993998,4.66275360740111,20.3878058811742));
#27091=CARTESIAN_POINT('Ctrl Pts',(-1.65728087661094,4.63164809628951,20.3933438988722));
#27092=CARTESIAN_POINT('Ctrl Pts',(-1.74904442656629,4.59778025841011,20.3988819165702));
#27093=CARTESIAN_POINT('Ctrl Pts',(-1.83970585710855,4.56121315242124,20.4044199342682));
#27094=CARTESIAN_POINT('Ctrl Pts',(-1.97323268672267,4.50735684658475,20.4125763679483));
#27095=CARTESIAN_POINT('Ctrl Pts',(-2.10441792833817,4.44762306864213,20.4207328016284));
#27096=CARTESIAN_POINT('Ctrl Pts',(-2.23274504039072,4.38224059667091,20.4288892353084));
#27097=CARTESIAN_POINT('Ctrl Pts',(-2.36104603425822,4.31687143187597,20.4370440089243));
#27098=CARTESIAN_POINT('Ctrl Pts',(-2.4864897610612,4.24585601839497,20.4451987825402));
#27099=CARTESIAN_POINT('Ctrl Pts',(-2.60858292234846,4.16946977441161,20.4533535561561));
#27100=CARTESIAN_POINT('Ctrl Pts',(-2.73068041344344,4.09308082153164,20.4615086189659));
#27101=CARTESIAN_POINT('Ctrl Pts',(-2.84942681559945,4.01132083132036,20.4696636817758));
#27102=CARTESIAN_POINT('Ctrl Pts',(-2.96435611309558,3.92450963780863,20.4778187445856));
#27103=CARTESIAN_POINT('Ctrl Pts',(-3.07927866999684,3.83770353576704,20.4859733291016));
#27104=CARTESIAN_POINT('Ctrl Pts',(-3.19038430367418,3.74584702557344,20.4941279136176));
#27105=CARTESIAN_POINT('Ctrl Pts',(-3.29723855453186,3.64930143685181,20.5022824981336));
#27106=CARTESIAN_POINT('Ctrl Pts',(-3.40411907709664,3.55273211096101,20.5104390875755));
#27107=CARTESIAN_POINT('Ctrl Pts',(-3.50674587961742,3.45147162710822,20.5185956770174));
#27108=CARTESIAN_POINT('Ctrl Pts',(-3.60471952372578,3.34591993594739,20.5267522664593));
#27109=CARTESIAN_POINT('Ctrl Pts',(-3.67123994612487,3.27425430439049,20.5322902841573));
#27110=CARTESIAN_POINT('Ctrl Pts',(-3.7356160460338,3.20061126464044,20.5378283018553));
#27111=CARTESIAN_POINT('Ctrl Pts',(-3.7977329246787,3.12512522874066,20.5433663195533));
#27112=CARTESIAN_POINT('Ctrl Pts',(-3.88921846670772,3.01394963427154,20.5515226944698));
#27113=CARTESIAN_POINT('Ctrl Pts',(-3.97583588714361,2.89873325391861,20.5596790693863));
#27114=CARTESIAN_POINT('Ctrl Pts',(-4.05724106183668,2.77992410483566,20.5678354443027));
#27115=CARTESIAN_POINT('Ctrl Pts',(-4.13863917622222,2.66112526012382,20.5759911118131));
#27116=CARTESIAN_POINT('Ctrl Pts',(-4.21482575387104,2.53873454170662,20.5841467793236));
#27117=CARTESIAN_POINT('Ctrl Pts',(-4.28549929090363,2.41322997042647,20.592302446834));
#27118=CARTESIAN_POINT('Ctrl Pts',(-4.35616260189941,2.28774355890481,20.6004569342682));
#27119=CARTESIAN_POINT('Ctrl Pts',(-4.42131430129921,2.15914448593707,20.6086114217024));
#27120=CARTESIAN_POINT('Ctrl Pts',(-4.48069824727407,2.02793645841655,20.6167659091367));
#27121=CARTESIAN_POINT('Ctrl Pts',(-4.54009265283834,1.89670532057433,20.6249218328613));
#27122=CARTESIAN_POINT('Ctrl Pts',(-4.59371713419027,1.7628646137145,20.6330777565859));
#27123=CARTESIAN_POINT('Ctrl Pts',(-4.64136295801333,1.62693975133738,20.6412336803105));
#27124=CARTESIAN_POINT('Ctrl Pts',(-4.68804206038235,1.49377276929592,20.6492241224502));
#27125=CARTESIAN_POINT('Ctrl Pts',(-4.72898271456912,1.35860569723107,20.6572145645899));
#27126=CARTESIAN_POINT('Ctrl Pts',(-4.76403458704968,1.22194824599669,20.6652050067296));
#27127=CARTESIAN_POINT('Ctrl Pts',(-4.91824999834649,-0.000127533484696671,
18.9851165466282));
#27128=CARTESIAN_POINT('Ctrl Pts',(-4.91825426647613,0.164470247714909,
18.9758954921501));
#27129=CARTESIAN_POINT('Ctrl Pts',(-4.90999572994125,0.32896299265212,18.9666777222489));
#27130=CARTESIAN_POINT('Ctrl Pts',(-4.88721015483374,0.555255832527698,
18.9538611209249));
#27131=CARTESIAN_POINT('Ctrl Pts',(-4.87971668875726,0.617654490600012,
18.9503131614603));
#27132=CARTESIAN_POINT('Ctrl Pts',(-4.86152175443621,0.748010587004119,
18.942864965379));
#27133=CARTESIAN_POINT('Ctrl Pts',(-4.85058607000977,0.815921713384803,
18.9389639209489));
#27134=CARTESIAN_POINT('Ctrl Pts',(-4.8174742604682,0.997232330121885,18.9284851571659));
#27135=CARTESIAN_POINT('Ctrl Pts',(-4.79272528367052,1.11009124993719,18.9218945455044));
#27136=CARTESIAN_POINT('Ctrl Pts',(-4.76403456361785,1.22194833735085,18.9152905258446));
#27137=CARTESIAN_POINT('Ctrl Pts',(-4.76403458707798,1.22194824588636,18.5697043142649));
#27138=CARTESIAN_POINT('Ctrl Pts',(-4.79432870303326,1.10383995719103,18.5766369470779));
#27139=CARTESIAN_POINT('Ctrl Pts',(-4.82022010554556,0.984646307948852,
18.5835959345697));
#27140=CARTESIAN_POINT('Ctrl Pts',(-4.86407035578851,0.739094272467518,
18.5978640165473));
#27141=CARTESIAN_POINT('Ctrl Pts',(-4.88159586539937,0.612750051166033,
18.6051692734577));
#27142=CARTESIAN_POINT('Ctrl Pts',(-4.9013045904696,0.41422223185854,18.6165700499129));
#27143=CARTESIAN_POINT('Ctrl Pts',(-4.90684315277572,0.342428397819731,
18.6206767293436));
#27144=CARTESIAN_POINT('Ctrl Pts',(-4.9128661836028,0.233098512577472,18.6268982956844));
#27145=CARTESIAN_POINT('Ctrl Pts',(-4.91450054511261,0.195636143911848,
18.6290241526574));
#27146=CARTESIAN_POINT('Ctrl Pts',(-4.91740116217215,0.105482254621061,
18.6341254373705));
#27147=CARTESIAN_POINT('Ctrl Pts',(-4.91824916554378,0.0527819592354969,
18.6370962725309));
#27148=CARTESIAN_POINT('Ctrl Pts',(-4.91825239113532,-0.15109410892035,
18.648565606603));
#27149=CARTESIAN_POINT('Ctrl Pts',(-4.91128494426198,-0.302186809004692,
18.6570175820926));
#27150=CARTESIAN_POINT('Ctrl Pts',(-4.89557526009948,-0.472129117360551,
18.6665822613926));
#27151=CARTESIAN_POINT('Ctrl Pts',(-4.89366559728594,-0.491528281524528,
18.66767490211));
#27152=CARTESIAN_POINT('Ctrl Pts',(-4.87921125968558,-0.629917930384619,
18.6754766685217));
#27153=CARTESIAN_POINT('Ctrl Pts',(-4.86244355274141,-0.748425873823323,
18.6821961863013));
#27154=CARTESIAN_POINT('Ctrl Pts',(-4.82919812443932,-0.934240783413535,
18.6928442494526));
#27155=CARTESIAN_POINT('Ctrl Pts',(-4.81559225279241,-1.00201371157166,
18.6967515731883));
#27156=CARTESIAN_POINT('Ctrl Pts',(-4.78333204332524,-1.14682017470983,
18.705159734493));
#27157=CARTESIAN_POINT('Ctrl Pts',(-4.764234892022,-1.22373511563692,18.7096625148899));
#27158=CARTESIAN_POINT('Ctrl Pts',(-4.73063504211087,-1.3463157619462,18.7169034802174));
#27159=CARTESIAN_POINT('Ctrl Pts',(-4.71730889568343,-1.39228976071185,
18.7196339945461));
#27160=CARTESIAN_POINT('Ctrl Pts',(-4.65910698213442,-1.58264450302222,
18.731002471672));
#27161=CARTESIAN_POINT('Ctrl Pts',(-4.60825682523033,-1.72511165143439,
18.7396651084371));
#27162=CARTESIAN_POINT('Ctrl Pts',(-4.52035783396687,-1.93959951023446,
18.7529219600983));
#27163=CARTESIAN_POINT('Ctrl Pts',(-4.48796049259087,-2.01342793443834,
18.7575250466827));
#27164=CARTESIAN_POINT('Ctrl Pts',(-4.43858711514532,-2.11882213030958,
18.7641450405954));
#27165=CARTESIAN_POINT('Ctrl Pts',(-4.42305816029026,-2.15105075479417,
18.7661760726778));
#27166=CARTESIAN_POINT('Ctrl Pts',(-4.38792848024276,-2.22196929406308,
18.7706586022368));
#27167=CARTESIAN_POINT('Ctrl Pts',(-4.36816477377153,-2.26057524984079,
18.7731077697738));
#27168=CARTESIAN_POINT('Ctrl Pts',(-4.33505476251579,-2.32319556431184,
18.7770999383562));
#27169=CARTESIAN_POINT('Ctrl Pts',(-4.3220134108504,-2.34736820962317,18.7786458169949));
#27170=CARTESIAN_POINT('Ctrl Pts',(-4.26925953279816,-2.44321936162507,
18.7847977244603));
#27171=CARTESIAN_POINT('Ctrl Pts',(-4.22796066111486,-2.51401006552931,
18.7893909513149));
#27172=CARTESIAN_POINT('Ctrl Pts',(-4.08579176459759,-2.74428293837395,
18.8045541987433));
#27173=CARTESIAN_POINT('Ctrl Pts',(-3.97751579749123,-2.89899123883298,
18.815109304399));
#27174=CARTESIAN_POINT('Ctrl Pts',(-3.81647353870796,-3.10302923770986,
18.8297596072273));
#27175=CARTESIAN_POINT('Ctrl Pts',(-3.77111590287003,-3.15799705740185,
18.8337844537811));
#27176=CARTESIAN_POINT('Ctrl Pts',(-3.67602973029557,-3.26825874900703,
18.8420300401426));
#27177=CARTESIAN_POINT('Ctrl Pts',(-3.62620924565683,-3.32344943664825,
18.8462506684459));
#27178=CARTESIAN_POINT('Ctrl Pts',(-3.46224163338755,-3.49701328387295,
18.8598400613412));
#27179=CARTESIAN_POINT('Ctrl Pts',(-3.34340424706155,-3.61079851719021,
18.8692445836429));
#27180=CARTESIAN_POINT('Ctrl Pts',(-3.12769534767233,-3.79754120303279,
18.8855774755665));
#27181=CARTESIAN_POINT('Ctrl Pts',(-3.0334103812626,-3.87326984610622,18.8924955985524));
#27182=CARTESIAN_POINT('Ctrl Pts',(-2.90176331872345,-3.971249201631,18.9018392393749));
#27183=CARTESIAN_POINT('Ctrl Pts',(-2.86675735132641,-3.99659266451767,
18.9042947421531));
#27184=CARTESIAN_POINT('Ctrl Pts',(-2.79745069637361,-4.04538981668817,
18.9090973586495));
#27185=CARTESIAN_POINT('Ctrl Pts',(-2.76317777843545,-4.06887672208052,
18.9114446850763));
#27186=CARTESIAN_POINT('Ctrl Pts',(-2.70723318683238,-4.106182140402,18.9152360835218));
#27187=CARTESIAN_POINT('Ctrl Pts',(-2.68574374039819,-4.120269878116,18.9166830139671));
#27188=CARTESIAN_POINT('Ctrl Pts',(-2.53698201416529,-4.2161345852076,18.9266388551767));
#27189=CARTESIAN_POINT('Ctrl Pts',(-2.40610521177728,-4.29217042399064,
18.9350967906375));
#27190=CARTESIAN_POINT('Ctrl Pts',(-2.15667076220081,-4.4220858485639,18.950858366288));
#27191=CARTESIAN_POINT('Ctrl Pts',(-2.03907694281269,-4.4775257288273,18.9581500052383));
#27192=CARTESIAN_POINT('Ctrl Pts',(-1.86096931040973,-4.55302180645849,
18.9690559070836));
#27193=CARTESIAN_POINT('Ctrl Pts',(-1.80203782152275,-4.57666624571895,
18.972642362632));
#27194=CARTESIAN_POINT('Ctrl Pts',(-1.67429179087219,-4.62507040204111,
18.9803769290442));
#27195=CARTESIAN_POINT('Ctrl Pts',(-1.60534940486965,-4.64944968180691,
18.9845268337863));
#27196=CARTESIAN_POINT('Ctrl Pts',(-1.46042235444775,-4.69709062798457,
18.993206967944));
#27197=CARTESIAN_POINT('Ctrl Pts',(-1.38436554835867,-4.72006627853959,
18.9977378139438));
#27198=CARTESIAN_POINT('Ctrl Pts',(-1.13795636709494,-4.78803456660602,
19.0123432878017));
#27199=CARTESIAN_POINT('Ctrl Pts',(-0.965732514575637,-4.82572070531165,
19.0224442742439));
#27200=CARTESIAN_POINT('Ctrl Pts',(-0.73189540278334,-4.86386713407337,
19.0359703616864));
#27201=CARTESIAN_POINT('Ctrl Pts',(-0.671755195955901,-4.87253727159177,
19.0394320181174));
#27202=CARTESIAN_POINT('Ctrl Pts',(-0.574636582512346,-4.8847061131109,
19.0449895497474));
#27203=CARTESIAN_POINT('Ctrl Pts',(-0.537752730431801,-4.88890407504678,
19.0470922966295));
#27204=CARTESIAN_POINT('Ctrl Pts',(-0.439376127973308,-4.89897408978788,
19.0526811382177));
#27205=CARTESIAN_POINT('Ctrl Pts',(-0.377814255559296,-4.90410593696443,
19.0561591307644));
#27206=CARTESIAN_POINT('Ctrl Pts',(-0.221688612512808,-4.9141633361231,
19.0649508945403));
#27207=CARTESIAN_POINT('Ctrl Pts',(-0.127049114941793,-4.91752029420821,
19.0702539036086));
#27208=CARTESIAN_POINT('Ctrl Pts',(0.128110007983465,-4.91919976060268,
19.0845484213874));
#27209=CARTESIAN_POINT('Ctrl Pts',(0.288545404198044,-4.91240055445093,
19.0935356251746));
#27210=CARTESIAN_POINT('Ctrl Pts',(0.520877362957384,-4.89113205091828,
19.1066790941154));
#27211=CARTESIAN_POINT('Ctrl Pts',(0.593238207355761,-4.88288380296367,
19.1107904015576));
#27212=CARTESIAN_POINT('Ctrl Pts',(0.737208516714782,-4.86322536304217,
19.1190162359285));
#27213=CARTESIAN_POINT('Ctrl Pts',(0.808802228264358,-4.85183224348297,
19.1231296527065));
#27214=CARTESIAN_POINT('Ctrl Pts',(0.91991527541282,-4.83162242107554,19.1295543828845));
#27215=CARTESIAN_POINT('Ctrl Pts',(0.959622202801336,-4.82389308921639,
19.1318584369995));
#27216=CARTESIAN_POINT('Ctrl Pts',(1.18717597902908,-4.77667678782321,19.1451110964801));
#27217=CARTESIAN_POINT('Ctrl Pts',(1.37267792339923,-4.72670945843621,19.156112912456));
#27218=CARTESIAN_POINT('Ctrl Pts',(1.62424242056307,-4.6428848850602,19.171271782757));
#27219=CARTESIAN_POINT('Ctrl Pts',(1.6931778874436,-4.61819145541775,19.1754503712101));
#27220=CARTESIAN_POINT('Ctrl Pts',(1.79432833913429,-4.57938886658624,19.1816109367912));
#27221=CARTESIAN_POINT('Ctrl Pts',(1.82698441010816,-4.56645864854688,19.1836043907144));
#27222=CARTESIAN_POINT('Ctrl Pts',(1.90095871697168,-4.53624785186008,19.1881289700401));
#27223=CARTESIAN_POINT('Ctrl Pts',(1.94218511172701,-4.51875045484249,19.1906572438408));
#27224=CARTESIAN_POINT('Ctrl Pts',(2.03430189876892,-4.4781604816573,19.1963286959396));
#27225=CARTESIAN_POINT('Ctrl Pts',(2.0850493284833,-4.45475867932403,19.1994686338295));
#27226=CARTESIAN_POINT('Ctrl Pts',(2.27029906402286,-4.3654730044483,19.211009229151));
#27227=CARTESIAN_POINT('Ctrl Pts',(2.4021705511308,-4.29432057232326,19.2193811843846));
#27228=CARTESIAN_POINT('Ctrl Pts',(2.62338472373952,-4.16157987907467,19.2338548520061));
#27229=CARTESIAN_POINT('Ctrl Pts',(2.71431581368152,-4.10285068484597,19.239937484154));
#27230=CARTESIAN_POINT('Ctrl Pts',(2.85949994390126,-4.00214095390071,19.2499085564038));
#27231=CARTESIAN_POINT('Ctrl Pts',(2.91494352867892,-3.96194096733918,19.2537811969673));
#27232=CARTESIAN_POINT('Ctrl Pts',(3.03517632227392,-3.870874526165,19.2623326010502));
#27233=CARTESIAN_POINT('Ctrl Pts',(3.09956361540195,-3.81951175752819,19.26701442908));
#27234=CARTESIAN_POINT('Ctrl Pts',(3.23858366880941,-3.70278206802622,19.2773610906178));
#27235=CARTESIAN_POINT('Ctrl Pts',(3.31259003083972,-3.63672465910901,19.2830291351357));
#27236=CARTESIAN_POINT('Ctrl Pts',(3.5045930936445,-3.45461787963514,19.298172563015));
#27237=CARTESIAN_POINT('Ctrl Pts',(3.61881712636447,-3.33477447372053,19.3076541905599));
#27238=CARTESIAN_POINT('Ctrl Pts',(3.75403136367206,-3.17776258546909,19.3194478308024));
#27239=CARTESIAN_POINT('Ctrl Pts',(3.78087467785808,-3.14577705156483,19.3218195512954));
#27240=CARTESIAN_POINT('Ctrl Pts',(3.83451221282742,-3.08018602581176,19.3266189163718));
#27241=CARTESIAN_POINT('Ctrl Pts',(3.86127981128248,-3.04656333286735,19.3290460523197));
#27242=CARTESIAN_POINT('Ctrl Pts',(3.90419197598866,-2.991187305484,19.3329947391149));
#27243=CARTESIAN_POINT('Ctrl Pts',(3.92060340974476,-2.96964398473853,19.334519162483));
#27244=CARTESIAN_POINT('Ctrl Pts',(3.98484223628481,-2.88385679413459,19.3405459276595));
#27245=CARTESIAN_POINT('Ctrl Pts',(4.03127548615795,-2.81858399923418,19.3450359004127));
#27246=CARTESIAN_POINT('Ctrl Pts',(4.17122233247975,-2.61131880567306,19.359049186885));
#27247=CARTESIAN_POINT('Ctrl Pts',(4.25898122966773,-2.46559523781207,19.3685590201726));
#27248=CARTESIAN_POINT('Ctrl Pts',(4.37521519296654,-2.24779573884169,19.3824547186311));
#27249=CARTESIAN_POINT('Ctrl Pts',(4.40981659854938,-2.17913080129116,19.386791346997));
#27250=CARTESIAN_POINT('Ctrl Pts',(4.47278107941558,-2.04653356507111,19.3950948936077));
#27251=CARTESIAN_POINT('Ctrl Pts',(4.50141812470357,-1.98275185892781,19.3990587030837));
#27252=CARTESIAN_POINT('Ctrl Pts',(4.58172078126055,-1.79318299274071,19.4107605899651));
#27253=CARTESIAN_POINT('Ctrl Pts',(4.62954064815573,-1.66584006521686,19.4185220974666));
#27254=CARTESIAN_POINT('Ctrl Pts',(4.72685629629543,-1.36996812769256,19.4363425988618));
#27255=CARTESIAN_POINT('Ctrl Pts',(4.77272788172151,-1.20043844764767,19.4464028437742));
#27256=CARTESIAN_POINT('Ctrl Pts',(4.81804093246147,-0.988612762782616,
19.4587299222992));
#27257=CARTESIAN_POINT('Ctrl Pts',(4.82613738011974,-0.948299357519549,
19.4610649764219));
#27258=CARTESIAN_POINT('Ctrl Pts',(4.84180297542768,-0.864893530228911,
19.4658712360023));
#27259=CARTESIAN_POINT('Ctrl Pts',(4.84930456243093,-0.821792061921997,
19.4683415685301));
#27260=CARTESIAN_POINT('Ctrl Pts',(4.86476479252794,-0.725364078129904,
19.4738450608758));
#27261=CARTESIAN_POINT('Ctrl Pts',(4.87242363944781,-0.671995151214585,
19.4768752744007));
#27262=CARTESIAN_POINT('Ctrl Pts',(4.89635685603151,-0.483194833892426,
19.4875578036661));
#27263=CARTESIAN_POINT('Ctrl Pts',(4.90787364274382,-0.347223573507748,
19.4951852407297));
#27264=CARTESIAN_POINT('Ctrl Pts',(4.9188097554043,-0.0924847346240719,
19.5094815563517));
#27265=CARTESIAN_POINT('Ctrl Pts',(4.91960972675315,0.0261240352611648,
19.5161404403524));
#27266=CARTESIAN_POINT('Ctrl Pts',(4.91410453217042,0.213232477211713,19.5266986324756));
#27267=CARTESIAN_POINT('Ctrl Pts',(4.9106513707835,0.281770149642892,19.5305772269907));
#27268=CARTESIAN_POINT('Ctrl Pts',(4.90019267294761,0.428275214564888,19.5389004963521));
#27269=CARTESIAN_POINT('Ctrl Pts',(4.89275753682427,0.506193020379609,19.5433469751185));
#27270=CARTESIAN_POINT('Ctrl Pts',(4.87275435669971,0.673490396800174,19.5529440966326));
#27271=CARTESIAN_POINT('Ctrl Pts',(4.85957896867461,0.762768875663262,19.5580967183268));
#27272=CARTESIAN_POINT('Ctrl Pts',(4.81573103892388,1.01216885011612,19.5725804157951));
#27273=CARTESIAN_POINT('Ctrl Pts',(4.77954362239245,1.17120207407848,19.5819238252465));
#27274=CARTESIAN_POINT('Ctrl Pts',(4.72145928084235,1.37830296625863,19.5941901124877));
#27275=CARTESIAN_POINT('Ctrl Pts',(4.70659556462621,1.42823495549765,19.5971548968754));
#27276=CARTESIAN_POINT('Ctrl Pts',(4.67970196840458,1.51359555077219,19.602232433501));
#27277=CARTESIAN_POINT('Ctrl Pts',(4.66805609797243,1.54913985760844,19.6043490560377));
#27278=CARTESIAN_POINT('Ctrl Pts',(4.63169333064582,1.65598750128358,19.6107225584945));
#27279=CARTESIAN_POINT('Ctrl Pts',(4.60573968511436,1.72685838715588,19.6149655800664));
#27280=CARTESIAN_POINT('Ctrl Pts',(4.52656548317585,1.9285564901575,19.6271272528967));
#27281=CARTESIAN_POINT('Ctrl Pts',(4.4693279356573,2.05772524694976,19.6350230689612));
#27282=CARTESIAN_POINT('Ctrl Pts',(4.35533300492557,2.28770393681237,19.6494179884599));
#27283=CARTESIAN_POINT('Ctrl Pts',(4.30042770271129,2.38931705205794,19.6559042867065));
#27284=CARTESIAN_POINT('Ctrl Pts',(4.2071387682403,2.54831542005669,19.6663043605052));
#27285=CARTESIAN_POINT('Ctrl Pts',(4.17103554398776,2.60698876946897,19.6701989748279));
#27286=CARTESIAN_POINT('Ctrl Pts',(4.09026532004442,2.73227784730404,19.6786484604192));
#27287=CARTESIAN_POINT('Ctrl Pts',(4.04517721981732,2.79859851828699,19.6832056239085));
#27288=CARTESIAN_POINT('Ctrl Pts',(3.90488611654688,2.99447635750198,19.6969337609773));
#27289=CARTESIAN_POINT('Ctrl Pts',(3.80493356569033,3.12049738133075,19.7061344269571));
#27290=CARTESIAN_POINT('Ctrl Pts',(3.627198762198,3.32332340285735,19.7215708197155));
#27291=CARTESIAN_POINT('Ctrl Pts',(3.55270376558751,3.40284376000782,19.7278010753153));
#27292=CARTESIAN_POINT('Ctrl Pts',(3.44588222421833,3.5095364935912,19.7363948210824));
#27293=CARTESIAN_POINT('Ctrl Pts',(3.4157551803352,3.53886525715323,19.7387831016085));
#27294=CARTESIAN_POINT('Ctrl Pts',(3.3543098991227,3.59716665476884,19.743581233846));
#27295=CARTESIAN_POINT('Ctrl Pts',(3.32298328459847,3.62612534105932,19.7459907296958));
#27296=CARTESIAN_POINT('Ctrl Pts',(3.1464425344962,3.78511239205391,19.7593826341135));
#27297=CARTESIAN_POINT('Ctrl Pts',(2.99397369653049,3.90682730708985,19.7702632753973));
#27298=CARTESIAN_POINT('Ctrl Pts',(2.73779672420761,4.08750640222258,19.7878412051488));
#27299=CARTESIAN_POINT('Ctrl Pts',(2.63847195465235,4.15231317731388,19.7945000067143));
#27300=CARTESIAN_POINT('Ctrl Pts',(2.47774168652459,4.24908792361381,19.8050835317234));
#27301=CARTESIAN_POINT('Ctrl Pts',(2.4178365971761,4.28345866027102,19.8089875786432));
#27302=CARTESIAN_POINT('Ctrl Pts',(2.28748222242553,4.35464387717831,19.817405527634));
#27303=CARTESIAN_POINT('Ctrl Pts',(2.2168240648166,4.39103507942887,19.8219214578777));
#27304=CARTESIAN_POINT('Ctrl Pts',(2.0004569245974,4.49591703447775,19.8356201890093));
#27305=CARTESIAN_POINT('Ctrl Pts',(1.85223897866696,4.55898099758762,19.8448332815318));
#27306=CARTESIAN_POINT('Ctrl Pts',(1.59953284735159,4.65214124076494,19.8602499369504));
#27307=CARTESIAN_POINT('Ctrl Pts',(1.49665642634832,4.68625046031451,19.8664476008381));
#27308=CARTESIAN_POINT('Ctrl Pts',(1.35151408767178,4.72910564403863,19.8750637351172));
#27309=CARTESIAN_POINT('Ctrl Pts',(1.3101332551722,4.74073638085314,19.8775058862079));
#27310=CARTESIAN_POINT('Ctrl Pts',(1.22826956602362,4.76259171469625,19.8823065276988));
#27311=CARTESIAN_POINT('Ctrl Pts',(1.18779838140854,4.77284621815424,19.8846651217342));
#27312=CARTESIAN_POINT('Ctrl Pts',(1.12202251238696,4.78862391420492,19.8884788499442));
#27313=CARTESIAN_POINT('Ctrl Pts',(1.09679635259678,4.79446465005718,19.8899368428148));
#27314=CARTESIAN_POINT('Ctrl Pts',(0.998780478637364,4.81634468282167,19.8955861802687));
#27315=CARTESIAN_POINT('Ctrl Pts',(0.925675608253634,4.83092779384029,19.8997664283788));
#27316=CARTESIAN_POINT('Ctrl Pts',(0.658333081801188,4.87796631825089,19.9149796688525));
#27317=CARTESIAN_POINT('Ctrl Pts',(0.462526433117458,4.90041081634733,19.925988357735));
#27318=CARTESIAN_POINT('Ctrl Pts',(0.193718860918683,4.91496510686333,19.9411563286238));
#27319=CARTESIAN_POINT('Ctrl Pts',(0.121457143487274,4.91728146450245,19.945238271405));
#27320=CARTESIAN_POINT('Ctrl Pts',(0.00686639641869532,4.91842716653716,
19.9517264060405));
#27321=CARTESIAN_POINT('Ctrl Pts',(-0.0354419246901917,4.91830425822997,
19.9541251300483));
#27322=CARTESIAN_POINT('Ctrl Pts',(-0.145492786155172,4.91656445772501,
19.9603748387904));
#27323=CARTESIAN_POINT('Ctrl Pts',(-0.213212531446191,4.91409345748516,
19.9642307652372));
#27324=CARTESIAN_POINT('Ctrl Pts',(-0.38688485398336,4.90415960294977,19.974150018255));
#27325=CARTESIAN_POINT('Ctrl Pts',(-0.492685660863038,4.89466258774151,
19.9802224140866));
#27326=CARTESIAN_POINT('Ctrl Pts',(-0.717299590460411,4.86714365382385,
19.9931751076551));
#27327=CARTESIAN_POINT('Ctrl Pts',(-0.83592958645818,4.84817780437051,20.0000530840343));
#27328=CARTESIAN_POINT('Ctrl Pts',(-1.00854683223634,4.81405616478265,20.0100934607818));
#27329=CARTESIAN_POINT('Ctrl Pts',(-1.0631590083135,4.8022907552385,20.0132746103603));
#27330=CARTESIAN_POINT('Ctrl Pts',(-1.12486107586515,4.78789377919472,20.016871114548));
#27331=CARTESIAN_POINT('Ctrl Pts',(-1.13215893972855,4.78617335837082,20.0172965309918));
#27332=CARTESIAN_POINT('Ctrl Pts',(-1.17381060179265,4.7762536724149,20.0197247142577));
#27333=CARTESIAN_POINT('Ctrl Pts',(-1.20807911052451,4.76770126540984,20.0217228261442));
#27334=CARTESIAN_POINT('Ctrl Pts',(-1.24501400374092,4.75805961880605,20.0238781474693));
#27335=CARTESIAN_POINT('Ctrl Pts',(-1.24777446657012,4.75733644870801,20.0240392443418));
#27336=CARTESIAN_POINT('Ctrl Pts',(-1.25347037997348,4.7558389675686,20.0243716748096));
#27337=CARTESIAN_POINT('Ctrl Pts',(-1.25640574714266,4.7550643399938,20.0245430051136));
#27338=CARTESIAN_POINT('Ctrl Pts',(-1.2625548712552,4.75343552784848,20.0249019450786));
#27339=CARTESIAN_POINT('Ctrl Pts',(-1.26576848320394,4.75258080071179,20.025089549177));
#27340=CARTESIAN_POINT('Ctrl Pts',(-1.27259250431573,4.75075839754867,20.0254879613153));
#27341=CARTESIAN_POINT('Ctrl Pts',(-1.27620268261707,4.74978986343968,20.0256987608068));
#27342=CARTESIAN_POINT('Ctrl Pts',(-1.28396402195081,4.74769817347365,20.0261520026911));
#27343=CARTESIAN_POINT('Ctrl Pts',(-1.28811482175121,4.7465736865768,20.0263944322311));
#27344=CARTESIAN_POINT('Ctrl Pts',(-1.29325052438582,4.74517514837672,20.026694430635));
#27345=CARTESIAN_POINT('Ctrl Pts',(-1.29423682104021,4.74490623286286,20.0267520465109));
#27346=CARTESIAN_POINT('Ctrl Pts',(-1.29671403840483,4.74422998534715,20.0268967618399));
#27347=CARTESIAN_POINT('Ctrl Pts',(-1.29820485123214,4.74382225800069,20.0269838576877));
#27348=CARTESIAN_POINT('Ctrl Pts',(-1.30198118215206,4.74278754326246,20.0272044898995));
#27349=CARTESIAN_POINT('Ctrl Pts',(-1.3042664401492,4.74215960637262,20.0273380177192));
#27350=CARTESIAN_POINT('Ctrl Pts',(-1.31012133743681,4.74054626145924,20.0276801506956));
#27351=CARTESIAN_POINT('Ctrl Pts',(-1.31369032037994,4.73955847289722,20.0278887348446));
#27352=CARTESIAN_POINT('Ctrl Pts',(-1.32296552816608,4.73698008912057,20.0284308920981));
#27353=CARTESIAN_POINT('Ctrl Pts',(-1.32867000372478,4.73538321308394,20.0287644114725));
#27354=CARTESIAN_POINT('Ctrl Pts',(-1.39764886320229,4.71593923656379,20.0327983964666));
#27355=CARTESIAN_POINT('Ctrl Pts',(-1.46056254049221,4.69683536009163,20.0364884487407));
#27356=CARTESIAN_POINT('Ctrl Pts',(-1.73234654059603,4.60831842322037,20.052515612393));
#27357=CARTESIAN_POINT('Ctrl Pts',(-1.9368056692472,4.52619111309733,20.0648081656987));
#27358=CARTESIAN_POINT('Ctrl Pts',(-2.18741716397102,4.40542451548976,20.0804891615229));
#27359=CARTESIAN_POINT('Ctrl Pts',(-2.23930825192616,4.37927590823518,20.0837700930237));
#27360=CARTESIAN_POINT('Ctrl Pts',(-2.34594576678927,4.32314883098023,20.0905892351438));
#27361=CARTESIAN_POINT('Ctrl Pts',(-2.4006094166857,4.29303525228549,20.0941279004626));
#27362=CARTESIAN_POINT('Ctrl Pts',(-2.51663105814461,4.22621124387671,20.1017367869762));
#27363=CARTESIAN_POINT('Ctrl Pts',(-2.5777915798545,4.18918653092184,20.1058085437105));
#27364=CARTESIAN_POINT('Ctrl Pts',(-2.74385248774433,4.08364431442169,20.1170377892196));
#27365=CARTESIAN_POINT('Ctrl Pts',(-2.84697544566685,4.01243165993736,20.1242086071037));
#27366=CARTESIAN_POINT('Ctrl Pts',(-2.95642222677594,3.93050651774702,20.1320344171906));
#27367=CARTESIAN_POINT('Ctrl Pts',(-2.965554367429,3.92362092498309,20.1326890742104));
#27368=CARTESIAN_POINT('Ctrl Pts',(-3.05915880171828,3.85253012396034,20.1394164886881));
#27369=CARTESIAN_POINT('Ctrl Pts',(-3.14155717965971,3.78563862674755,20.1454834655101));
#27370=CARTESIAN_POINT('Ctrl Pts',(-3.25274580468659,3.68924287971734,20.1538575485699));
#27371=CARTESIAN_POINT('Ctrl Pts',(-3.28342597606756,3.66196425665762,20.1561888783821));
#27372=CARTESIAN_POINT('Ctrl Pts',(-3.34461570159707,3.60617142332149,20.1608785596103));
#27373=CARTESIAN_POINT('Ctrl Pts',(-3.37511082618469,3.5776463617704,20.1632366772715));
#27374=CARTESIAN_POINT('Ctrl Pts',(-3.41875128830562,3.53577054909075,20.1666456851509));
#27375=CARTESIAN_POINT('Ctrl Pts',(-3.43218921955439,3.52272776580468,20.1677002311345));
#27376=CARTESIAN_POINT('Ctrl Pts',(-3.46132935260226,3.49411948832873,20.16999809171));
#27377=CARTESIAN_POINT('Ctrl Pts',(-3.47700175729448,3.47852420871381,20.1712410694524));
#27378=CARTESIAN_POINT('Ctrl Pts',(-3.56437494627038,3.39040050653644,20.1782128622542));
#27379=CARTESIAN_POINT('Ctrl Pts',(-3.63391166545402,3.31576093242839,20.1839231048122));
#27380=CARTESIAN_POINT('Ctrl Pts',(-3.80576622150275,3.11939030161214,20.1985419915032));
#27381=CARTESIAN_POINT('Ctrl Pts',(-3.90459254113118,2.99476352706129,20.2074487818447));
#27382=CARTESIAN_POINT('Ctrl Pts',(-4.02644777760171,2.82478665607139,20.2192384447823));
#27383=CARTESIAN_POINT('Ctrl Pts',(-4.05506011657345,2.78355685329612,20.22207166518));
#27384=CARTESIAN_POINT('Ctrl Pts',(-4.09776891307631,2.71995796874464,20.2264046753747));
#27385=CARTESIAN_POINT('Ctrl Pts',(-4.11232437550277,2.69790096912222,20.2279007003425));
#27386=CARTESIAN_POINT('Ctrl Pts',(-4.16807613635892,2.611916563205,20.2337074769161));
#27387=CARTESIAN_POINT('Ctrl Pts',(-4.20796496005974,2.54715478901617,20.2380277707696));
#27388=CARTESIAN_POINT('Ctrl Pts',(-4.29074913079805,2.40549444999091,20.247371730651));
#27389=CARTESIAN_POINT('Ctrl Pts',(-4.33311385126951,2.32831608453999,20.2523974351221));
#27390=CARTESIAN_POINT('Ctrl Pts',(-4.44863512482891,2.10377863784714,20.2668379662034));
#27391=CARTESIAN_POINT('Ctrl Pts',(-4.5165012312343,1.95383108247484,20.2762672745679));
#27392=CARTESIAN_POINT('Ctrl Pts',(-4.59635539201891,1.750878122394,20.2887085913383));
#27393=CARTESIAN_POINT('Ctrl Pts',(-4.61516729231499,1.70067282216006,20.2917606471296));
#27394=CARTESIAN_POINT('Ctrl Pts',(-4.64462112157506,1.61797577883822,20.2967425556194));
#27395=CARTESIAN_POINT('Ctrl Pts',(-4.65575158392822,1.58566333095274,20.2986776402141));
#27396=CARTESIAN_POINT('Ctrl Pts',(-4.67952939376046,1.51422529478869,20.3029320526274));
#27397=CARTESIAN_POINT('Ctrl Pts',(-4.69202465932715,1.47505194165565,20.3052497211436));
#27398=CARTESIAN_POINT('Ctrl Pts',(-4.72563968281926,1.36491535679559,20.3117300454252));
#27399=CARTESIAN_POINT('Ctrl Pts',(-4.74564665006456,1.29363767442263,20.3158827199713));
#27400=CARTESIAN_POINT('Ctrl Pts',(-4.76403459893337,1.2219481996655,20.3200311864783));
#27401=CARTESIAN_POINT('Origin',(0.,0.,-3.23514056400928));
#27402=CARTESIAN_POINT('',(-4.76363197251292,1.22184512090322,22.4152102246214));
#27403=CARTESIAN_POINT('',(-4.76399535256163,1.22193798731013,22.0699206410069));
#27404=CARTESIAN_POINT('',(-4.76403458704967,1.22194824599672,-3.23514056400928));
#27405=CARTESIAN_POINT('',(-4.91798113867399,8.40603594123364E-5,20.7351405640093));
#27406=CARTESIAN_POINT('Ctrl Pts',(-4.91792389088375,8.40593809071227E-5,
20.7351405640093));
#27407=CARTESIAN_POINT('Ctrl Pts',(-4.91761499568841,-0.506908622338837,
20.7638467393807));
#27408=CARTESIAN_POINT('Ctrl Pts',(-4.71379420543462,-1.83214221616955,
20.8388683765138));
#27409=CARTESIAN_POINT('Ctrl Pts',(-3.54218620419026,-3.70656535167346,
20.9602054754087));
#27410=CARTESIAN_POINT('Ctrl Pts',(-1.33712299005241,-4.94952643399905,
21.0991518606938));
#27411=CARTESIAN_POINT('Ctrl Pts',(1.1938697653851,-4.98601893244312,21.2380982459789));
#27412=CARTESIAN_POINT('Ctrl Pts',(3.43385157575744,-3.80714764187707,21.377044631264));
#27413=CARTESIAN_POINT('Ctrl Pts',(4.83681713758415,-1.70026756393053,21.5159910165492));
#27414=CARTESIAN_POINT('Ctrl Pts',(5.0607874964779,0.821060123788163,21.6549374018343));
#27415=CARTESIAN_POINT('Ctrl Pts',(4.05116890385901,3.14225083718467,21.7938837871194));
#27416=CARTESIAN_POINT('Ctrl Pts',(2.05406028049099,4.69750424965121,21.9328301724046));
#27417=CARTESIAN_POINT('Ctrl Pts',(-0.443734465247909,5.10772058121166,
22.0717765576897));
#27418=CARTESIAN_POINT('Ctrl Pts',(-2.83336700616869,4.27290781783748,22.2107229429748));
#27419=CARTESIAN_POINT('Ctrl Pts',(-4.23316194614979,2.72698140687266,22.3252008319521));
#27420=CARTESIAN_POINT('Ctrl Pts',(-4.66782063352313,1.59563011253093,22.3933632591676));
#27421=CARTESIAN_POINT('Ctrl Pts',(-4.76363197251275,1.2218451209039,22.4152102246213));
#27422=CARTESIAN_POINT('Ctrl Pts',(-4.76403458704968,1.22194824599669,20.6652050067296));
#27423=CARTESIAN_POINT('Ctrl Pts',(-4.78905017617746,1.12441945767804,20.6709075727659));
#27424=CARTESIAN_POINT('Ctrl Pts',(-4.81106738250268,1.02613190791664,20.6766101388022));
#27425=CARTESIAN_POINT('Ctrl Pts',(-4.8300460831109,0.92727444563358,20.6823127048384));
#27426=CARTESIAN_POINT('Ctrl Pts',(-4.85934880158881,0.774640582730084,
20.6911173480336));
#27427=CARTESIAN_POINT('Ctrl Pts',(-4.88141421064647,0.620601429743954,
20.6999219912287));
#27428=CARTESIAN_POINT('Ctrl Pts',(-4.89613885764341,0.465840476101292,
20.7087266344239));
#27429=CARTESIAN_POINT('Ctrl Pts',(-4.91086350464035,0.311079522458631,
20.717531277619));
#27430=CARTESIAN_POINT('Ctrl Pts',(-4.91824734118169,0.155597140481115,
20.7263359208142));
#27431=CARTESIAN_POINT('Ctrl Pts',(-4.91824999928156,8.40649548998676E-5,
20.7351405640093));
#27432=CARTESIAN_POINT('',(-4.91801076244909,-0.000108722639682,20.3898594359907));
#27433=CARTESIAN_POINT('Ctrl Pts',(-4.76403459893337,1.2219481996655,20.3200311864783));
#27434=CARTESIAN_POINT('Ctrl Pts',(-4.78939679683197,1.1230680766562,20.3257530986544));
#27435=CARTESIAN_POINT('Ctrl Pts',(-4.81167893680868,1.02340456671475,20.3314672887943));
#27436=CARTESIAN_POINT('Ctrl Pts',(-4.85262058922403,0.809145605183855,
20.3436986279325));
#27437=CARTESIAN_POINT('Ctrl Pts',(-4.87035662702895,0.694455932341157,
20.3502142598379));
#27438=CARTESIAN_POINT('Ctrl Pts',(-4.89205212983886,0.511526776241396,
20.3606037104151));
#27439=CARTESIAN_POINT('Ctrl Pts',(-4.89867442481973,0.443646736066814,
20.3644580876923));
#27440=CARTESIAN_POINT('Ctrl Pts',(-4.90824927956457,0.318653304397231,
20.371561197904));
#27441=CARTESIAN_POINT('Ctrl Pts',(-4.91162140275056,0.261583703428601,
20.3748064943107));
#27442=CARTESIAN_POINT('Ctrl Pts',(-4.91683397047562,0.136310000200659,
20.3819382603392));
#27443=CARTESIAN_POINT('Ctrl Pts',(-4.91825161573311,0.0681001683324553,
20.3858266413289));
#27444=CARTESIAN_POINT('Ctrl Pts',(-4.91824999861809,-0.000116589767614233,
20.3897217550049));
#27445=CARTESIAN_POINT('Ctrl Pts',(-4.91801076244909,-0.000108722639682,
20.3898594359907));
#27446=CARTESIAN_POINT('Ctrl Pts',(-4.91822955624353,-0.271374287939473,
20.4052194041072));
#27447=CARTESIAN_POINT('Ctrl Pts',(-4.82960853223233,-1.36088848373683,
20.4669193707278));
#27448=CARTESIAN_POINT('Ctrl Pts',(-4.03599310824848,-3.16208627326169,
20.5749593358526));
#27449=CARTESIAN_POINT('Ctrl Pts',(-2.02999983921845,-4.70819823522251,
20.7139793313651));
#27450=CARTESIAN_POINT('Ctrl Pts',(0.471328207970822,-5.10547546167352,
20.8529993268776));
#27451=CARTESIAN_POINT('Ctrl Pts',(2.85764873209287,-4.25697940955172,20.9920193223901));
#27452=CARTESIAN_POINT('Ctrl Pts',(4.54668210701339,-2.36974930892355,21.1310393179027));
#27453=CARTESIAN_POINT('Ctrl Pts',(5.12629186064678,0.0957169203737284,
21.2700593134152));
#27454=CARTESIAN_POINT('Ctrl Pts',(4.45504898241472,2.53782752244213,21.4090793089277));
#27455=CARTESIAN_POINT('Ctrl Pts',(2.69674163414686,4.36068968490516,21.5480993044402));
#27456=CARTESIAN_POINT('Ctrl Pts',(0.28040964307056,5.11951173467278,21.6871192999527));
#27457=CARTESIAN_POINT('Ctrl Pts',(-2.20434434768312,4.62913555280215,21.8261392954652));
#27458=CARTESIAN_POINT('Ctrl Pts',(-3.99129943177484,3.14228185516009,21.9537397424833));
#27459=CARTESIAN_POINT('Ctrl Pts',(-4.61016782489247,1.81908628318109,22.0350001909972));
#27460=CARTESIAN_POINT('Ctrl Pts',(-4.76399535256163,1.22193798731013,22.0699206410069));
#27461=CARTESIAN_POINT('Origin',(0.,0.,-3.23514056400928));
#27462=CARTESIAN_POINT('',(-4.76403458701365,1.22194824613716,24.1649977190913));
#27463=CARTESIAN_POINT('',(-4.76403458704968,1.22194824599669,23.8199296610182));
#27464=CARTESIAN_POINT('',(-4.76403458704967,1.22194824599672,-3.23514056400928));
#27465=CARTESIAN_POINT('',(-4.91864051099776,-2.23298241357769E-5,22.4851265773791));
#27466=CARTESIAN_POINT('Ctrl Pts',(-4.76403458701365,1.22194824613716,24.1649977190913));
#27467=CARTESIAN_POINT('Ctrl Pts',(-4.75363281635131,1.2625018418874,24.1626119398973));
#27468=CARTESIAN_POINT('Ctrl Pts',(-4.74271348670068,1.30292162016342,24.1602303929971));
#27469=CARTESIAN_POINT('Ctrl Pts',(-4.72112396186882,1.37896855831405,24.1557448825383));
#27470=CARTESIAN_POINT('Ctrl Pts',(-4.71056339189361,1.41462302684786,24.1536402595871));
#27471=CARTESIAN_POINT('Ctrl Pts',(-4.67841977361937,1.51879268596693,24.1474832684845));
#27472=CARTESIAN_POINT('Ctrl Pts',(-4.65573882185894,1.58695904832956,24.1434431493272));
#27473=CARTESIAN_POINT('Ctrl Pts',(-4.58869297343085,1.77463391762388,24.1322545062445));
#27474=CARTESIAN_POINT('Ctrl Pts',(-4.54116335511359,1.89295122427059,24.1251249865935));
#27475=CARTESIAN_POINT('Ctrl Pts',(-4.43836439743762,2.12262151543145,24.1110205962885));
#27476=CARTESIAN_POINT('Ctrl Pts',(-4.3833642138382,2.23399155090376,24.1040515868379));
#27477=CARTESIAN_POINT('Ctrl Pts',(-4.2942992636445,2.39835741281224,24.0935113850455));
#27478=CARTESIAN_POINT('Ctrl Pts',(-4.26333539333574,2.45297689826029,24.0899649190951));
#27479=CARTESIAN_POINT('Ctrl Pts',(-4.19435753355469,2.56939882590294,24.0823029697932));
#27480=CARTESIAN_POINT('Ctrl Pts',(-4.15600446169644,2.63098312326885,24.0781856610526));
#27481=CARTESIAN_POINT('Ctrl Pts',(-4.07315478243788,2.7576818390502,24.0695724340903));
#27482=CARTESIAN_POINT('Ctrl Pts',(-4.02842584521631,2.82262006741788,24.0650758955646));
#27483=CARTESIAN_POINT('Ctrl Pts',(-3.88001568486795,3.02736687603185,24.0506272348809));
#27484=CARTESIAN_POINT('Ctrl Pts',(-3.77046851882402,3.16275812411159,24.0406493719329));
#27485=CARTESIAN_POINT('Ctrl Pts',(-3.61240899686483,3.33819423488402,24.0271664021113));
#27486=CARTESIAN_POINT('Ctrl Pts',(-3.56997135369261,3.38354018417156,24.0236275420042));
#27487=CARTESIAN_POINT('Ctrl Pts',(-3.50106217658194,3.45443167303,24.018013218801));
#27488=CARTESIAN_POINT('Ctrl Pts',(-3.47514349412997,3.48050460217875,24.0159303289431));
#27489=CARTESIAN_POINT('Ctrl Pts',(-3.40708780186065,3.54744714701854,24.0105342388606));
#27490=CARTESIAN_POINT('Ctrl Pts',(-3.36450710698333,3.58785738281828,24.007228026295));
#27491=CARTESIAN_POINT('Ctrl Pts',(-3.28824842792264,3.65767725505637,24.0014158383051));
#27492=CARTESIAN_POINT('Ctrl Pts',(-3.25487391797626,3.68740782044014,23.9989074307868));
#27493=CARTESIAN_POINT('Ctrl Pts',(-3.08472340505253,3.8348705229166,23.9862805043539));
#27494=CARTESIAN_POINT('Ctrl Pts',(-2.94194688341965,3.94546558139833,23.9761961129164));
#27495=CARTESIAN_POINT('Ctrl Pts',(-2.72468937698022,4.09539053348215,23.9613546417961));
#27496=CARTESIAN_POINT('Ctrl Pts',(-2.65476613328415,4.14105932982072,23.9566497862757));
#27497=CARTESIAN_POINT('Ctrl Pts',(-2.52677338651492,4.22008027152164,23.9481483585877));
#27498=CARTESIAN_POINT('Ctrl Pts',(-2.46912088535045,4.25406901290821,23.9443579139273));
#27499=CARTESIAN_POINT('Ctrl Pts',(-2.32298067850495,4.33625339992634,23.9348382281556));
#27500=CARTESIAN_POINT('Ctrl Pts',(-2.23367237938419,4.38292597379616,23.9290994079972));
#27501=CARTESIAN_POINT('Ctrl Pts',(-2.00697061889581,4.49267076134325,23.9147146020704));
#27502=CARTESIAN_POINT('Ctrl Pts',(-1.86798403862433,4.55221451091376,23.9060558570609));
#27503=CARTESIAN_POINT('Ctrl Pts',(-1.65123355061661,4.63347259059811,23.8928175669778));
#27504=CARTESIAN_POINT('Ctrl Pts',(-1.57530854822261,4.65983301047621,23.8882290463911));
#27505=CARTESIAN_POINT('Ctrl Pts',(-1.46498286364453,4.69513224505472,23.8816404530144));
#27506=CARTESIAN_POINT('Ctrl Pts',(-1.43107824495466,4.70557718933143,23.8796263111362));
#27507=CARTESIAN_POINT('Ctrl Pts',(-1.35609481771983,4.72779183585825,23.8751967505451));
#27508=CARTESIAN_POINT('Ctrl Pts',(-1.31496953878995,4.73939489460497,23.8727835443422));
#27509=CARTESIAN_POINT('Ctrl Pts',(-1.24767502016877,4.75743796427594,23.8688565960864));
#27510=CARTESIAN_POINT('Ctrl Pts',(-1.22159506721075,4.7642013435836,23.8673400220984));
#27511=CARTESIAN_POINT('Ctrl Pts',(-1.11817175512541,4.79011729165105,23.8613442359394));
#27512=CARTESIAN_POINT('Ctrl Pts',(-1.04042305655069,4.80760353522793,23.8568772516731));
#27513=CARTESIAN_POINT('Ctrl Pts',(-0.771537192694124,4.86124941311935,
23.8415133493799));
#27514=CARTESIAN_POINT('Ctrl Pts',(-0.578703172797429,4.88795632202422,
23.8306342908209));
#27515=CARTESIAN_POINT('Ctrl Pts',(-0.321709385304962,4.90812496302579,
23.816102948643));
#27516=CARTESIAN_POINT('Ctrl Pts',(-0.258532865706478,4.9118579204495,23.8125288830362));
#27517=CARTESIAN_POINT('Ctrl Pts',(-0.123602951670436,4.91722017990039,
23.8048844338932));
#27518=CARTESIAN_POINT('Ctrl Pts',(-0.0518503582946505,4.91850011356894,
23.8008125732088));
#27519=CARTESIAN_POINT('Ctrl Pts',(0.0598864713917693,4.91804791575499,
23.794456347513));
#27520=CARTESIAN_POINT('Ctrl Pts',(0.0998653794617415,4.91739855741258,
23.7921791006398));
#27521=CARTESIAN_POINT('Ctrl Pts',(0.321386503889912,4.91109789840972,23.7795426890686));
#27522=CARTESIAN_POINT('Ctrl Pts',(0.502514915989395,4.89588089161654,23.7691361681624));
#27523=CARTESIAN_POINT('Ctrl Pts',(0.761297277986533,4.85962540384258,23.7541911402653));
#27524=CARTESIAN_POINT('Ctrl Pts',(0.839930976755452,4.84665335834015,23.7496405674957));
#27525=CARTESIAN_POINT('Ctrl Pts',(0.953713289547652,4.82503053232281,23.7430513774998));
#27526=CARTESIAN_POINT('Ctrl Pts',(0.989136094779115,4.81789357476211,23.7409994147684));
#27527=CARTESIAN_POINT('Ctrl Pts',(1.06520524643603,4.80169291519703,23.7365932149715));
#27528=CARTESIAN_POINT('Ctrl Pts',(1.10582174120222,4.79250199762617,23.7342407882073));
#27529=CARTESIAN_POINT('Ctrl Pts',(1.17149689281986,4.77676130302535,23.7304332299061));
#27530=CARTESIAN_POINT('Ctrl Pts',(1.19662892648629,4.77052751149441,23.7289752823241));
#27531=CARTESIAN_POINT('Ctrl Pts',(1.37184094741916,4.72559592054621,23.7188005555667));
#27532=CARTESIAN_POINT('Ctrl Pts',(1.52006847974102,4.68002103336966,23.7101365849302));
#27533=CARTESIAN_POINT('Ctrl Pts',(1.7840260981573,4.58499693561589,23.6944121539718));
#27534=CARTESIAN_POINT('Ctrl Pts',(1.90048230307274,4.5379634727758,23.6873660977633));
#27535=CARTESIAN_POINT('Ctrl Pts',(2.07234468652241,4.46077581854696,23.6767441982816));
#27536=CARTESIAN_POINT('Ctrl Pts',(2.12918001775185,4.43392892917132,23.6731938069074));
#27537=CARTESIAN_POINT('Ctrl Pts',(2.25036205575529,4.37381965057869,23.6655349451547));
#27538=CARTESIAN_POINT('Ctrl Pts',(2.31452007068354,4.3402101787422,23.6614247018392));
#27539=CARTESIAN_POINT('Ctrl Pts',(2.53293709721332,4.21957074634783,23.6472282145625));
#27540=CARTESIAN_POINT('Ctrl Pts',(2.68322244101844,4.12563492453167,23.6370973052321));
#27541=CARTESIAN_POINT('Ctrl Pts',(2.83547195790068,4.01862697669044,23.6264448788333));
#27542=CARTESIAN_POINT('Ctrl Pts',(2.84281822078119,4.01343351327193,23.6259299073577));
#27543=CARTESIAN_POINT('Ctrl Pts',(2.9386852051657,3.94526477267804,23.6191969317627));
#27544=CARTESIAN_POINT('Ctrl Pts',(3.02511083142521,3.87939295830927,23.6129841521701));
#27545=CARTESIAN_POINT('Ctrl Pts',(3.14125222771581,3.78462940989133,23.6044530596793));
#27546=CARTESIAN_POINT('Ctrl Pts',(3.17289056748573,3.75814459969224,23.6021096300691));
#27547=CARTESIAN_POINT('Ctrl Pts',(3.23646205837304,3.70355311573759,23.5973632752029));
#27548=CARTESIAN_POINT('Ctrl Pts',(3.26837136175739,3.67542392582332,23.5949608627785));
#27549=CARTESIAN_POINT('Ctrl Pts',(3.31975080072493,3.62893283370501,23.5910551649576));
#27550=CARTESIAN_POINT('Ctrl Pts',(3.339442876036,3.61081987622443,23.5895490504008));
#27551=CARTESIAN_POINT('Ctrl Pts',(3.47124609185732,3.48758553047829,23.5794015412238));
#27552=CARTESIAN_POINT('Ctrl Pts',(3.57852518150923,3.37741919192519,23.5708103348311));
#27553=CARTESIAN_POINT('Ctrl Pts',(3.76283625345998,3.16948967793822,23.5552355975117));
#27554=CARTESIAN_POINT('Ctrl Pts',(3.84165295118343,3.073483943344,23.5482663935508));
#27555=CARTESIAN_POINT('Ctrl Pts',(3.9547215125295,2.92460291687742,23.5377259876296));
#27556=CARTESIAN_POINT('Ctrl Pts',(3.99173069379903,2.87388420528602,23.5341795139011));
#27557=CARTESIAN_POINT('Ctrl Pts',(4.06938876642955,2.7630636036435,23.5265175709376));
#27558=CARTESIAN_POINT('Ctrl Pts',(4.10969918976051,2.70274264674488,23.5224002764183));
#27559=CARTESIAN_POINT('Ctrl Pts',(4.19100506168466,2.57504864015972,23.5137870931857));
#27560=CARTESIAN_POINT('Ctrl Pts',(4.23174425468662,2.50753650371374,23.5092905842304));
#27561=CARTESIAN_POINT('Ctrl Pts',(4.35714970240799,2.28795039716937,23.4948421782815));
#27562=CARTESIAN_POINT('Ctrl Pts',(4.43537438191799,2.132351877021,23.4848645416041));
#27563=CARTESIAN_POINT('Ctrl Pts',(4.53009948837585,1.91604763835229,23.471381600174));
#27564=CARTESIAN_POINT('Ctrl Pts',(4.55393260056208,1.85869253245921,23.4678425476648));
#27565=CARTESIAN_POINT('Ctrl Pts',(4.5901345631387,1.76669160982141,23.4622280295423));
#27566=CARTESIAN_POINT('Ctrl Pts',(4.60321186606939,1.73233227490345,23.46014513598));
#27567=CARTESIAN_POINT('Ctrl Pts',(4.63616511915414,1.64274197553066,23.454749205338));
#27568=CARTESIAN_POINT('Ctrl Pts',(4.65543978121025,1.5872960579709,23.4514431548043));
#27569=CARTESIAN_POINT('Ctrl Pts',(4.68763389884376,1.4890496034675,23.445631338234));
#27570=CARTESIAN_POINT('Ctrl Pts',(4.70097081569815,1.44639334601556,23.4431231398826));
#27571=CARTESIAN_POINT('Ctrl Pts',(4.7652246568399,1.23060301940565,23.4304965113166));
#27572=CARTESIAN_POINT('Ctrl Pts',(4.80716615658716,1.05494221183952,23.4204122135255));
#27573=CARTESIAN_POINT('Ctrl Pts',(4.85425605322918,0.795207327790857,23.4055706064557));
#27574=CARTESIAN_POINT('Ctrl Pts',(4.86705781472965,0.712674206983198,23.4008655168694));
#27575=CARTESIAN_POINT('Ctrl Pts',(4.88632195994068,0.563488146704479,23.3923638794242));
#27576=CARTESIAN_POINT('Ctrl Pts',(4.8935364384407,0.496952896665293,23.3885734606663));
#27577=CARTESIAN_POINT('Ctrl Pts',(4.90820438091778,0.329940639013733,23.3790542855101));
#27578=CARTESIAN_POINT('Ctrl Pts',(4.9139324602483,0.229343531533057,23.3733159529812));
#27579=CARTESIAN_POINT('Ctrl Pts',(4.92051936296306,-0.0224000320528518,
23.3589333561474));
#27580=CARTESIAN_POINT('Ctrl Pts',(4.91750898769162,-0.173544246678037,
23.3502763392639));
#27581=CARTESIAN_POINT('Ctrl Pts',(4.90224722590296,-0.404490236563302,
23.3370398408738));
#27582=CARTESIAN_POINT('Ctrl Pts',(4.89498422490087,-0.48453057107198,23.3324514030228));
#27583=CARTESIAN_POINT('Ctrl Pts',(4.88169115623406,-0.599611490484468,
23.3258621569221));
#27584=CARTESIAN_POINT('Ctrl Pts',(4.87723747182906,-0.634820578031856,
23.3238472890544));
#27585=CARTESIAN_POINT('Ctrl Pts',(4.8665856149228,-0.712285944216729,23.3194183094497));
#27586=CARTESIAN_POINT('Ctrl Pts',(4.86021732393673,-0.754516026889388,
23.3170064016834));
#27587=CARTESIAN_POINT('Ctrl Pts',(4.84893936266278,-0.823222195517016,
23.3130820111139));
#27588=CARTESIAN_POINT('Ctrl Pts',(4.84436089359634,-0.849750121563693,
23.3115666967033));
#27589=CARTESIAN_POINT('Ctrl Pts',(4.82538841979017,-0.95453716599194,23.3055781944255));
#27590=CARTESIAN_POINT('Ctrl Pts',(4.80931385542178,-1.03248001900831,23.3011172095604));
#27591=CARTESIAN_POINT('Ctrl Pts',(4.74833253332805,-1.29570836995476,23.2859765806535));
#27592=CARTESIAN_POINT('Ctrl Pts',(4.69454966853988,-1.47875772149309,23.2753142299341));
#27593=CARTESIAN_POINT('Ctrl Pts',(4.60632854032987,-1.72509903637105,23.2605680546434));
#27594=CARTESIAN_POINT('Ctrl Pts',(4.58093203916142,-1.7914493593339,23.2565561602073));
#27595=CARTESIAN_POINT('Ctrl Pts',(4.52656720824242,-1.92475748393204,23.2484040448458));
#27596=CARTESIAN_POINT('Ctrl Pts',(4.49752840221002,-1.99166768470933,23.2442642583583));
#27597=CARTESIAN_POINT('Ctrl Pts',(4.43368498174905,-2.13024994013496,23.2355819738333));
#27598=CARTESIAN_POINT('Ctrl Pts',(4.39860502560117,-2.20177223577574,23.2310387574657));
#27599=CARTESIAN_POINT('Ctrl Pts',(4.28249288404842,-2.42464499236741,23.2166785295574));
#27600=CARTESIAN_POINT('Ctrl Pts',(4.19526652132877,-2.57262266417517,23.2068375171293));
#27601=CARTESIAN_POINT('Ctrl Pts',(4.06618769753098,-2.76751841958359,23.1934900134867));
#27602=CARTESIAN_POINT('Ctrl Pts',(4.03091451386379,-2.81864664509382,23.1899506528104));
#27603=CARTESIAN_POINT('Ctrl Pts',(3.97323641326655,-2.89895273549963,23.1843358224786));
#27604=CARTESIAN_POINT('Ctrl Pts',(3.95145650061225,-2.92857066242305,23.1822529229725));
#27605=CARTESIAN_POINT('Ctrl Pts',(3.89404838838512,-3.00483191117359,23.1768572476015));
#27606=CARTESIAN_POINT('Ctrl Pts',(3.85791368935393,-3.05108665115517,23.1735514565006));
#27607=CARTESIAN_POINT('Ctrl Pts',(3.79282483510735,-3.13139897259176,23.1677402345912));
#27608=CARTESIAN_POINT('Ctrl Pts',(3.76421825590976,-3.16572909572056,23.1652323711145));
#27609=CARTESIAN_POINT('Ctrl Pts',(3.61774591813145,-3.33671445362707,23.1526062195923));
#27610=CARTESIAN_POINT('Ctrl Pts',(3.49289063671655,-3.46719823189656,23.1425220718892));
#27611=CARTESIAN_POINT('Ctrl Pts',(3.30017937434332,-3.64759835310928,23.1276802471827));
#27612=CARTESIAN_POINT('Ctrl Pts',(3.23776745369198,-3.70310941466093,23.1229747827119));
#27613=CARTESIAN_POINT('Ctrl Pts',(3.12285485791498,-3.80018928904171,23.1144728092698));
#27614=CARTESIAN_POINT('Ctrl Pts',(3.07086110155305,-3.84232651648697,23.1106824319524));
#27615=CARTESIAN_POINT('Ctrl Pts',(2.93849395500464,-3.94519728383304,23.101164074049));
#27616=CARTESIAN_POINT('Ctrl Pts',(2.85708462695806,-4.00454683774597,23.0954265219999));
#27617=CARTESIAN_POINT('Ctrl Pts',(2.64918151914229,-4.14654498702786,23.0810474600151));
#27618=CARTESIAN_POINT('Ctrl Pts',(2.52059365296332,-4.22594431743793,23.0723932081582));
#27619=CARTESIAN_POINT('Ctrl Pts',(2.31831684224585,-4.33832301567438,23.0591596520405));
#27620=CARTESIAN_POINT('Ctrl Pts',(2.24713021611858,-4.37561945122382,23.0545714218355));
#27621=CARTESIAN_POINT('Ctrl Pts',(2.14321350561366,-4.4268589108072,23.0479811817797));
#27622=CARTESIAN_POINT('Ctrl Pts',(2.1111963325242,-4.44221724263565,23.0459651282934));
#27623=CARTESIAN_POINT('Ctrl Pts',(2.04034726338444,-4.47526386255296,23.0415370849775));
#27624=CARTESIAN_POINT('Ctrl Pts',(2.00144573507179,-4.49279630309929,23.0391272852502));
#27625=CARTESIAN_POINT('Ctrl Pts',(1.93767017584439,-4.52054643242715,23.0352070463384));
#27626=CARTESIAN_POINT('Ctrl Pts',(1.9129320222673,-4.53107016573018,23.033693776082));
#27627=CARTESIAN_POINT('Ctrl Pts',(1.8147959479843,-4.57187079203813,23.0277170828895));
#27628=CARTESIAN_POINT('Ctrl Pts',(1.74075538953395,-4.60057145273527,23.0232658226211));
#27629=CARTESIAN_POINT('Ctrl Pts',(1.48370490107368,-4.69311873618654,23.007956816658));
#27630=CARTESIAN_POINT('Ctrl Pts',(1.2976383096565,-4.74793401604108,22.9971170986894));
#27631=CARTESIAN_POINT('Ctrl Pts',(1.04696862063117,-4.8059412063301,22.9826144773261));
#27632=CARTESIAN_POINT('Ctrl Pts',(0.984841278992134,-4.81905610235706,
22.9790288368528));
#27633=CARTESIAN_POINT('Ctrl Pts',(0.860415936866699,-4.84281525631282,
22.971858305144));
#27634=CARTESIAN_POINT('Ctrl Pts',(0.798131820792461,-4.85346893238568,
22.9682741627323));
#27635=CARTESIAN_POINT('Ctrl Pts',(0.705729951494024,-4.86744744390977,
22.9629613243532));
#27636=CARTESIAN_POINT('Ctrl Pts',(0.675758631029433,-4.87169884588969,
22.9612387632728));
#27637=CARTESIAN_POINT('Ctrl Pts',(0.557159970118804,-4.88740643928316,
22.9544246404962));
#27638=CARTESIAN_POINT('Ctrl Pts',(0.468267178940948,-4.89672283928233,
22.9493217290823));
#27639=CARTESIAN_POINT('Ctrl Pts',(0.2139257255232,-4.91638973230299,22.9347315331563));
#27640=CARTESIAN_POINT('Ctrl Pts',(0.0481401655254922,-4.92080634360156,
22.9252307160508));
#27641=CARTESIAN_POINT('Ctrl Pts',(-0.167760106194562,-4.91564461031795,
22.9129164476526));
#27642=CARTESIAN_POINT('Ctrl Pts',(-0.21794760137163,-4.91367523468527,
22.9100583946967));
#27643=CARTESIAN_POINT('Ctrl Pts',(-0.304791773108721,-4.90893426256406,
22.9051238755183));
#27644=CARTESIAN_POINT('Ctrl Pts',(-0.341463338215585,-4.90651978849226,
22.9030440026842));
#27645=CARTESIAN_POINT('Ctrl Pts',(-0.418590724273965,-4.90057279488081,
22.89867524763));
#27646=CARTESIAN_POINT('Ctrl Pts',(-0.459036625533927,-4.89694979853538,
22.896387288996));
#27647=CARTESIAN_POINT('Ctrl Pts',(-0.536871489671071,-4.88900483651822,
22.8919857319605));
#27648=CARTESIAN_POINT('Ctrl Pts',(-0.574264778111661,-4.88475375777505,
22.8898717846808));
#27649=CARTESIAN_POINT('Ctrl Pts',(-0.757134858939948,-4.86183517300296,
22.8795283768062));
#27650=CARTESIAN_POINT('Ctrl Pts',(-0.901775472957081,-4.83709578108482,
22.8713287570633));
#27651=CARTESIAN_POINT('Ctrl Pts',(-1.15277484017265,-4.78251363791775,
22.856919624179));
#27652=CARTESIAN_POINT('Ctrl Pts',(-1.25963713659576,-4.75548529360846,
22.8507269206461));
#27653=CARTESIAN_POINT('Ctrl Pts',(-1.42964710344575,-4.70635216661582,
22.8407415713474));
#27654=CARTESIAN_POINT('Ctrl Pts',(-1.4934092709226,-4.68650938084254,22.8369660186691));
#27655=CARTESIAN_POINT('Ctrl Pts',(-1.6166334908108,-4.64539179256364,22.829602742714));
#27656=CARTESIAN_POINT('Ctrl Pts',(-1.6761290646742,-4.62425777839593,22.8260166909005));
#27657=CARTESIAN_POINT('Ctrl Pts',(-1.88808217620377,-4.54433981502277,
22.8131231209283));
#27658=CARTESIAN_POINT('Ctrl Pts',(-2.03799447773967,-4.4791133116889,22.803777682958));
#27659=CARTESIAN_POINT('Ctrl Pts',(-2.29152579983446,-4.35343471114599,
22.7875790851894));
#27660=CARTESIAN_POINT('Ctrl Pts',(-2.39669943443484,-4.29643067537482,
22.7807357706578));
#27661=CARTESIAN_POINT('Ctrl Pts',(-2.53645120613345,-4.21395541850418,
22.7714961598607));
#27662=CARTESIAN_POINT('Ctrl Pts',(-2.57292747797696,-4.19178353912988,
22.7690706409353));
#27663=CARTESIAN_POINT('Ctrl Pts',(-2.63730457530052,-4.15149537459055,
22.7647670691262));
#27664=CARTESIAN_POINT('Ctrl Pts',(-2.66531873635941,-4.13356569122878,
22.7628866298749));
#27665=CARTESIAN_POINT('Ctrl Pts',(-2.72970513775886,-4.09143025965455,
22.7585437853213));
#27666=CARTESIAN_POINT('Ctrl Pts',(-2.76594103862293,-4.06702125969586,
22.7560839473428));
#27667=CARTESIAN_POINT('Ctrl Pts',(-2.92534251259589,-3.95653043515634,
22.7451801263919));
#27668=CARTESIAN_POINT('Ctrl Pts',(-3.04485072135958,-3.86531324879298,
22.7367796378347));
#27669=CARTESIAN_POINT('Ctrl Pts',(-3.25457854607934,-3.68946293481423,
22.7214378998592));
#27670=CARTESIAN_POINT('Ctrl Pts',(-3.34614161669123,-3.60662640235896,
22.7145099320098));
#27671=CARTESIAN_POINT('Ctrl Pts',(-3.47940410689395,-3.47661721540432,
22.7040130174062));
#27672=CARTESIAN_POINT('Ctrl Pts',(-3.5234745644396,-3.4319450883633,22.7004684122164));
#27673=CARTESIAN_POINT('Ctrl Pts',(-3.61003285808672,-3.34077992829052,
22.6933505050603));
#27674=CARTESIAN_POINT('Ctrl Pts',(-3.65250658299013,-3.29428950127429,
22.6897778035394));
#27675=CARTESIAN_POINT('Ctrl Pts',(-3.83334312377685,-3.08855357988104,
22.6742021947446));
#27676=CARTESIAN_POINT('Ctrl Pts',(-3.96227107642496,-2.92131620382396,
22.6621260149102));
#27677=CARTESIAN_POINT('Ctrl Pts',(-4.13011525046187,-2.67195927118062,
22.6449263897562));
#27678=CARTESIAN_POINT('Ctrl Pts',(-4.17812756394652,-2.59624125284309,
22.6398030806088));
#27679=CARTESIAN_POINT('Ctrl Pts',(-4.24558769299956,-2.4831305166957,22.6323054232603));
#27680=CARTESIAN_POINT('Ctrl Pts',(-4.26666730757667,-2.44673295685174,
22.629915789141));
#27681=CARTESIAN_POINT('Ctrl Pts',(-4.30342916044187,-2.3813372136461,22.6256651581413));
#27682=CARTESIAN_POINT('Ctrl Pts',(-4.31929155749443,-2.35244339550757,
22.6238018171683));
#27683=CARTESIAN_POINT('Ctrl Pts',(-4.35569080675922,-2.28453159848305,
22.61945347387));
#27684=CARTESIAN_POINT('Ctrl Pts',(-4.37599585612377,-2.24539246989924,
22.6169711924386));
#27685=CARTESIAN_POINT('Ctrl Pts',(-4.45885387989294,-2.0802848570807,22.6065864823423));
#27686=CARTESIAN_POINT('Ctrl Pts',(-4.51651531885476,-1.95193566529595,
22.5987212159425));
#27687=CARTESIAN_POINT('Ctrl Pts',(-4.59309786003349,-1.75983309877459,
22.587131146069));
#27688=CARTESIAN_POINT('Ctrl Pts',(-4.61635581570514,-1.69788674781731,
22.5834209993106));
#27689=CARTESIAN_POINT('Ctrl Pts',(-4.66888749080919,-1.54890350032694,
22.574547255183));
#27690=CARTESIAN_POINT('Ctrl Pts',(-4.69698729231255,-1.46147957403543,
22.5693793727349));
#27691=CARTESIAN_POINT('Ctrl Pts',(-4.74013326567671,-1.3131077424678,22.5606524284325));
#27692=CARTESIAN_POINT('Ctrl Pts',(-4.75648980741909,-1.25256533697481,
22.5571035667272));
#27693=CARTESIAN_POINT('Ctrl Pts',(-4.78723653981814,-1.12945520095368,
22.5499059326125));
#27694=CARTESIAN_POINT('Ctrl Pts',(-4.80156835113523,-1.06688518485319,
22.5462574622833));
#27695=CARTESIAN_POINT('Ctrl Pts',(-4.84640628900657,-0.851876690113653,
22.5337472436324));
#27696=CARTESIAN_POINT('Ctrl Pts',(-4.87090836043322,-0.698282660932549,
22.5248535705399));
#27697=CARTESIAN_POINT('Ctrl Pts',(-4.90112114811131,-0.426700947045144,
22.509211331776));
#27698=CARTESIAN_POINT('Ctrl Pts',(-4.90993574011038,-0.309182287191449,
22.5024706214595));
#27699=CARTESIAN_POINT('Ctrl Pts',(-4.9158821497358,-0.156545822731047,
22.4937744193805));
#27700=CARTESIAN_POINT('Ctrl Pts',(-4.91687024323224,-0.121618032780329,
22.4917885365338));
#27701=CARTESIAN_POINT('Ctrl Pts',(-4.91799513852044,-0.0578028651488844,
22.4881688539813));
#27702=CARTESIAN_POINT('Ctrl Pts',(-4.91824979373262,-0.028919407406132,
22.4865339698279));
#27703=CARTESIAN_POINT('Ctrl Pts',(-4.91824999987475,-3.51006693910429E-5,
22.4849018564489));
#27704=CARTESIAN_POINT('Ctrl Pts',(-4.76363197251275,1.2218451209039,22.4152102246213));
#27705=CARTESIAN_POINT('Ctrl Pts',(-4.86586003699209,0.823026811626357,
22.4385203361033));
#27706=CARTESIAN_POINT('Ctrl Pts',(-4.91856347066883,0.411490142340121,
22.4618304475853));
#27707=CARTESIAN_POINT('Ctrl Pts',(-4.9186648078212,-2.15352476078406E-5,
22.4851405590673));
#27708=CARTESIAN_POINT('',(-4.9182499983453,0.000127579104957042,22.1398594359908));
#27709=CARTESIAN_POINT('Ctrl Pts',(-4.76399535256163,1.22193798731013,22.0699206410069));
#27710=CARTESIAN_POINT('Ctrl Pts',(-4.81429942686512,1.02666089548625,22.0813401895013));
#27711=CARTESIAN_POINT('Ctrl Pts',(-4.89251683443142,0.621776568813317,
22.1046531201869));
#27712=CARTESIAN_POINT('Ctrl Pts',(-4.91839361835249,0.210150187564921,
22.1279660508726));
#27713=CARTESIAN_POINT('Ctrl Pts',(-4.91818349699392,0.000127629067394636,
22.1398594330638));
#27714=CARTESIAN_POINT('Ctrl Pts',(-4.9182499983453,0.000127579104957042,
22.1398594359908));
#27715=CARTESIAN_POINT('Ctrl Pts',(-4.91825372288393,-0.143455589280298,
22.1479903075752));
#27716=CARTESIAN_POINT('Ctrl Pts',(-4.91196546422664,-0.287055776384316,
22.1561211791597));
#27717=CARTESIAN_POINT('Ctrl Pts',(-4.89940681158052,-0.430111563595313,
22.1642520507441));
#27718=CARTESIAN_POINT('Ctrl Pts',(-4.88684771079342,-0.573172455586439,
22.1723832124693));
#27719=CARTESIAN_POINT('Ctrl Pts',(-4.86801779513648,-0.715688571369777,
22.1805143741945));
#27720=CARTESIAN_POINT('Ctrl Pts',(-4.84299060350325,-0.857102722478036,
22.1886455359196));
#27721=CARTESIAN_POINT('Ctrl Pts',(-4.81796399284641,-0.998513590825499,
22.1967765088896));
#27722=CARTESIAN_POINT('Ctrl Pts',(-4.78674045548509,-1.13882221279591,
22.2049074818596));
#27723=CARTESIAN_POINT('Ctrl Pts',(-4.74944480663373,-1.27748075963587,
22.2130384548295));
#27724=CARTESIAN_POINT('Ctrl Pts',(-4.71214071757721,-1.4161706856479,22.2211712678822));
#27725=CARTESIAN_POINT('Ctrl Pts',(-4.66876186166881,-1.55320946412703,
22.229304080935));
#27726=CARTESIAN_POINT('Ctrl Pts',(-4.61948328533162,-1.68806316204158,
22.2374368939877));
#27727=CARTESIAN_POINT('Ctrl Pts',(-4.60784474256061,-1.71991271305675,
22.2393576899927));
#27728=CARTESIAN_POINT('Ctrl Pts',(-4.59587732787198,-1.75164045437253,
22.2412784859977));
#27729=CARTESIAN_POINT('Ctrl Pts',(-4.58358374572119,-1.78323949834577,
22.2431992820028));
#27730=CARTESIAN_POINT('Ctrl Pts',(-4.53138139485292,-1.91741880917317,
22.2513555757316));
#27731=CARTESIAN_POINT('Ctrl Pts',(-4.4732732995595,-2.04932941321032,22.2595118694605));
#27732=CARTESIAN_POINT('Ctrl Pts',(-4.40948182443103,-2.17845199683454,
22.2676681631893));
#27733=CARTESIAN_POINT('Ctrl Pts',(-4.34570335099645,-2.30754826326978,
22.2758227945388));
#27734=CARTESIAN_POINT('Ctrl Pts',(-4.27624395672583,-2.43385734304699,
22.2839774258882));
#27735=CARTESIAN_POINT('Ctrl Pts',(-4.20137293026017,-2.55688258693611,
22.2921320572376));
#27736=CARTESIAN_POINT('Ctrl Pts',(-4.12649924762621,-2.67991219534067,
22.3002869778855));
#27737=CARTESIAN_POINT('Ctrl Pts',(-4.04621371938924,-2.79965744692355,
22.3084418985335));
#27738=CARTESIAN_POINT('Ctrl Pts',(-3.96083038422565,-2.91564842357492,
22.3165968191814));
#27739=CARTESIAN_POINT('Ctrl Pts',(-3.87545206900655,-3.03163258076598,
22.3247512603768));
#27740=CARTESIAN_POINT('Ctrl Pts',(-3.78497674564009,-3.14386263566029,
22.3329057015723));
#27741=CARTESIAN_POINT('Ctrl Pts',(-3.6897603353316,-3.25189971098644,22.3410601427678));
#27742=CARTESIAN_POINT('Ctrl Pts',(-3.59452045517901,-3.35996341631582,
22.3492165939472));
#27743=CARTESIAN_POINT('Ctrl Pts',(-3.49453737409855,-3.46383182553087,
22.3573730451267));
#27744=CARTESIAN_POINT('Ctrl Pts',(-3.390206064975,-3.5631006019346,22.3655294963062));
#27745=CARTESIAN_POINT('Ctrl Pts',(-3.3190449401094,-3.63080873147178,22.3710927567092));
#27746=CARTESIAN_POINT('Ctrl Pts',(-3.2458617485111,-3.69637775720605,22.3766560171123));
#27747=CARTESIAN_POINT('Ctrl Pts',(-3.17079131872694,-3.75968954510687,
22.3822192775153));
#27748=CARTESIAN_POINT('Ctrl Pts',(-3.06073059330498,-3.85251093062657,
22.3903755712441));
#27749=CARTESIAN_POINT('Ctrl Pts',(-2.94657060164346,-3.94051351297408,
22.398531864973));
#27750=CARTESIAN_POINT('Ctrl Pts',(-2.82875515750392,-4.02334777534766,
22.4066881587018));
#27751=CARTESIAN_POINT('Ctrl Pts',(-2.71096372598283,-4.10616515481127,
22.4148427900512));
#27752=CARTESIAN_POINT('Ctrl Pts',(-2.58951860188466,-4.18381612337722,
22.4229974214006));
#27753=CARTESIAN_POINT('Ctrl Pts',(-2.46489394941216,-4.25599352450768,
22.43115205275));
#27754=CARTESIAN_POINT('Ctrl Pts',(-2.34026487568228,-4.32817348624603,
22.4393069733979));
#27755=CARTESIAN_POINT('Ctrl Pts',(-2.2124563355605,-4.39487932101967,22.4474618940458));
#27756=CARTESIAN_POINT('Ctrl Pts',(-2.08196898830354,-4.45584876249658,
22.4556168146937));
#27757=CARTESIAN_POINT('Ctrl Pts',(-1.95148931279198,-4.51681461939581,
22.4637712558892));
#27758=CARTESIAN_POINT('Ctrl Pts',(-1.81833144883585,-4.57204461692049,
22.4719256970847));
#27759=CARTESIAN_POINT('Ctrl Pts',(-1.6830179701643,-4.62132379027958,22.4800801382801));
#27760=CARTESIAN_POINT('Ctrl Pts',(-1.5476711381433,-4.67061511043665,22.4882365894596));
#27761=CARTESIAN_POINT('Ctrl Pts',(-1.41016794418998,-4.71395256061313,
22.4963930406391));
#27762=CARTESIAN_POINT('Ctrl Pts',(-1.27104871582113,-4.75117019527921,
22.5045494918186));
#27763=CARTESIAN_POINT('Ctrl Pts',(-1.1761598386047,-4.7765551805722,22.5101127522216));
#27764=CARTESIAN_POINT('Ctrl Pts',(-1.0805195132734,-4.79909414325774,22.5156760126247));
#27765=CARTESIAN_POINT('Ctrl Pts',(-0.984302665699794,-4.81874790010811,
22.5212392730278));
#27766=CARTESIAN_POINT('Ctrl Pts',(-0.843239186082988,-4.84756226473104,
22.5293955667566));
#27767=CARTESIAN_POINT('Ctrl Pts',(-0.700883169296038,-4.87018355294729,
22.5375518604854));
#27768=CARTESIAN_POINT('Ctrl Pts',(-0.557791584474612,-4.88651732942689,
22.5457081542143));
#27769=CARTESIAN_POINT('Ctrl Pts',(-0.414729163941527,-4.90284777682904,
22.5538627855637));
#27770=CARTESIAN_POINT('Ctrl Pts',(-0.270931806748138,-4.91289323106356,
22.5620174169132));
#27771=CARTESIAN_POINT('Ctrl Pts',(-0.126962853132465,-4.91661097672212,
22.5701720482626));
#27772=CARTESIAN_POINT('Ctrl Pts',(0.0170112080101646,-4.92032885427361,
22.5783269689105));
#27773=CARTESIAN_POINT('Ctrl Pts',(0.161156543326358,-4.9177185616535,22.5864818895584));
#27774=CARTESIAN_POINT('Ctrl Pts',(0.304908037492154,-4.90878947920693,
22.5946368102063));
#27775=CARTESIAN_POINT('Ctrl Pts',(0.44865108007284,-4.89986092172813,22.6027912514018));
#27776=CARTESIAN_POINT('Ctrl Pts',(0.591999993866124,-4.88461433935163,
22.6109456925973));
#27777=CARTESIAN_POINT('Ctrl Pts',(0.734393064423372,-4.86311113274484,
22.6191001337927));
#27778=CARTESIAN_POINT('Ctrl Pts',(0.876821233375318,-4.84160262582372,
22.6272565849722));
#27779=CARTESIAN_POINT('Ctrl Pts',(1.01829275721281,-4.81383446278952,22.6354130361517));
#27780=CARTESIAN_POINT('Ctrl Pts',(1.15825379764511,-4.77991958120016,22.6435694873312));
#27781=CARTESIAN_POINT('Ctrl Pts',(1.25371684855673,-4.75678730054672,22.6491327477342));
#27782=CARTESIAN_POINT('Ctrl Pts',(1.34847737014033,-4.7307965287713,22.6546960081373));
#27783=CARTESIAN_POINT('Ctrl Pts',(1.4423630223874,-4.70199659444256,22.6602592685403));
#27784=CARTESIAN_POINT('Ctrl Pts',(1.58000873752081,-4.6597730228787,22.6684155622691));
#27785=CARTESIAN_POINT('Ctrl Pts',(1.71582487225093,-4.61149325752146,22.676571855998));
#27786=CARTESIAN_POINT('Ctrl Pts',(1.84927720660251,-4.55734098742243,22.6847281497268));
#27787=CARTESIAN_POINT('Ctrl Pts',(1.9827023412946,-4.50319975439753,22.6928827810762));
#27788=CARTESIAN_POINT('Ctrl Pts',(2.11376432682064,-4.44318853014346,22.7010374124256));
#27789=CARTESIAN_POINT('Ctrl Pts',(2.24194810603734,-4.37753946325279,22.7091920437751));
#27790=CARTESIAN_POINT('Ctrl Pts',(2.3701364327771,-4.31188806735727,22.717346964423));
#27791=CARTESIAN_POINT('Ctrl Pts',(2.49544604932357,-4.24059857779578,22.7255018850709));
#27792=CARTESIAN_POINT('Ctrl Pts',(2.61738527654948,-4.16394973271797,22.7336568057188));
#27793=CARTESIAN_POINT('Ctrl Pts',(2.7393173345993,-4.08730539405764,22.7418112469143));
#27794=CARTESIAN_POINT('Ctrl Pts',(2.85787911693075,-4.00530250916809,22.7499656881097));
#27795=CARTESIAN_POINT('Ctrl Pts',(2.9726068308012,-3.91826386196413,22.7581201293052));
#27796=CARTESIAN_POINT('Ctrl Pts',(3.08736282384696,-3.8312037606487,22.7662765804847));
#27797=CARTESIAN_POINT('Ctrl Pts',(3.19828259312217,-3.73910561886982,22.7744330316642));
#27798=CARTESIAN_POINT('Ctrl Pts',(3.30493393014768,-3.64233369968467,22.7825894828436));
#27799=CARTESIAN_POINT('Ctrl Pts',(3.37767747352875,-3.57632859841125,22.7881527432467));
#27800=CARTESIAN_POINT('Ctrl Pts',(3.44843593242285,-3.50815003019972,22.7937160036498));
#27801=CARTESIAN_POINT('Ctrl Pts',(3.51708160490553,-3.43792379888432,22.7992792640529));
#27802=CARTESIAN_POINT('Ctrl Pts',(3.61772299635861,-3.33496515079369,22.8074355577817));
#27803=CARTESIAN_POINT('Ctrl Pts',(3.71385912080785,-3.22756494701395,22.8155918515106));
#27804=CARTESIAN_POINT('Ctrl Pts',(3.80510886101175,-3.11614017950891,22.8237481452394));
#27805=CARTESIAN_POINT('Ctrl Pts',(3.89634000310112,-3.00473812210237,22.8319027765889));
#27806=CARTESIAN_POINT('Ctrl Pts',(3.98268653584365,-2.88931339611125,22.8400574079384));
#27807=CARTESIAN_POINT('Ctrl Pts',(4.06380736289325,-2.77031636817793,22.8482120392878));
#27808=CARTESIAN_POINT('Ctrl Pts',(4.14493106783251,-2.65131511863683,22.8563669599358));
#27809=CARTESIAN_POINT('Ctrl Pts',(4.22082850451108,-2.52874158794351,22.8645218805837));
#27810=CARTESIAN_POINT('Ctrl Pts',(4.2912014032943,-2.40307585790899,22.8726768012316));
#27811=CARTESIAN_POINT('Ctrl Pts',(4.36157016464185,-2.27741751614301,22.8808312424271));
#27812=CARTESIAN_POINT('Ctrl Pts',(4.42641487521565,-2.14866763120932,22.8889856836225));
#27813=CARTESIAN_POINT('Ctrl Pts',(4.48548283279364,-2.01733160863889,22.897140124818));
#27814=CARTESIAN_POINT('Ctrl Pts',(4.54456535000215,-1.8859632131197,22.9052965759975));
#27815=CARTESIAN_POINT('Ctrl Pts',(4.59786813138542,-1.7520077114335,22.9134530271769));
#27816=CARTESIAN_POINT('Ctrl Pts',(4.64518606029957,-1.61599180929191,22.9216094783564));
#27817=CARTESIAN_POINT('Ctrl Pts',(4.67746014059345,-1.52321961389581,22.9271727387594));
#27818=CARTESIAN_POINT('Ctrl Pts',(4.70695095634588,-1.42948931754304,22.9327359991624));
#27819=CARTESIAN_POINT('Ctrl Pts',(4.73360660391814,-1.33497250227958,22.9382992595654));
#27820=CARTESIAN_POINT('Ctrl Pts',(4.77268643757363,-1.19640143931329,22.9464555532942));
#27821=CARTESIAN_POINT('Ctrl Pts',(4.80568463565858,-1.05608723077017,22.954611847023));
#27822=CARTESIAN_POINT('Ctrl Pts',(4.83246617905403,-0.914578422443352,
22.9627681407518));
#27823=CARTESIAN_POINT('Ctrl Pts',(4.85924226395468,-0.77309845581107,22.9709227721012));
#27824=CARTESIAN_POINT('Ctrl Pts',(4.87980415966228,-0.630424703735813,
22.9790774034506));
#27825=CARTESIAN_POINT('Ctrl Pts',(4.89406796062614,-0.487115858161732,
22.9872320348));
#27826=CARTESIAN_POINT('Ctrl Pts',(4.90833226762104,-0.34380192847831,22.9953869554479));
#27827=CARTESIAN_POINT('Ctrl Pts',(4.91629799589111,-0.199853192832361,
23.0035418760958));
#27828=CARTESIAN_POINT('Ctrl Pts',(4.91793306526228,-0.0558339332302211,
23.0116967967437));
#27829=CARTESIAN_POINT('Ctrl Pts',(4.91956803850278,0.0881768590439297,
23.0198512379392));
#27830=CARTESIAN_POINT('Ctrl Pts',(4.91487309462416,0.232257832325536,23.0280056791346));
#27831=CARTESIAN_POINT('Ctrl Pts',(4.90386828311162,0.375844282106113,23.0361601203301));
#27832=CARTESIAN_POINT('Ctrl Pts',(4.89286075902875,0.519466124436981,23.0443165715095));
#27833=CARTESIAN_POINT('Ctrl Pts',(4.8755402847948,0.662592865849866,23.052473022689));
#27834=CARTESIAN_POINT('Ctrl Pts',(4.85197888555946,0.804663878016858,23.0606294738685));
#27835=CARTESIAN_POINT('Ctrl Pts',(4.83590839160025,0.901566074699,23.0661927342716));
#27836=CARTESIAN_POINT('Ctrl Pts',(4.81693558990863,0.997977222729638,23.0717559946748));
#27837=CARTESIAN_POINT('Ctrl Pts',(4.79509703999832,1.09372182912263,23.0773192550779));
#27838=CARTESIAN_POINT('Ctrl Pts',(4.76307955119264,1.23409295614259,23.0854755488067));
#27839=CARTESIAN_POINT('Ctrl Pts',(4.72488802171999,1.37308347838278,23.0936318425356));
#27840=CARTESIAN_POINT('Ctrl Pts',(4.68066647623451,1.51014714539823,23.1017881362644));
#27841=CARTESIAN_POINT('Ctrl Pts',(4.6364539437873,1.64718287670805,23.1099427676138));
#27842=CARTESIAN_POINT('Ctrl Pts',(4.58621394982244,1.78229221795751,23.1180973989632));
#27843=CARTESIAN_POINT('Ctrl Pts',(4.53014025315144,1.91494447681311,23.1262520303126));
#27844=CARTESIAN_POINT('Ctrl Pts',(4.47406456717687,2.04760144171856,23.1344069509606));
#27845=CARTESIAN_POINT('Ctrl Pts',(4.41215489119676,2.17780084010838,23.1425618716085));
#27846=CARTESIAN_POINT('Ctrl Pts',(4.3446531622943,2.3050318787093,23.1507167922564));
#27847=CARTESIAN_POINT('Ctrl Pts',(4.27715540202295,2.43225543701207,23.1588712334519));
#27848=CARTESIAN_POINT('Ctrl Pts',(4.20406640426756,2.55651068948397,23.1670256746473));
#27849=CARTESIAN_POINT('Ctrl Pts',(4.12567407799985,2.67731142466095,23.1751801158427));
#27850=CARTESIAN_POINT('Ctrl Pts',(4.04726242884778,2.7981419359493,23.1833365670222));
#27851=CARTESIAN_POINT('Ctrl Pts',(3.96354502113518,2.91551594747252,23.1914930182017));
#27852=CARTESIAN_POINT('Ctrl Pts',(3.87485344714308,3.02897570569052,23.1996494693812));
#27853=CARTESIAN_POINT('Ctrl Pts',(3.81435969675836,3.10636306035582,23.2052127297842));
#27854=CARTESIAN_POINT('Ctrl Pts',(3.75155277972171,3.18193003621664,23.2107759901873));
#27855=CARTESIAN_POINT('Ctrl Pts',(3.68654879791111,3.2555400509163,23.2163392505904));
#27856=CARTESIAN_POINT('Ctrl Pts',(3.59124648761512,3.36345966239857,23.2244955443192));
#27857=CARTESIAN_POINT('Ctrl Pts',(3.49118424254412,3.46721179638804,23.232651838048));
#27858=CARTESIAN_POINT('Ctrl Pts',(3.38674998805847,3.56638578688369,23.2408081317769));
#27859=CARTESIAN_POINT('Ctrl Pts',(3.28233701889694,3.66553956417875,23.2489627631263));
#27860=CARTESIAN_POINT('Ctrl Pts',(3.1735540604992,3.76011682914599,23.2571173944757));
#27861=CARTESIAN_POINT('Ctrl Pts',(3.06082525747466,3.84974438186553,23.2652720258251));
#27862=CARTESIAN_POINT('Ctrl Pts',(2.94809245521654,3.93937511426505,23.273426946473));
#27863=CARTESIAN_POINT('Ctrl Pts',(2.83141378781708,4.02405557183889,23.281581867121));
#27864=CARTESIAN_POINT('Ctrl Pts',(2.71124617520242,4.10345308733392,23.2897367877689));
#27865=CARTESIAN_POINT('Ctrl Pts',(2.59108562760575,4.18284593480847,23.2978912289643));
#27866=CARTESIAN_POINT('Ctrl Pts',(2.46743682491781,4.25695627790285,23.3060456701598));
#27867=CARTESIAN_POINT('Ctrl Pts',(2.34078528370626,4.32549503734361,23.3142001113552));
#27868=CARTESIAN_POINT('Ctrl Pts',(2.21410252422082,4.39405069086828,23.3223565625347));
#27869=CARTESIAN_POINT('Ctrl Pts',(2.084415841582,4.45703185695303,23.3305130137142));
#27870=CARTESIAN_POINT('Ctrl Pts',(1.9522354842652,4.51419535205066,23.3386694648937));
#27871=CARTESIAN_POINT('Ctrl Pts',(1.86207939410505,4.55318478529557,23.3442327252968));
#27872=CARTESIAN_POINT('Ctrl Pts',(1.77076370792075,4.58946869529863,23.3497959856998));
#27873=CARTESIAN_POINT('Ctrl Pts',(1.67845574024884,4.62298273742459,23.3553592461029));
#27874=CARTESIAN_POINT('Ctrl Pts',(1.54312306780585,4.67211766044005,23.3635155398318));
#27875=CARTESIAN_POINT('Ctrl Pts',(1.40560602530865,4.71531512817721,23.3716718335606));
#27876=CARTESIAN_POINT('Ctrl Pts',(1.26644178220433,4.75240026458074,23.3798281272894));
#27877=CARTESIAN_POINT('Ctrl Pts',(1.1273059029359,4.78947784245703,23.3879827586388));
#27878=CARTESIAN_POINT('Ctrl Pts',(0.986523815983789,4.82044548815092,23.3961373899882));
#27879=CARTESIAN_POINT('Ctrl Pts',(0.844646557374703,4.8451785576607,23.4042920213376));
#27880=CARTESIAN_POINT('Ctrl Pts',(0.702764265444423,4.86991250461543,23.4124469419856));
#27881=CARTESIAN_POINT('Ctrl Pts',(0.559787053133157,4.88841137162501,23.4206018626335));
#27882=CARTESIAN_POINT('Ctrl Pts',(0.416275331412915,4.90060179069439,23.4287567832814));
#27883=CARTESIAN_POINT('Ctrl Pts',(0.272772047180556,4.91279149305219,23.4369112244768));
#27884=CARTESIAN_POINT('Ctrl Pts',(0.128734649953469,4.91867346210729,23.4450656656723));
#27885=CARTESIAN_POINT('Ctrl Pts',(-0.0152722056911815,4.91822628822966,
23.4532201068678));
#27886=CARTESIAN_POINT('Ctrl Pts',(-0.159314557511585,4.91777900412838,
23.4613765580473));
#27887=CARTESIAN_POINT('Ctrl Pts',(-0.303326017902509,4.91099946053709,
23.4695330092268));
#27888=CARTESIAN_POINT('Ctrl Pts',(-0.44674218654659,4.89791838246204,23.4776894604063));
#27889=CARTESIAN_POINT('Ctrl Pts',(-0.544561872414483,4.88899618798277,
23.4832527208093));
#27890=CARTESIAN_POINT('Ctrl Pts',(-0.642104633784729,4.8771434932435,23.4888159812124));
#27891=CARTESIAN_POINT('Ctrl Pts',(-0.739192769430403,4.86238389189108,
23.4943792416154));
#27892=CARTESIAN_POINT('Ctrl Pts',(-0.881533644123139,4.84074484657778,
23.5025355353443));
#27893=CARTESIAN_POINT('Ctrl Pts',(-1.02295032191188,4.8128471506273,23.5106918290731));
#27894=CARTESIAN_POINT('Ctrl Pts',(-1.16288746252878,4.77879438896396,23.518848122802));
#27895=CARTESIAN_POINT('Ctrl Pts',(-1.30279608178157,4.74474856778267,23.5270027541514));
#27896=CARTESIAN_POINT('Ctrl Pts',(-1.44122544047467,4.70455026261454,23.5351573855009));
#27897=CARTESIAN_POINT('Ctrl Pts',(-1.57763206797674,4.65835379942222,23.5433120168503));
#27898=CARTESIAN_POINT('Ctrl Pts',(-1.71404353472009,4.61215569733716,23.5514669374982));
#27899=CARTESIAN_POINT('Ctrl Pts',(-1.84843180851907,4.55995911520521,23.5596218581461));
#27900=CARTESIAN_POINT('Ctrl Pts',(-1.98026973172354,4.50196788661576,23.567776778794));
#27901=CARTESIAN_POINT('Ctrl Pts',(-2.11209990377826,4.44398006750581,23.5759312199895));
#27902=CARTESIAN_POINT('Ctrl Pts',(-2.24137971926182,4.380198419138,23.584085661185));
#27903=CARTESIAN_POINT('Ctrl Pts',(-2.36760316542589,4.31087442563169,23.5922401023805));
#27904=CARTESIAN_POINT('Ctrl Pts',(-2.49385772434203,4.24153334449001,23.60039655356));
#27905=CARTESIAN_POINT('Ctrl Pts',(-2.61705411498013,4.16664734934428,23.6085530047395));
#27906=CARTESIAN_POINT('Ctrl Pts',(-2.73671150297794,4.0865135766284,23.616709455919));
#27907=CARTESIAN_POINT('Ctrl Pts',(-2.81832606719533,4.03185683500354,23.622272716322));
#27908=CARTESIAN_POINT('Ctrl Pts',(-2.89829475799206,3.97475967955432,23.627835976725));
#27909=CARTESIAN_POINT('Ctrl Pts',(-2.97647284784729,3.91532788518763,23.633399237128));
#27910=CARTESIAN_POINT('Ctrl Pts',(-3.0910897123887,3.82819495655002,23.6415555308568));
#27911=CARTESIAN_POINT('Ctrl Pts',(-3.20189932385839,3.73600933835503,23.6497118245856));
#27912=CARTESIAN_POINT('Ctrl Pts',(-3.30846367824667,3.63912780102904,23.6578681183145));
#27913=CARTESIAN_POINT('Ctrl Pts',(-3.41500631316333,3.54226600966608,23.6660227496639));
#27914=CARTESIAN_POINT('Ctrl Pts',(-3.51730516965091,3.44071043351294,23.6741773810133));
#27915=CARTESIAN_POINT('Ctrl Pts',(-3.61495695327442,3.3348567118353,23.6823320123627));
#27916=CARTESIAN_POINT('Ctrl Pts',(-3.71261220125015,3.22899923482864,23.6904869330107));
#27917=CARTESIAN_POINT('Ctrl Pts',(-3.80561981680225,3.11884355058895,23.6986418536586));
#27918=CARTESIAN_POINT('Ctrl Pts',(-3.89361452591695,3.00482095740636,23.7067967743065));
#27919=CARTESIAN_POINT('Ctrl Pts',(-3.98160406155576,2.89080506795794,23.7149512155019));
#27920=CARTESIAN_POINT('Ctrl Pts',(-4.06458107667659,2.77292298992585,23.7231056566973));
#27921=CARTESIAN_POINT('Ctrl Pts',(-4.14222167116401,2.65163773721811,23.7312600978927));
#27922=CARTESIAN_POINT('Ctrl Pts',(-4.21988140324229,2.5303225889698,23.7394165490722));
#27923=CARTESIAN_POINT('Ctrl Pts',(-4.29220190557602,2.40560287169386,23.7475730002516));
#27924=CARTESIAN_POINT('Ctrl Pts',(-4.35890323685217,2.27796962979308,23.7557294514311));
#27925=CARTESIAN_POINT('Ctrl Pts',(-4.40439813003045,2.19091498492802,23.7612927118343));
#27926=CARTESIAN_POINT('Ctrl Pts',(-4.44727980599316,2.10250549146035,23.7668559722374));
#27927=CARTESIAN_POINT('Ctrl Pts',(-4.48747182549699,2.01290329570766,23.7724192326405));
#27928=CARTESIAN_POINT('Ctrl Pts',(-4.54616430584186,1.88205704369058,23.7805432720865));
#27929=CARTESIAN_POINT('Ctrl Pts',(-4.59914265290002,1.74861370798986,23.7886673115325));
#27930=CARTESIAN_POINT('Ctrl Pts',(-4.64619388201968,1.61309189855472,23.7967913509785));
#27931=CARTESIAN_POINT('Ctrl Pts',(-4.69086320095292,1.48443071283582,23.8045041209918));
#27932=CARTESIAN_POINT('Ctrl Pts',(-4.73019058037801,1.35389656612923,23.812216891005));
#27933=CARTESIAN_POINT('Ctrl Pts',(-4.76403458704968,1.22194824599669,23.8199296610182));
#27934=CARTESIAN_POINT('Origin',(0.,0.,-3.23514056400928));
#27935=CARTESIAN_POINT('',(-4.76403457790609,1.221948281645,25.9153493127618));
#27936=CARTESIAN_POINT('',(-4.76438990516231,1.22203958206317,25.569924562744));
#27937=CARTESIAN_POINT('',(-4.76403458704967,1.22194824599672,-3.23514056400928));
#27938=CARTESIAN_POINT('Ctrl Pts',(-4.76403457790609,1.221948281645,25.9153493127618));
#27939=CARTESIAN_POINT('Ctrl Pts',(-4.74875002836548,1.28153846529919,25.9118945228887));
#27940=CARTESIAN_POINT('Ctrl Pts',(-4.73234658248963,1.34084513057762,25.9084346143025));
#27941=CARTESIAN_POINT('Ctrl Pts',(-4.69614720705212,1.46276932404858,25.9012681232217));
#27942=CARTESIAN_POINT('Ctrl Pts',(-4.67620448887776,1.52532099721689,25.8975618007853));
#27943=CARTESIAN_POINT('Ctrl Pts',(-4.63222091208789,1.6542974654206,25.8898497389304));
#27944=CARTESIAN_POINT('Ctrl Pts',(-4.60798912151711,1.72064138763471,25.8858434768254));
#27945=CARTESIAN_POINT('Ctrl Pts',(-4.51839064989085,1.95046742754488,25.8718161362204));
#27946=CARTESIAN_POINT('Ctrl Pts',(-4.44568366032193,2.11094114988293,25.8617495733547));
#27947=CARTESIAN_POINT('Ctrl Pts',(-4.32332118104867,2.34650144285512,25.8465541938121));
#27948=CARTESIAN_POINT('Ctrl Pts',(-4.27995581230672,2.42469656592521,25.8414376007671));
#27949=CARTESIAN_POINT('Ctrl Pts',(-4.20461684436959,2.5522201961594,25.8329825919278));
#27950=CARTESIAN_POINT('Ctrl Pts',(-4.17384733280937,2.60223544202071,25.8296373223592));
#27951=CARTESIAN_POINT('Ctrl Pts',(-4.13451793790827,2.66367170302817,25.8254950832103));
#27952=CARTESIAN_POINT('Ctrl Pts',(-4.12679446771772,2.6756219732771,25.8246877781314));
#27953=CARTESIAN_POINT('Ctrl Pts',(-4.09767138862207,2.72025706171964,25.8216666892418));
#27954=CARTESIAN_POINT('Ctrl Pts',(-4.07593448720148,2.75271999618634,25.8194581497318));
#27955=CARTESIAN_POINT('Ctrl Pts',(-3.94719896339505,2.94011122106081,25.8066314063624));
#27956=CARTESIAN_POINT('Ctrl Pts',(-3.83176004896034,3.08905331441592,25.7961158073582));
#27957=CARTESIAN_POINT('Ctrl Pts',(-3.62416225441081,3.32730263217222,25.7784033607096));
#27958=CARTESIAN_POINT('Ctrl Pts',(-3.53654097633806,3.42028831921108,25.7712353389081));
#27959=CARTESIAN_POINT('Ctrl Pts',(-3.40607262686828,3.5483643478114,25.7609259341696));
#27960=CARTESIAN_POINT('Ctrl Pts',(-3.36609847511608,3.58630746988575,25.7578129616853));
#27961=CARTESIAN_POINT('Ctrl Pts',(-3.27323291417364,3.67153390265311,25.7506789193559));
#27962=CARTESIAN_POINT('Ctrl Pts',(-3.21993934609282,3.71836057433297,25.7466545508027));
#27963=CARTESIAN_POINT('Ctrl Pts',(-3.00536396947071,3.89882491348648,25.7307091999655));
#27964=CARTESIAN_POINT('Ctrl Pts',(-2.8366301860255,4.02325431635058,25.7187187283622));
#27965=CARTESIAN_POINT('Ctrl Pts',(-2.60205705991811,4.17412358660298,25.702760080165));
#27966=CARTESIAN_POINT('Ctrl Pts',(-2.54284161599757,4.21045903433922,25.6987888323481));
#27967=CARTESIAN_POINT('Ctrl Pts',(-2.43965848985968,4.270802744875,25.69197263239));
#27968=CARTESIAN_POINT('Ctrl Pts',(-2.39605708792969,4.29541617815705,25.6891233058648));
#27969=CARTESIAN_POINT('Ctrl Pts',(-2.33404859179352,4.32918261477363,25.6851169827759));
#27970=CARTESIAN_POINT('Ctrl Pts',(-2.31594860845906,4.33889236932821,25.6839530349122));
#27971=CARTESIAN_POINT('Ctrl Pts',(-2.28571799161006,4.35486655296985,25.6820180852886));
#27972=CARTESIAN_POINT('Ctrl Pts',(-2.27362125872273,4.3611943094973,25.6812461896));
#27973=CARTESIAN_POINT('Ctrl Pts',(-2.24860046154847,4.37415020140538,25.6796543017208));
#27974=CARTESIAN_POINT('Ctrl Pts',(-2.23567306398049,4.38077161847659,25.6788343969311));
#27975=CARTESIAN_POINT('Ctrl Pts',(-2.07692426712593,4.46119709626134,25.6687960404098));
#27976=CARTESIAN_POINT('Ctrl Pts',(-1.92753921805164,4.5277464388947,25.6596567720064));
#27977=CARTESIAN_POINT('Ctrl Pts',(-1.68000008054214,4.62354681230963,25.6447851253013));
#27978=CARTESIAN_POINT('Ctrl Pts',(-1.58376152517707,4.65739032174958,25.6390681400481));
#27979=CARTESIAN_POINT('Ctrl Pts',(-1.45989532629235,4.69666584648349,25.6317619024208));
#27980=CARTESIAN_POINT('Ctrl Pts',(-1.43317817093539,4.70488732700011,25.6301890667584));
#27981=CARTESIAN_POINT('Ctrl Pts',(-1.38406322686001,4.71954394419686,25.627302592721));
#27982=CARTESIAN_POINT('Ctrl Pts',(-1.36168698270088,4.72604851998848,25.6259894053175));
#27983=CARTESIAN_POINT('Ctrl Pts',(-1.28287441192812,4.74835244356736,25.6213699769613));
#27984=CARTESIAN_POINT('Ctrl Pts',(-1.2262030469283,4.76330176309321,25.6180586997349));
#27985=CARTESIAN_POINT('Ctrl Pts',(-1.09866510402713,4.79451801642506,25.6106240775847));
#27986=CARTESIAN_POINT('Ctrl Pts',(-1.02767782807547,4.81023348041227,25.6064977905989));
#27987=CARTESIAN_POINT('Ctrl Pts',(-0.806010885904746,4.85417608620273,
25.5936396372583));
#27988=CARTESIAN_POINT('Ctrl Pts',(-0.654343236654578,4.87693684089327,
25.5848773823583));
#27989=CARTESIAN_POINT('Ctrl Pts',(-0.404505680617832,4.90256426088584,
25.570500839929));
#27990=CARTESIAN_POINT('Ctrl Pts',(-0.306871944675769,4.90964264745801,
25.5648976325931));
#27991=CARTESIAN_POINT('Ctrl Pts',(-0.162462333983677,4.91578755680258,
25.5566441092165));
#27992=CARTESIAN_POINT('Ctrl Pts',(-0.115806625120437,4.91710790925397,
25.5539829125758));
#27993=CARTESIAN_POINT('Ctrl Pts',(-0.0502419764562126,4.91802968394553,
25.5502526000273));
#27994=CARTESIAN_POINT('Ctrl Pts',(-0.0313435736795576,4.91818643541423,
25.549178475921));
#27995=CARTESIAN_POINT('Ctrl Pts',(0.0198230901555402,4.91831590313559,
25.546273601232));
#27996=CARTESIAN_POINT('Ctrl Pts',(0.0520909331190609,4.91807999545365,
25.5444453970307));
#27997=CARTESIAN_POINT('Ctrl Pts',(0.138886448811547,4.91659111830121,25.5395371916102));
#27998=CARTESIAN_POINT('Ctrl Pts',(0.19339953504859,4.91474866004097,25.5364637871435));
#27999=CARTESIAN_POINT('Ctrl Pts',(0.41317027152132,4.9036585095395,25.5240881587301));
#28000=CARTESIAN_POINT('Ctrl Pts',(0.577943962168558,4.8869784044902,25.5148401042331));
#28001=CARTESIAN_POINT('Ctrl Pts',(0.826917085376503,4.84900463280085,25.5007188877127));
#28002=CARTESIAN_POINT('Ctrl Pts',(0.911912635931431,4.83374109364452,25.4958723068545));
#28003=CARTESIAN_POINT('Ctrl Pts',(1.00509993357753,4.81446102884588,25.490515783982));
#28004=CARTESIAN_POINT('Ctrl Pts',(1.01373328274043,4.81265059047086,25.4900191236602));
#28005=CARTESIAN_POINT('Ctrl Pts',(1.02946000951978,4.80930845472745,25.4891136357867));
#28006=CARTESIAN_POINT('Ctrl Pts',(1.03655495940822,4.80778426511544,25.4887048523722));
#28007=CARTESIAN_POINT('Ctrl Pts',(1.04991020668931,4.80488425503551,25.4879348320322));
#28008=CARTESIAN_POINT('Ctrl Pts',(1.05617123963045,4.80351188807435,25.4875736161116));
#28009=CARTESIAN_POINT('Ctrl Pts',(1.06841303567721,4.80080349545828,25.4868669053009));
#28010=CARTESIAN_POINT('Ctrl Pts',(1.07439402034343,4.79946852326035,25.4865214173269));
#28011=CARTESIAN_POINT('Ctrl Pts',(1.14802273977636,4.78288986253755,25.4822656718128));
#28012=CARTESIAN_POINT('Ctrl Pts',(1.2153427367887,4.76622843943874,25.4783471119655));
#28013=CARTESIAN_POINT('Ctrl Pts',(1.35547661561205,4.7283838193993,25.4701235798356));
#28014=CARTESIAN_POINT('Ctrl Pts',(1.42819841314884,4.70692888257124,25.4658177274077));
#28015=CARTESIAN_POINT('Ctrl Pts',(1.64552473023388,4.63731124179539,25.4528240196952));
#28016=CARTESIAN_POINT('Ctrl Pts',(1.78841427296511,4.58410085870939,25.4441082412064));
#28017=CARTESIAN_POINT('Ctrl Pts',(2.04694568047216,4.47389616161636,25.4280200953883));
#28018=CARTESIAN_POINT('Ctrl Pts',(2.16326663764913,4.41882467209778,25.4206568116731));
#28019=CARTESIAN_POINT('Ctrl Pts',(2.31431760536911,4.33991495424295,25.4109563830767));
#28020=CARTESIAN_POINT('Ctrl Pts',(2.35109248018979,4.32010323863895,25.4085836010601));
#28021=CARTESIAN_POINT('Ctrl Pts',(2.41912546407324,4.28232582355539,25.4041753017039));
#28022=CARTESIAN_POINT('Ctrl Pts',(2.45044702193469,4.2644802611968,25.402138244685));
#28023=CARTESIAN_POINT('Ctrl Pts',(2.62325523881742,4.1634896416304,25.3908480097775));
#28024=CARTESIAN_POINT('Ctrl Pts',(2.76070938764347,4.07364689674998,25.3816715192091));
#28025=CARTESIAN_POINT('Ctrl Pts',(2.97558899947648,3.91731789626265,25.3667830000934));
#28026=CARTESIAN_POINT('Ctrl Pts',(3.05588895172479,3.85500348781476,25.3610867758089));
#28027=CARTESIAN_POINT('Ctrl Pts',(3.19829199426285,3.73724870863627,25.3506969138183));
#28028=CARTESIAN_POINT('Ctrl Pts',(3.26102843752471,3.68263396164004,25.3460108530485));
#28029=CARTESIAN_POINT('Ctrl Pts',(3.37219251976504,3.58079183424249,25.3374898433669));
#28030=CARTESIAN_POINT('Ctrl Pts',(3.42108856480557,3.53410603214349,25.3336607342812));
#28031=CARTESIAN_POINT('Ctrl Pts',(3.54152979551226,3.41426662960101,25.3240130712444));
#28032=CARTESIAN_POINT('Ctrl Pts',(3.61178316939242,3.33986105120147,25.318184567119));
#28033=CARTESIAN_POINT('Ctrl Pts',(3.78362255592755,3.14609784889867,25.3033915434807));
#28034=CARTESIAN_POINT('Ctrl Pts',(3.88191994586096,3.02397562365284,25.2944130243293));
#28035=CARTESIAN_POINT('Ctrl Pts',(3.99707234477015,2.86602521527625,25.2832378579024));
#28036=CARTESIAN_POINT('Ctrl Pts',(4.01955324499409,2.83440992027006,25.2810219756092));
#28037=CARTESIAN_POINT('Ctrl Pts',(4.05645923102551,2.78118613031717,25.277327375925));
#28038=CARTESIAN_POINT('Ctrl Pts',(4.07109133322094,2.75972338296839,25.2758470486522));
#28039=CARTESIAN_POINT('Ctrl Pts',(4.10878334400893,2.70348360671294,25.2719934373972));
#28040=CARTESIAN_POINT('Ctrl Pts',(4.13157205269595,2.66852704834047,25.2696231356119));
#28041=CARTESIAN_POINT('Ctrl Pts',(4.17641621133642,2.59778697057288,25.2648784603831));
#28042=CARTESIAN_POINT('Ctrl Pts',(4.19846332812367,2.56200219596304,25.2625043567665));
#28043=CARTESIAN_POINT('Ctrl Pts',(4.30718214443455,2.38036726258589,25.2505708850209));
#28044=CARTESIAN_POINT('Ctrl Pts',(4.38672537253607,2.23038295384594,25.2410884138778));
#28045=CARTESIAN_POINT('Ctrl Pts',(4.50411876974339,1.97834348095936,25.2255075415065));
#28046=CARTESIAN_POINT('Ctrl Pts',(4.54661798150407,1.87861476664434,25.2194292235948));
#28047=CARTESIAN_POINT('Ctrl Pts',(4.61345190189181,1.70619559886004,25.2090210330939));
#28048=CARTESIAN_POINT('Ctrl Pts',(4.63944611601942,1.63419136756133,25.2047036356566));
#28049=CARTESIAN_POINT('Ctrl Pts',(4.6854196546457,1.49689140814331,25.1965134484897));
#28050=CARTESIAN_POINT('Ctrl Pts',(4.70574050472253,1.43172881185113,25.1926440787384));
#28051=CARTESIAN_POINT('Ctrl Pts',(4.78788540151665,1.1476416878596,25.1758381160438));
#28052=CARTESIAN_POINT('Ctrl Pts',(4.83583492567065,0.925000392210101,25.1628136794565));
#28053=CARTESIAN_POINT('Ctrl Pts',(4.87486173681126,0.653525841951685,25.147123065902));
#28054=CARTESIAN_POINT('Ctrl Pts',(4.880859272914,0.607112647828514,25.1444477424287));
#28055=CARTESIAN_POINT('Ctrl Pts',(4.89306669070323,0.50071665554164,25.138334007194));
#28056=CARTESIAN_POINT('Ctrl Pts',(4.89883768700977,0.440690651205942,25.1348985826877));
#28057=CARTESIAN_POINT('Ctrl Pts',(4.90634708071251,0.343935721916961,25.1293882428031));
#28058=CARTESIAN_POINT('Ctrl Pts',(4.90877991194379,0.307267429807165,25.1273065374152));
#28059=CARTESIAN_POINT('Ctrl Pts',(4.91412323350844,0.210288738032719,25.1218171109064));
#28060=CARTESIAN_POINT('Ctrl Pts',(4.91633449034602,0.149946046654312,25.1184170245335));
#28061=CARTESIAN_POINT('Ctrl Pts',(4.92064124695686,-0.0864771760380505,
25.10512705447));
#28062=CARTESIAN_POINT('Ctrl Pts',(4.91439132807231,-0.262577658666979,
25.0952922350161));
#28063=CARTESIAN_POINT('Ctrl Pts',(4.89166681725229,-0.516755903942656,
25.0809744088554));
#28064=CARTESIAN_POINT('Ctrl Pts',(4.88272257619821,-0.59536627711533,25.0765299464555));
#28065=CARTESIAN_POINT('Ctrl Pts',(4.86193164199094,-0.745710841696043,
25.0679802827223));
#28066=CARTESIAN_POINT('Ctrl Pts',(4.85038287242818,-0.817465461366168,
25.0638779847333));
#28067=CARTESIAN_POINT('Ctrl Pts',(4.82437083697558,-0.959012775985137,
25.0557317699744));
#28068=CARTESIAN_POINT('Ctrl Pts',(4.8099720023394,-1.02879961921618,25.0516892487404));
#28069=CARTESIAN_POINT('Ctrl Pts',(4.76535025269178,-1.22358200180145,25.040323634478));
#28070=CARTESIAN_POINT('Ctrl Pts',(4.73173455993439,-1.34774008211567,25.0329815499531));
#28071=CARTESIAN_POINT('Ctrl Pts',(4.65783751870718,-1.58360230434377,25.0188391334739));
#28072=CARTESIAN_POINT('Ctrl Pts',(4.61830060162211,-1.69544868890356,25.01204582796));
#28073=CARTESIAN_POINT('Ctrl Pts',(4.55611676870843,-1.85298713888958,25.0023690940653));
#28074=CARTESIAN_POINT('Ctrl Pts',(4.53674342472499,-1.89992644765093,24.9994719547882));
#28075=CARTESIAN_POINT('Ctrl Pts',(4.50003622043109,-1.98509909825754,24.9941925527533));
#28076=CARTESIAN_POINT('Ctrl Pts',(4.48293305672543,-2.02342671672803,24.9918083775204));
#28077=CARTESIAN_POINT('Ctrl Pts',(4.44782631327875,-2.09946903245329,24.9870635426189));
#28078=CARTESIAN_POINT('Ctrl Pts',(4.42982840700796,-2.13718260080019,24.9847030340324));
#28079=CARTESIAN_POINT('Ctrl Pts',(4.35215321764349,-2.29474847518332,24.9747992348253));
#28080=CARTESIAN_POINT('Ctrl Pts',(4.28807503532063,-2.41236843434848,24.9673024429398));
#28081=CARTESIAN_POINT('Ctrl Pts',(4.13508732614429,-2.66778563486339,24.9506230882706));
#28082=CARTESIAN_POINT('Ctrl Pts',(4.04392723399034,-2.80404690543407,24.9414476033246));
#28083=CARTESIAN_POINT('Ctrl Pts',(3.90352009856139,-2.99279340583187,24.9281916835003));
#28084=CARTESIAN_POINT('Ctrl Pts',(3.85966000459452,-3.04914840973011,24.9241595131294));
#28085=CARTESIAN_POINT('Ctrl Pts',(3.77447902277333,-3.15381179773572,24.9165189752553));
#28086=CARTESIAN_POINT('Ctrl Pts',(3.73341810534733,-3.20231320888572,24.9129135587893));
#28087=CARTESIAN_POINT('Ctrl Pts',(3.61824704873583,-3.33312710056247,24.9030028101423));
#28088=CARTESIAN_POINT('Ctrl Pts',(3.54227886064693,-3.41375277186777,24.8966837466174));
#28089=CARTESIAN_POINT('Ctrl Pts',(3.36856034709123,-3.58607378919437,24.8826912808268));
#28090=CARTESIAN_POINT('Ctrl Pts',(3.26965227216473,-3.67647902912972,24.8750166782366));
#28091=CARTESIAN_POINT('Ctrl Pts',(3.12634584575987,-3.79710326393923,24.8643112451312));
#28092=CARTESIAN_POINT('Ctrl Pts',(3.08495695275294,-3.83080568696026,24.8612650020019));
#28093=CARTESIAN_POINT('Ctrl Pts',(3.00895851107873,-3.89065963251992,24.855756576577));
#28094=CARTESIAN_POINT('Ctrl Pts',(2.9745358471372,-3.91703973043366,24.8532922029504));
#28095=CARTESIAN_POINT('Ctrl Pts',(2.91158814086704,-3.96397188945642,24.8488428471127));
#28096=CARTESIAN_POINT('Ctrl Pts',(2.88318314603763,-3.98467986355621,24.8468557601274));
#28097=CARTESIAN_POINT('Ctrl Pts',(2.79159276974941,-4.04995945218888,24.8405092529416));
#28098=CARTESIAN_POINT('Ctrl Pts',(2.72757692295855,-4.09334656566228,24.8361644375581));
#28099=CARTESIAN_POINT('Ctrl Pts',(2.50654684152594,-4.23566274040518,24.8214155989341));
#28100=CARTESIAN_POINT('Ctrl Pts',(2.34496968592233,-4.32720844884156,24.8110501117144));
#28101=CARTESIAN_POINT('Ctrl Pts',(2.14239529354691,-4.42729679290538,24.7983495532319));
#28102=CARTESIAN_POINT('Ctrl Pts',(2.10596437784323,-4.44474166874671,24.7960769229157));
#28103=CARTESIAN_POINT('Ctrl Pts',(2.00389342532524,-4.4920814859191,24.7897379815021));
#28104=CARTESIAN_POINT('Ctrl Pts',(1.93780492820308,-4.52098405640698,24.7856659250069));
#28105=CARTESIAN_POINT('Ctrl Pts',(1.81281120585003,-4.57240329238063,24.778014696421));
#28106=CARTESIAN_POINT('Ctrl Pts',(1.7540619178666,-4.59526093004211,24.7744388182871));
#28107=CARTESIAN_POINT('Ctrl Pts',(1.57346208256761,-4.66155895508438,24.7635011798637));
#28108=CARTESIAN_POINT('Ctrl Pts',(1.45032427299878,-4.70132679263998,24.7561175121078));
#28109=CARTESIAN_POINT('Ctrl Pts',(1.19267523494882,-4.77344836438742,24.740810752005));
#28110=CARTESIAN_POINT('Ctrl Pts',(1.05807532269833,-4.80507651287101,24.7328918541439));
#28111=CARTESIAN_POINT('Ctrl Pts',(0.862870866002943,-4.84234449709967,
24.7215465624031));
#28112=CARTESIAN_POINT('Ctrl Pts',(0.803214493592105,-4.85259651766762,
24.7180980576105));
#28113=CARTESIAN_POINT('Ctrl Pts',(0.707057953862087,-4.86729930449453,
24.7125746632872));
#28114=CARTESIAN_POINT('Ctrl Pts',(0.67067110686897,-4.87244638518387,24.7104929033638));
#28115=CARTESIAN_POINT('Ctrl Pts',(0.574580805407105,-4.88494197448149,
24.7050161767685));
#28116=CARTESIAN_POINT('Ctrl Pts',(0.514794283022248,-4.89160384448855,
24.7016287572397));
#28117=CARTESIAN_POINT('Ctrl Pts',(0.279298420002498,-4.91347916340054,
24.6883357899522));
#28118=CARTESIAN_POINT('Ctrl Pts',(0.102945798036454,-4.92033411843586,
24.6784857719044));
#28119=CARTESIAN_POINT('Ctrl Pts',(-0.152526876040929,-4.91652133513303,
24.6641506601392));
#28120=CARTESIAN_POINT('Ctrl Pts',(-0.231619298670093,-4.91343045456756,
24.6597042414346));
#28121=CARTESIAN_POINT('Ctrl Pts',(-0.383143685070682,-4.90384209845029,
24.6511516770548));
#28122=CARTESIAN_POINT('Ctrl Pts',(-0.455573966956382,-4.89764418974435,
24.647048441161));
#28123=CARTESIAN_POINT('Ctrl Pts',(-0.590176620624893,-4.88311435383984,
24.6393852481865));
#28124=CARTESIAN_POINT('Ctrl Pts',(-0.652378735392301,-4.87519395655599,
24.6358288387104));
#28125=CARTESIAN_POINT('Ctrl Pts',(-0.835703772958265,-4.84827918670137,
24.6252959527907));
#28126=CARTESIAN_POINT('Ctrl Pts',(-0.956286057888601,-4.82594324689242,
24.6183004296419));
#28127=CARTESIAN_POINT('Ctrl Pts',(-1.25257064314254,-4.75951980371715,
24.600933314225));
#28128=CARTESIAN_POINT('Ctrl Pts',(-1.42691394045778,-4.71018887179745,
24.5905524813566));
#28129=CARTESIAN_POINT('Ctrl Pts',(-1.63894829265869,-4.63733689092631,
24.5777867371998));
#28130=CARTESIAN_POINT('Ctrl Pts',(-1.67957034075495,-4.62277930188418,
24.5753347977912));
#28131=CARTESIAN_POINT('Ctrl Pts',(-1.75817123991425,-4.59343851471963,
24.5705807183892));
#28132=CARTESIAN_POINT('Ctrl Pts',(-1.79616829907697,-4.57871411871256,
24.5682781801633));
#28133=CARTESIAN_POINT('Ctrl Pts',(-1.93065715844491,-4.52466599697305,
24.5601044868722));
#28134=CARTESIAN_POINT('Ctrl Pts',(-2.02607804151243,-4.48275001099167,
24.5542604083466));
#28135=CARTESIAN_POINT('Ctrl Pts',(-2.13247163187994,-4.43192237124954,
24.5476523023696));
#28136=CARTESIAN_POINT('Ctrl Pts',(-2.14482222924629,-4.4259585143526,24.5468837865482));
#28137=CARTESIAN_POINT('Ctrl Pts',(-2.27586534939798,-4.36200308243287,
24.5387137211771));
#28138=CARTESIAN_POINT('Ctrl Pts',(-2.39219985749253,-4.29930384559869,
24.5313199721257));
#28139=CARTESIAN_POINT('Ctrl Pts',(-2.58229888333374,-4.18674160583593,
24.5189063024916));
#28140=CARTESIAN_POINT('Ctrl Pts',(-2.65748854877547,-4.13942352823295,
24.513904938638));
#28141=CARTESIAN_POINT('Ctrl Pts',(-2.78172617930073,-4.05645797336813,
24.5054655694754));
#28142=CARTESIAN_POINT('Ctrl Pts',(-2.83147138682824,-4.02189277756184,
24.5020371117377));
#28143=CARTESIAN_POINT('Ctrl Pts',(-2.94991368737741,-3.93630697754053,
24.493747661292));
#28144=CARTESIAN_POINT('Ctrl Pts',(-3.0179421690765,-3.88439547335493,24.4888804744478));
#28145=CARTESIAN_POINT('Ctrl Pts',(-3.28024928063424,-3.67318083455939,
24.4696735313068));
#28146=CARTESIAN_POINT('Ctrl Pts',(-3.46355705662923,-3.50086625062439,
24.4552473399512));
#28147=CARTESIAN_POINT('Ctrl Pts',(-3.66142136286597,-3.2840474043411,24.4385371770045));
#28148=CARTESIAN_POINT('Ctrl Pts',(-3.68954180614442,-3.25242295314027,
24.4361330310958));
#28149=CARTESIAN_POINT('Ctrl Pts',(-3.7443956145862,-3.18910694410987,24.4313868639297));
#28150=CARTESIAN_POINT('Ctrl Pts',(-3.77114337306935,-3.1574323949716,24.4290448278979));
#28151=CARTESIAN_POINT('Ctrl Pts',(-3.88669517477196,-3.0170333176635,24.4187926492465));
#28152=CARTESIAN_POINT('Ctrl Pts',(-3.9712222104939,-2.9048725363278,24.4109345388819));
#28153=CARTESIAN_POINT('Ctrl Pts',(-4.1419976834632,-2.65685469470588,24.3940649349396));
#28154=CARTESIAN_POINT('Ctrl Pts',(-4.22661283480377,-2.520072370854,24.3850605900295));
#28155=CARTESIAN_POINT('Ctrl Pts',(-4.3386601588022,-2.31737623043034,24.3720076862598));
#28156=CARTESIAN_POINT('Ctrl Pts',(-4.37159806093122,-2.25462520372215,
24.3680054278167));
#28157=CARTESIAN_POINT('Ctrl Pts',(-4.43576227975074,-2.12568772551956,
24.3598499253914));
#28158=CARTESIAN_POINT('Ctrl Pts',(-4.46689045451696,-2.05947197289073,
24.3556970001224));
#28159=CARTESIAN_POINT('Ctrl Pts',(-4.54747699290876,-1.87761805458317,
24.3443778734031));
#28160=CARTESIAN_POINT('Ctrl Pts',(-4.59399563410975,-1.76073850206107,
24.3371949085604));
#28161=CARTESIAN_POINT('Ctrl Pts',(-4.67437318127326,-1.53383094874207,
24.3234197317762));
#28162=CARTESIAN_POINT('Ctrl Pts',(-4.70895100423211,-1.42414274752008,
24.3168340540159));
#28163=CARTESIAN_POINT('Ctrl Pts',(-4.75789307223235,-1.24751842851091,
24.3063633027376));
#28164=CARTESIAN_POINT('Ctrl Pts',(-4.77475993704927,-1.18131978131719,
24.302468428636));
#28165=CARTESIAN_POINT('Ctrl Pts',(-4.79787435774482,-1.08199739384228,
24.2966750468482));
#28166=CARTESIAN_POINT('Ctrl Pts',(-4.80516917266076,-1.04912629159437,
24.2947660246127));
#28167=CARTESIAN_POINT('Ctrl Pts',(-4.82259739546037,-0.966595049042747,
24.2899941162226));
#28168=CARTESIAN_POINT('Ctrl Pts',(-4.8323018245132,-0.916848291746842,
24.2871361969917));
#28169=CARTESIAN_POINT('Ctrl Pts',(-4.86971990716506,-0.707900073762178,
24.2751901952639));
#28170=CARTESIAN_POINT('Ctrl Pts',(-4.89034807242049,-0.547531767085985,
24.2661587863224));
#28171=CARTESIAN_POINT('Ctrl Pts',(-4.91317675200177,-0.257886624354426,
24.2498734132655));
#28172=CARTESIAN_POINT('Ctrl Pts',(-4.91824897357135,-0.128987335353184,
24.2426359827897));
#28173=CARTESIAN_POINT('Ctrl Pts',(-4.91825054418017,0.0683528868924758,
24.2315070543874));
#28174=CARTESIAN_POINT('Ctrl Pts',(-4.91682452396337,0.13673695520985,24.2276419294321));
#28175=CARTESIAN_POINT('Ctrl Pts',(-4.91079728389466,0.281165252383581,
24.2194519491413));
#28176=CARTESIAN_POINT('Ctrl Pts',(-4.90585446576094,0.357177315883419,
24.215125832008));
#28177=CARTESIAN_POINT('Ctrl Pts',(-4.88981864771805,0.538595342356156,
24.2047551069089));
#28178=CARTESIAN_POINT('Ctrl Pts',(-4.87708007680103,0.643817457016504,
24.1987027752241));
#28179=CARTESIAN_POINT('Ctrl Pts',(-4.83789295986772,0.898293467968513,
24.1839719279346));
#28180=CARTESIAN_POINT('Ctrl Pts',(-4.80792540240429,1.04689689662642,24.1752892081604));
#28181=CARTESIAN_POINT('Ctrl Pts',(-4.76880303843594,1.20324303490926,24.1660979591495));
#28182=CARTESIAN_POINT('Ctrl Pts',(-4.76643256600081,1.21259919647824,24.1655477262546));
#28183=CARTESIAN_POINT('Ctrl Pts',(-4.76403458701365,1.22194824613716,24.1649977190913));
#28184=CARTESIAN_POINT('',(-4.91834666357043,-0.000109981193844847,23.8898594354524));
#28185=CARTESIAN_POINT('Ctrl Pts',(-4.76403458704968,1.22194824599669,23.8199296610182));
#28186=CARTESIAN_POINT('Ctrl Pts',(-4.79967280710214,1.08300478950659,23.8280513174643));
#28187=CARTESIAN_POINT('Ctrl Pts',(-4.8292303566121,0.942493438545646,23.8361729739104));
#28188=CARTESIAN_POINT('Ctrl Pts',(-4.85259123348966,0.800962785127571,
23.8442946303564));
#28189=CARTESIAN_POINT('Ctrl Pts',(-4.87595661619512,0.659404833386302,
23.8524178533013));
#28190=CARTESIAN_POINT('Ctrl Pts',(-4.89312288018924,0.516827521625683,
23.8605410762462));
#28191=CARTESIAN_POINT('Ctrl Pts',(-4.90402544113868,0.373788088580368,
23.8686642991911));
#28192=CARTESIAN_POINT('Ctrl Pts',(-4.9135077718429,0.249381794117097,23.8757293444318));
#28193=CARTESIAN_POINT('Ctrl Pts',(-4.91825278780639,0.124626196682925,
23.8827943896725));
#28194=CARTESIAN_POINT('Ctrl Pts',(-4.91824999877057,-0.000109969512879116,
23.8898594349132));
#28195=CARTESIAN_POINT('Ctrl Pts',(-4.91844317597977,-0.000109992856395721,
23.8898594359907));
#28196=CARTESIAN_POINT('Ctrl Pts',(-4.91856639306803,-0.127114903953705,
23.8970527000448));
#28197=CARTESIAN_POINT('Ctrl Pts',(-4.88269542365051,-1.07223352680412,
23.9505859626031));
#28198=CARTESIAN_POINT('Ctrl Pts',(-4.2981825700306,-2.79529185668768,24.0504592236655));
#28199=CARTESIAN_POINT('Ctrl Pts',(-2.43577373223791,-4.51165560462223,
24.189479219178));
#28200=CARTESIAN_POINT('Ctrl Pts',(0.0209816754386009,-5.12714245351884,
24.3284992146905));
#28201=CARTESIAN_POINT('Ctrl Pts',(2.47261740115848,-4.49156911968052,24.4675192102031));
#28202=CARTESIAN_POINT('Ctrl Pts',(4.32091643284836,-2.76002013574545,24.6065392057156));
#28203=CARTESIAN_POINT('Ctrl Pts',(5.11488031565789,-0.355006092729031,
24.7455592012281));
#28204=CARTESIAN_POINT('Ctrl Pts',(4.66077606687451,2.13663202817638,24.8845791967406));
#28205=CARTESIAN_POINT('Ctrl Pts',(3.06940843780244,4.1069163384864,25.0235991922531));
#28206=CARTESIAN_POINT('Ctrl Pts',(0.729082745657666,5.07508308497148,25.1626191877656));
#28207=CARTESIAN_POINT('Ctrl Pts',(-1.78914445815378,4.80489251463932,25.3016391832782));
#28208=CARTESIAN_POINT('Ctrl Pts',(-3.82211936364006,3.39601450889612,25.4374076416044));
#28209=CARTESIAN_POINT('Ctrl Pts',(-4.57494348751987,1.95876786470781,25.5268361014264));
#28210=CARTESIAN_POINT('Ctrl Pts',(-4.76438990516341,1.22203958205891,25.5699245627443));
#28211=CARTESIAN_POINT('Origin',(0.,0.,-3.23514056400928));
#28212=CARTESIAN_POINT('',(-4.76403458666814,1.22194824748421,27.665253726697));
#28213=CARTESIAN_POINT('',(-4.76403458719828,1.22194824541733,27.3196847251172));
#28214=CARTESIAN_POINT('',(-4.76403458704967,1.22194824599672,-3.23514056400928));
#28215=CARTESIAN_POINT('',(-4.91825002738015,0.00010786925271452,25.9850428854515));
#28216=CARTESIAN_POINT('Ctrl Pts',(-4.76403458666814,1.22194824748421,27.665253726697));
#28217=CARTESIAN_POINT('Ctrl Pts',(-4.76064996511665,1.23514394064655,27.6644742206369));
#28218=CARTESIAN_POINT('Ctrl Pts',(-4.7572104390177,1.24832588052699,27.6636945838257));
#28219=CARTESIAN_POINT('Ctrl Pts',(-4.71472557611052,1.40842257577462,27.6542144107116));
#28220=CARTESIAN_POINT('Ctrl Pts',(-4.66894380530174,1.55346573809053,27.645506153256));
#28221=CARTESIAN_POINT('Ctrl Pts',(-4.60181203668596,1.73618183649792,27.6344238022613));
#28222=CARTESIAN_POINT('Ctrl Pts',(-4.58658610954864,1.7760150072666,27.6320009900598));
#28223=CARTESIAN_POINT('Ctrl Pts',(-4.55564695658767,1.85390358612041,27.6272524850546));
#28224=CARTESIAN_POINT('Ctrl Pts',(-4.53997008276712,1.8919697126724,27.6249266255795));
#28225=CARTESIAN_POINT('Ctrl Pts',(-4.51383836417046,1.95322631117566,27.6211714560554));
#28226=CARTESIAN_POINT('Ctrl Pts',(-4.50367835575932,1.97654017861358,27.6197393329264));
#28227=CARTESIAN_POINT('Ctrl Pts',(-4.43219185283861,2.13716481521198,27.6098483184765));
#28228=CARTESIAN_POINT('Ctrl Pts',(-4.36477612579108,2.27167957594816,27.6014399966203));
#28229=CARTESIAN_POINT('Ctrl Pts',(-4.26230244143279,2.45468620632135,27.5896853908593));
#28230=CARTESIAN_POINT('Ctrl Pts',(-4.23236678175184,2.50594849424051,27.5863570348855));
#28231=CARTESIAN_POINT('Ctrl Pts',(-4.15183028490007,2.63829908330319,27.5776573184999));
#28232=CARTESIAN_POINT('Ctrl Pts',(-4.0997811906588,2.71847579392088,27.5722799167477));
#28233=CARTESIAN_POINT('Ctrl Pts',(-4.00714440926774,2.85245658919234,27.5630825130861));
#28234=CARTESIAN_POINT('Ctrl Pts',(-3.96772652645394,2.90703646133973,27.5592731077788));
#28235=CARTESIAN_POINT('Ctrl Pts',(-3.874814923407,3.03027471692886,27.550518062231));
#28236=CARTESIAN_POINT('Ctrl Pts',(-3.82059439056381,3.09835662658847,27.5455675823048));
#28237=CARTESIAN_POINT('Ctrl Pts',(-3.6436142650878,3.30886736111055,27.5298814541515));
#28238=CARTESIAN_POINT('Ctrl Pts',(-3.51448050112049,3.44571532237051,27.51910618738));
#28239=CARTESIAN_POINT('Ctrl Pts',(-3.32462576279781,3.62510758844716,27.504173950256));
#28240=CARTESIAN_POINT('Ctrl Pts',(-3.27030313309836,3.67418822170003,27.4999961848289));
#28241=CARTESIAN_POINT('Ctrl Pts',(-3.1885415628719,3.74480965037837,27.493852651144));
#28242=CARTESIAN_POINT('Ctrl Pts',(-3.16193685642271,3.76730035618366,27.49187536492));
#28243=CARTESIAN_POINT('Ctrl Pts',(-3.1011402483738,3.81759797281668,27.4874072372669));
#28244=CARTESIAN_POINT('Ctrl Pts',(-3.0668089789828,3.84523183566234,27.4849190976179));
#28245=CARTESIAN_POINT('Ctrl Pts',(-2.98904530750111,3.90612121022145,27.4793539751629));
#28246=CARTESIAN_POINT('Ctrl Pts',(-2.94542011511696,3.93912111763403,27.4762800610756));
#28247=CARTESIAN_POINT('Ctrl Pts',(-2.78608496067803,4.05552168112575,27.4652050227098));
#28248=CARTESIAN_POINT('Ctrl Pts',(-2.66731111347218,4.13460724979505,27.4572304922474));
#28249=CARTESIAN_POINT('Ctrl Pts',(-2.44801899439175,4.26723598243721,27.4428568356669));
#28250=CARTESIAN_POINT('Ctrl Pts',(-2.34876106128912,4.32266363918994,27.4364715963063));
#28251=CARTESIAN_POINT('Ctrl Pts',(-2.18697814426443,4.4057877925507,27.4262098583004));
#28252=CARTESIAN_POINT('Ctrl Pts',(-2.12564105470533,4.43570619463604,27.4223517511758));
#28253=CARTESIAN_POINT('Ctrl Pts',(-1.99176054517494,4.49759430032889,27.4139916974572));
#28254=CARTESIAN_POINT('Ctrl Pts',(-1.9190265629286,4.52910602667835,27.4094875489816));
#28255=CARTESIAN_POINT('Ctrl Pts',(-1.69731274489711,4.61886271730072,27.395859724521));
#28256=CARTESIAN_POINT('Ctrl Pts',(-1.54622382371118,4.67161153653316,27.3867063946848));
#28257=CARTESIAN_POINT('Ctrl Pts',(-1.28069652815407,4.75001801494066,27.3708589550009));
#28258=CARTESIAN_POINT('Ctrl Pts',(-1.16741108866242,4.77912194835796,27.3641714159793));
#28259=CARTESIAN_POINT('Ctrl Pts',(-1.01822230305812,4.81182795844294,27.3554831431432));
#28260=CARTESIAN_POINT('Ctrl Pts',(-0.983166313800091,4.81911288473193,
27.353450136301));
#28261=CARTESIAN_POINT('Ctrl Pts',(-0.906667609463635,4.83414047086758,
27.3490338982472));
#28262=CARTESIAN_POINT('Ctrl Pts',(-0.865198451120929,4.84173439395674,
27.3466526685673));
#28263=CARTESIAN_POINT('Ctrl Pts',(-0.773235502627993,4.857355605201,27.3413943076014));
#28264=CARTESIAN_POINT('Ctrl Pts',(-0.722703773281822,4.86513061892693,
27.338519729489));
#28265=CARTESIAN_POINT('Ctrl Pts',(-0.552666011687396,4.88858562741374,
27.3288815440531));
#28266=CARTESIAN_POINT('Ctrl Pts',(-0.432706841024413,4.90066058416014,
27.3221383498482));
#28267=CARTESIAN_POINT('Ctrl Pts',(-0.180503025085497,4.9167139099475,27.3079759729082));
#28268=CARTESIAN_POINT('Ctrl Pts',(-0.0482973586361654,4.91978899569347,
27.3005599703677));
#28269=CARTESIAN_POINT('Ctrl Pts',(0.146919523155377,4.91645950808169,27.2895530335701));
#28270=CARTESIAN_POINT('Ctrl Pts',(0.209941926458302,4.91417172282328,27.2859912497351));
#28271=CARTESIAN_POINT('Ctrl Pts',(0.344877120279991,4.90667292419014,27.2783401675765));
#28272=CARTESIAN_POINT('Ctrl Pts',(0.416754548684503,4.90109119449554,27.2742492427617));
#28273=CARTESIAN_POINT('Ctrl Pts',(0.631465975187671,4.87965999625878,27.2619735399502));
#28274=CARTESIAN_POINT('Ctrl Pts',(0.77375355326237,4.85912909117222,27.253763005014));
#28275=CARTESIAN_POINT('Ctrl Pts',(1.04582118161549,4.80761751102473,27.2379140907233));
#28276=CARTESIAN_POINT('Ctrl Pts',(1.17564618194848,4.77752912240826,27.2302844844276));
#28277=CARTESIAN_POINT('Ctrl Pts',(1.35203791184395,4.72902203616986,27.2198552035504));
#28278=CARTESIAN_POINT('Ctrl Pts',(1.39978359947179,4.71510995505442,27.2170259562016));
#28279=CARTESIAN_POINT('Ctrl Pts',(1.48336692702505,4.68937404645186,27.2120653086015));
#28280=CARTESIAN_POINT('Ctrl Pts',(1.51929435034912,4.67785753215388,27.2099308855668));
#28281=CARTESIAN_POINT('Ctrl Pts',(1.63107751393597,4.64060182953047,27.2032786634592));
#28282=CARTESIAN_POINT('Ctrl Pts',(1.70643958853681,4.61342209022953,27.1987767585127));
#28283=CARTESIAN_POINT('Ctrl Pts',(1.94585397673784,4.52040645982469,27.1843651287646));
#28284=CARTESIAN_POINT('Ctrl Pts',(2.1070327679654,4.44756508149975,27.1744905806663));
#28285=CARTESIAN_POINT('Ctrl Pts',(2.33679635745353,4.32842938821258,27.1599508385517));
#28286=CARTESIAN_POINT('Ctrl Pts',(2.40869499412891,4.28883508742562,27.1553317773876));
#28287=CARTESIAN_POINT('Ctrl Pts',(2.53785697157189,4.21343333173724,27.1468890915158));
#28288=CARTESIAN_POINT('Ctrl Pts',(2.5954382013193,4.17821000643685,27.1430708264778));
#28289=CARTESIAN_POINT('Ctrl Pts',(2.72321235052482,4.09638779933686,27.1344660712232));
#28290=CARTESIAN_POINT('Ctrl Pts',(2.79296949765636,4.04914801503473,27.1296756625979));
#28291=CARTESIAN_POINT('Ctrl Pts',(3.01703128682595,3.88886665497159,27.1139684256475));
#28292=CARTESIAN_POINT('Ctrl Pts',(3.16596041457574,3.7686145058122,27.1030077072156));
#28293=CARTESIAN_POINT('Ctrl Pts',(3.36369269603077,3.5889438410337,27.0877322332719));
#28294=CARTESIAN_POINT('Ctrl Pts',(3.41868973334464,3.53659541807505,27.0833987732702));
#28295=CARTESIAN_POINT('Ctrl Pts',(3.4972102838737,3.45831250770342,27.0770935067622));
#28296=CARTESIAN_POINT('Ctrl Pts',(3.52170357172565,3.43336703032634,27.0751091512852));
#28297=CARTESIAN_POINT('Ctrl Pts',(3.57626947536161,3.37659543238593,27.0706500002222));
#28298=CARTESIAN_POINT('Ctrl Pts',(3.60618729483753,3.34462454237405,27.0681778028635));
#28299=CARTESIAN_POINT('Ctrl Pts',(3.67214701018624,3.27222437387932,27.0626588042039));
#28300=CARTESIAN_POINT('Ctrl Pts',(3.70795607643927,3.23159060307155,27.0596149917805));
#28301=CARTESIAN_POINT('Ctrl Pts',(3.83326393563282,3.08457389389448,27.0487722407558));
#28302=CARTESIAN_POINT('Ctrl Pts',(3.91891484837524,2.97499833659421,27.0409988678308));
#28303=CARTESIAN_POINT('Ctrl Pts',(4.06165631414309,2.77550490662336,27.0272430812276));
#28304=CARTESIAN_POINT('Ctrl Pts',(4.12068495731941,2.68708664159231,27.0212740155317));
#28305=CARTESIAN_POINT('Ctrl Pts',(4.21013213851027,2.54321749510737,27.0117238845032));
#28306=CARTESIAN_POINT('Ctrl Pts',(4.24242669102736,2.48897238134715,27.0081584266551));
#28307=CARTESIAN_POINT('Ctrl Pts',(4.30929395651268,2.37157128262066,27.0005095079028));
#28308=CARTESIAN_POINT('Ctrl Pts',(4.34354216065408,2.30824740636024,26.9964244660516));
#28309=CARTESIAN_POINT('Ctrl Pts',(4.39474752026173,2.20839222607463,26.9900404791641));
#28310=CARTESIAN_POINT('Ctrl Pts',(4.41266703051343,2.17236544895714,26.9877486659967));
#28311=CARTESIAN_POINT('Ctrl Pts',(4.51411473668546,1.96197129839419,26.9744291338578));
#28312=CARTESIAN_POINT('Ctrl Pts',(4.58774466734351,1.78302022990197,26.9633474004599));
#28313=CARTESIAN_POINT('Ctrl Pts',(4.67438371846522,1.53122224161548,26.9481255631684));
#28314=CARTESIAN_POINT('Ctrl Pts',(4.69658115126848,1.46172171490275,26.9439626184082));
#28315=CARTESIAN_POINT('Ctrl Pts',(4.72793355463609,1.35545547087873,26.9376632577862));
#28316=CARTESIAN_POINT('Ctrl Pts',(4.73822334484207,1.31903556602557,26.9355160209801));
#28317=CARTESIAN_POINT('Ctrl Pts',(4.76051713811959,1.23649913735366,26.9306775392048));
#28318=CARTESIAN_POINT('Ctrl Pts',(4.77227333332955,1.19031963983346,26.927989157465));
#28319=CARTESIAN_POINT('Ctrl Pts',(4.81949318119061,0.992877276003605,26.9165584291248));
#28320=CARTESIAN_POINT('Ctrl Pts',(4.84845019829669,0.840149594657339,26.907871860414));
#28321=CARTESIAN_POINT('Ctrl Pts',(4.88943092519163,0.549344588365354,26.891414914993));
#28322=CARTESIAN_POINT('Ctrl Pts',(4.90294542595198,0.411630541058711,26.88365631214));
#28323=CARTESIAN_POINT('Ctrl Pts',(4.91412316198807,0.210959712626267,26.8723242173166));
#28324=CARTESIAN_POINT('Ctrl Pts',(4.91641224255763,0.148327365530215,26.8687838896767));
#28325=CARTESIAN_POINT('Ctrl Pts',(4.91877088284774,0.0129383021127199,
26.8611166523174));
#28326=CARTESIAN_POINT('Ctrl Pts',(4.91842422953663,-0.0598107800746115,
26.8569878329261));
#28327=CARTESIAN_POINT('Ctrl Pts',(4.9143286050754,-0.211752099166897,26.8483392282834));
#28328=CARTESIAN_POINT('Ctrl Pts',(4.91027825149939,-0.290915639716645,
26.8438187725225));
#28329=CARTESIAN_POINT('Ctrl Pts',(4.89098413574901,-0.546694666853374,
26.8291620544453));
#28330=CARTESIAN_POINT('Ctrl Pts',(4.86810643566972,-0.722592926676408,
26.8189991404571));
#28331=CARTESIAN_POINT('Ctrl Pts',(4.8249483881279,-0.955294051612906,26.805489534729));
#28332=CARTESIAN_POINT('Ctrl Pts',(4.81305505929978,-1.01351605319028,26.8021044849998));
#28333=CARTESIAN_POINT('Ctrl Pts',(4.79210261696473,-1.10737811894963,26.7966441315826));
#28334=CARTESIAN_POINT('Ctrl Pts',(4.7836938257061,-1.14315668679057,26.7945623471964));
#28335=CARTESIAN_POINT('Ctrl Pts',(4.76019350058588,-1.23834477064705,26.7890212947696));
#28336=CARTESIAN_POINT('Ctrl Pts',(4.74439106995902,-1.29757213460608,26.7855700165795));
#28337=CARTESIAN_POINT('Ctrl Pts',(4.70163834685193,-1.44656918815566,26.7768588656913));
#28338=CARTESIAN_POINT('Ctrl Pts',(4.67322156482481,-1.53589255807802,26.771609522555));
#28339=CARTESIAN_POINT('Ctrl Pts',(4.58886742171799,-1.77697037894829,26.7573009755254));
#28340=CARTESIAN_POINT('Ctrl Pts',(4.52797145819568,-1.9268631519593,26.748246425354));
#28341=CARTESIAN_POINT('Ctrl Pts',(4.4293459748742,-2.13899433707183,26.7350670915183));
#28342=CARTESIAN_POINT('Ctrl Pts',(4.39744829908983,-2.20382640813193,26.7309882800607));
#28343=CARTESIAN_POINT('Ctrl Pts',(4.33110799349748,-2.33148368999399,26.7228442466557));
#28344=CARTESIAN_POINT('Ctrl Pts',(4.2966976653546,-2.39430609174228,26.7187801881253));
#28345=CARTESIAN_POINT('Ctrl Pts',(4.18117738833755,-2.59469396752875,26.705623068095));
#28346=CARTESIAN_POINT('Ctrl Pts',(4.09473774498144,-2.7290662853541,26.6964953200188));
#28347=CARTESIAN_POINT('Ctrl Pts',(3.92196476841252,-2.9709076771374,26.6794815137971));
#28348=CARTESIAN_POINT('Ctrl Pts',(3.83735288569841,-3.079419346278,26.6716069654977));
#28349=CARTESIAN_POINT('Ctrl Pts',(3.72136750334687,-3.2159505495092,26.6614102768428));
#28350=CARTESIAN_POINT('Ctrl Pts',(3.69402958449487,-3.2473157401144,26.65904696373));
#28351=CARTESIAN_POINT('Ctrl Pts',(3.63819695717747,-3.30975574758314,26.654302114897));
#28352=CARTESIAN_POINT('Ctrl Pts',(3.60969403369218,-3.34081864912121,26.6519209105823));
#28353=CARTESIAN_POINT('Ctrl Pts',(3.54575033274494,-3.4087315984533,26.6466626217176));
#28354=CARTESIAN_POINT('Ctrl Pts',(3.51012718253375,-3.44540327975182,26.6437880902243));
#28355=CARTESIAN_POINT('Ctrl Pts',(3.38862565914825,-3.56664045899597,26.6341502151322));
#28356=CARTESIAN_POINT('Ctrl Pts',(3.30021224138485,-3.64860348596269,26.6274072833686));
#28357=CARTESIAN_POINT('Ctrl Pts',(3.10868852854766,-3.8134913716271,26.6132443678981));
#28358=CARTESIAN_POINT('Ctrl Pts',(3.00506369191737,-3.8956709818707,26.6058275618341));
#28359=CARTESIAN_POINT('Ctrl Pts',(2.84730966573292,-4.0107339661912,26.5948198824504));
#28360=CARTESIAN_POINT('Ctrl Pts',(2.79565460639087,-4.04690925212025,26.5912581688691));
#28361=CARTESIAN_POINT('Ctrl Pts',(2.68348682992467,-4.12229039869624,26.5836070437771));
#28362=CARTESIAN_POINT('Ctrl Pts',(2.62277871392765,-4.16117908204585,26.5795160048968));
#28363=CARTESIAN_POINT('Ctrl Pts',(2.43854776265057,-4.27356082551775,26.5672389237854));
#28364=CARTESIAN_POINT('Ctrl Pts',(2.31263710137224,-4.34298815174005,26.5590271146051));
#28365=CARTESIAN_POINT('Ctrl Pts',(2.0648012072018,-4.46580764068894,26.5431954614029));
#28366=CARTESIAN_POINT('Ctrl Pts',(1.94339033898596,-4.51996419008817,26.5355844203629));
#28367=CARTESIAN_POINT('Ctrl Pts',(1.77360090035928,-4.58759309109774,26.5251650076955));
#28368=CARTESIAN_POINT('Ctrl Pts',(1.72698825890711,-4.60534278391403,26.5223273599875));
#28369=CARTESIAN_POINT('Ctrl Pts',(1.64468872980568,-4.63525649118953,26.5173602912255));
#28370=CARTESIAN_POINT('Ctrl Pts',(1.6091173639672,-4.64772472211019,26.5152277931673));
#28371=CARTESIAN_POINT('Ctrl Pts',(1.49800159162702,-4.68524367862435,26.5086064342846));
#28372=CARTESIAN_POINT('Ctrl Pts',(1.42198976562632,-4.7088706134757,26.5041332318151));
#28373=CARTESIAN_POINT('Ctrl Pts',(1.19088013671228,-4.77460027483214,26.4906511007212));
#28374=CARTESIAN_POINT('Ctrl Pts',(1.03426150879265,-4.81095691991202,26.481670528841));
#28375=CARTESIAN_POINT('Ctrl Pts',(0.778333401567124,-4.85728944992974,
26.4670702921644));
#28376=CARTESIAN_POINT('Ctrl Pts',(0.680008613754562,-4.87202746556686,
26.4614793409982));
#28377=CARTESIAN_POINT('Ctrl Pts',(0.516820198808213,-4.89145144586059,
26.4522019503655));
#28378=CARTESIAN_POINT('Ctrl Pts',(0.452189419176299,-4.89784901508398,
26.4485282482567));
#28379=CARTESIAN_POINT('Ctrl Pts',(0.315824625756783,-4.90862509277537,
26.4407716597912));
#28380=CARTESIAN_POINT('Ctrl Pts',(0.244082985159172,-4.91271501681042,
26.4366877325577));
#28381=CARTESIAN_POINT('Ctrl Pts',(0.080506099021611,-4.91844836047242,
26.4273631404639));
#28382=CARTESIAN_POINT('Ctrl Pts',(-0.0113373198127981,-4.91909409761994,
26.4221182616299));
#28383=CARTESIAN_POINT('Ctrl Pts',(-0.290191398105914,-4.91324475883017,
26.4061633589779));
#28384=CARTESIAN_POINT('Ctrl Pts',(-0.476863367831023,-4.89865158055568,
26.3954359061231));
#28385=CARTESIAN_POINT('Ctrl Pts',(-0.701075958242673,-4.86818352561199,
26.3825649330758));
#28386=CARTESIAN_POINT('Ctrl Pts',(-0.739837655438666,-4.86244369047897,
26.3803406367033));
#28387=CARTESIAN_POINT('Ctrl Pts',(-0.815656108875953,-4.85028887539322,
26.3759931987426));
#28388=CARTESIAN_POINT('Ctrl Pts',(-0.852715979703553,-4.84391087442513,
26.3738694840199));
#28389=CARTESIAN_POINT('Ctrl Pts',(-0.893477122236693,-4.83641359369834,
26.3715330345062));
#28390=CARTESIAN_POINT('Ctrl Pts',(-0.897254130788829,-4.83571430525909,
26.3713165285209));
#28391=CARTESIAN_POINT('Ctrl Pts',(-0.905498595786359,-4.83417790471142,
26.370843921455));
#28392=CARTESIAN_POINT('Ctrl Pts',(-0.909965719689209,-4.83333902291333,
26.3705878362863));
#28393=CARTESIAN_POINT('Ctrl Pts',(-0.970764398347969,-4.82183435507857,
26.3671022590888));
#28394=CARTESIAN_POINT('Ctrl Pts',(-1.02690678412038,-4.81019049555959,
26.3638813134181));
#28395=CARTESIAN_POINT('Ctrl Pts',(-1.24077041667061,-4.76192049122991,
26.3515794844854));
#28396=CARTESIAN_POINT('Ctrl Pts',(-1.39685108212735,-4.71849606398248,
26.3425307538868));
#28397=CARTESIAN_POINT('Ctrl Pts',(-1.64402203672741,-4.63638707311834,
26.3279091109782));
#28398=CARTESIAN_POINT('Ctrl Pts',(-1.73658321896128,-4.60251799943816,
26.3223660724372));
#28399=CARTESIAN_POINT('Ctrl Pts',(-1.87641862523985,-4.54653156012294,
26.3138624481865));
#28400=CARTESIAN_POINT('Ctrl Pts',(-1.92446276681263,-4.52640465290204,
26.3109169509253));
#28401=CARTESIAN_POINT('Ctrl Pts',(-2.03939878595792,-4.47609429003001,
26.3038085132982));
#28402=CARTESIAN_POINT('Ctrl Pts',(-2.10595222314233,-4.44516957677413,
26.2996409284886));
#28403=CARTESIAN_POINT('Ctrl Pts',(-2.24767910674318,-4.37541725628407,
26.290647681846));
#28404=CARTESIAN_POINT('Ctrl Pts',(-2.32259321675628,-4.33611555257538,
26.2858201376729));
#28405=CARTESIAN_POINT('Ctrl Pts',(-2.5512966163641,-4.2085043421337,26.2708470617046));
#28406=CARTESIAN_POINT('Ctrl Pts',(-2.70135190529194,-4.11379646437946,
26.2606801329224));
#28407=CARTESIAN_POINT('Ctrl Pts',(-2.88773957098651,-3.98155332275614,
26.2476484521273));
#28408=CARTESIAN_POINT('Ctrl Pts',(-2.9290491304873,-3.95126283213868,26.2447335599257));
#28409=CARTESIAN_POINT('Ctrl Pts',(-2.99762864449907,-3.89930988744348,
26.2398525423825));
#28410=CARTESIAN_POINT('Ctrl Pts',(-3.02515491053225,-3.87799340885901,
26.2378820988019));
#28411=CARTESIAN_POINT('Ctrl Pts',(-3.05968157330942,-3.85066445242693,
26.2353948780981));
#28412=CARTESIAN_POINT('Ctrl Pts',(-3.06689419292561,-3.84492237440164,
26.2348744114903));
#28413=CARTESIAN_POINT('Ctrl Pts',(-3.08050459899719,-3.83402425569698,
26.2338905452295));
#28414=CARTESIAN_POINT('Ctrl Pts',(-3.0869056901489,-3.8288723977435,26.2334270954222));
#28415=CARTESIAN_POINT('Ctrl Pts',(-3.10291754508265,-3.81591915510387,
26.2322659308781));
#28416=CARTESIAN_POINT('Ctrl Pts',(-3.11251183270786,-3.80809747541361,
26.2315684571914));
#28417=CARTESIAN_POINT('Ctrl Pts',(-3.16847594732679,-3.76212030980905,
26.2274896610047));
#28418=CARTESIAN_POINT('Ctrl Pts',(-3.21417365981904,-3.72315415049807,
26.2241171454808));
#28419=CARTESIAN_POINT('Ctrl Pts',(-3.39773050482049,-3.56073762100317,
26.2103682015441));
#28420=CARTESIAN_POINT('Ctrl Pts',(-3.52928312686911,-3.43039143590329,
26.2000305896804));
#28421=CARTESIAN_POINT('Ctrl Pts',(-3.70921370855081,-3.23077721904066,
26.1849228291555));
#28422=CARTESIAN_POINT('Ctrl Pts',(-3.76365347986991,-3.16719118956933,
26.1802079751842));
#28423=CARTESIAN_POINT('Ctrl Pts',(-3.83250274439961,-3.08249151982606,
26.1740399489608));
#28424=CARTESIAN_POINT('Ctrl Pts',(-3.84840803776563,-3.06261111198495,
26.1726000434062));
#28425=CARTESIAN_POINT('Ctrl Pts',(-3.8714032244837,-3.0334068783846,26.1704959022487));
#28426=CARTESIAN_POINT('Ctrl Pts',(-3.87861534485782,-3.02417976024834,
26.1698326914501));
#28427=CARTESIAN_POINT('Ctrl Pts',(-3.89023284715783,-3.00920652010283,
26.1687590178432));
#28428=CARTESIAN_POINT('Ctrl Pts',(-3.89465862316918,-3.00347626834985,
26.1683487234224));
#28429=CARTESIAN_POINT('Ctrl Pts',(-3.90426824045027,-2.99097730790976,
26.1674550754577));
#28430=CARTESIAN_POINT('Ctrl Pts',(-3.90944716653823,-2.98420485248403,
26.1669716836808));
#28431=CARTESIAN_POINT('Ctrl Pts',(-3.96461188899948,-2.91167616544092,
26.1618035901253));
#28432=CARTESIAN_POINT('Ctrl Pts',(-4.01295079305615,-2.84468473177401,
26.1571062475886));
#28433=CARTESIAN_POINT('Ctrl Pts',(-4.11787063596362,-2.69127967795946,
26.1465101734134));
#28434=CARTESIAN_POINT('Ctrl Pts',(-4.17346312471482,-2.60423696052733,
26.1406071861521));
#28435=CARTESIAN_POINT('Ctrl Pts',(-4.30661010575211,-2.38053849813489,
26.1257079032542));
#28436=CARTESIAN_POINT('Ctrl Pts',(-4.38043473350752,-2.24179535634945,
26.116709422727));
#28437=CARTESIAN_POINT('Ctrl Pts',(-4.465047696652,-2.06257670001851,26.1054302956516));
#28438=CARTESIAN_POINT('Ctrl Pts',(-4.48213459307556,-2.02517730684825,
26.1030950568623));
#28439=CARTESIAN_POINT('Ctrl Pts',(-4.51521357793691,-1.95030483789718,
26.0984587733466));
#28440=CARTESIAN_POINT('Ctrl Pts',(-4.53121301799591,-1.91283853226417,
26.0961576911522));
#28441=CARTESIAN_POINT('Ctrl Pts',(-4.63989458995137,-1.64931818970439,
26.0800878910288));
#28442=CARTESIAN_POINT('Ctrl Pts',(-4.7160860033962,-1.41683011621999,26.0664808773928));
#28443=CARTESIAN_POINT('Ctrl Pts',(-4.79422268247865,-1.10056653420995,
26.0481782450019));
#28444=CARTESIAN_POINT('Ctrl Pts',(-4.81179183044261,-1.02101763275938,
26.0435933944782));
#28445=CARTESIAN_POINT('Ctrl Pts',(-4.8397925158082,-0.877383363066244,
26.0353321621244));
#28446=CARTESIAN_POINT('Ctrl Pts',(-4.85094621396667,-0.813457971635867,
26.0316615536937));
#28447=CARTESIAN_POINT('Ctrl Pts',(-4.87052539044151,-0.686449919960619,
26.0243744957381));
#28448=CARTESIAN_POINT('Ctrl Pts',(-4.87899780821496,-0.623386998595736,
26.0207590700356));
#28449=CARTESIAN_POINT('Ctrl Pts',(-4.90756838396048,-0.374175436473399,
26.0064755421049));
#28450=CARTESIAN_POINT('Ctrl Pts',(-4.91825410378982,-0.187108860318732,
25.9957559094304));
#28451=CARTESIAN_POINT('Ctrl Pts',(-4.91824999881774,0.000107839092156406,
25.985042837665));
#28452=CARTESIAN_POINT('Ctrl Pts',(-4.91824999881714,0.00010786642811769,
25.9850428361008));
#28453=CARTESIAN_POINT('Ctrl Pts',(-4.91824859447662,0.0641398167640534,
25.9813787458714));
#28454=CARTESIAN_POINT('Ctrl Pts',(-4.91699671764731,0.12816596342371,25.9777175108798));
#28455=CARTESIAN_POINT('Ctrl Pts',(-4.91299657002833,0.23047530219885,25.9718756339816));
#28456=CARTESIAN_POINT('Ctrl Pts',(-4.91104981305733,0.268782304395479,
25.9696902343865));
#28457=CARTESIAN_POINT('Ctrl Pts',(-4.90660886371666,0.339774585574197,
25.965645209907));
#28458=CARTESIAN_POINT('Ctrl Pts',(-4.90423561074501,0.372465318778533,
25.9637845410905));
#28459=CARTESIAN_POINT('Ctrl Pts',(-4.89805355438409,0.447259984964282,
25.9595333058903));
#28460=CARTESIAN_POINT('Ctrl Pts',(-4.89402830481027,0.48934356351924,25.9571455411912));
#28461=CARTESIAN_POINT('Ctrl Pts',(-4.8751761641213,0.662813556767806,25.9473094579166));
#28462=CARTESIAN_POINT('Ctrl Pts',(-4.85559662887549,0.793628730723643,
25.9399057938522));
#28463=CARTESIAN_POINT('Ctrl Pts',(-4.81162092519639,1.02366360476718,25.9267854602727));
#28464=CARTESIAN_POINT('Ctrl Pts',(-4.78936417432496,1.12319526975691,25.9210745997888));
#28465=CARTESIAN_POINT('Ctrl Pts',(-4.76403457790608,1.22194828164502,25.9153493127618));
#28466=CARTESIAN_POINT('',(-4.91787650032817,4.95708214059191E-5,25.6398490687309));
#28467=CARTESIAN_POINT('Ctrl Pts',(-4.76438990516341,1.22203958205891,25.5699245627443));
#28468=CARTESIAN_POINT('Ctrl Pts',(-4.77868589190668,1.16644466560101,25.5731760999306));
#28469=CARTESIAN_POINT('Ctrl Pts',(-4.87410541215778,0.766055703403716,
25.5964877222952));
#28470=CARTESIAN_POINT('Ctrl Pts',(-4.91798476554411,0.354353816740224,
25.6197993446597));
#28471=CARTESIAN_POINT('Ctrl Pts',(-4.91785849824545,5.01597051061138E-5,
25.6398594298379));
#28472=CARTESIAN_POINT('Ctrl Pts',(-4.91824999985816,3.73529137002939E-5,
25.6396341009043));
#28473=CARTESIAN_POINT('Ctrl Pts',(-4.91825040859229,-0.0537805815385731,
25.6426695501133));
#28474=CARTESIAN_POINT('Ctrl Pts',(-4.91736746376412,-0.107594589358031,
25.6457101258233));
#28475=CARTESIAN_POINT('Ctrl Pts',(-4.91368567495012,-0.219739063851807,
25.6520618332672));
#28476=CARTESIAN_POINT('Ctrl Pts',(-4.91073079301712,-0.278056036895246,
25.6553735176413));
#28477=CARTESIAN_POINT('Ctrl Pts',(-4.89794772651726,-0.464562163061656,
25.6659983254188));
#28478=CARTESIAN_POINT('Ctrl Pts',(-4.88413191376792,-0.592422708574879,
25.6733344125371));
#28479=CARTESIAN_POINT('Ctrl Pts',(-4.83785904150373,-0.905283383512189,
25.6914253924981));
#28480=CARTESIAN_POINT('Ctrl Pts',(-4.79978685301425,-1.08924979830331,
25.7021890384979));
#28481=CARTESIAN_POINT('Ctrl Pts',(-4.74267753754525,-1.30280657669003,
25.7147647340652));
#28482=CARTESIAN_POINT('Ctrl Pts',(-4.73373465495577,-1.33493499672673,
25.7166586611372));
#28483=CARTESIAN_POINT('Ctrl Pts',(-4.71307798310571,-1.40632773011291,
25.7208702750094));
#28484=CARTESIAN_POINT('Ctrl Pts',(-4.70119888806464,-1.44554170314726,
25.7231855202486));
#28485=CARTESIAN_POINT('Ctrl Pts',(-4.66185901973552,-1.56978906912364,
25.7305350828253));
#28486=CARTESIAN_POINT('Ctrl Pts',(-4.63257017947281,-1.65422521931918,
25.7355507560079));
#28487=CARTESIAN_POINT('Ctrl Pts',(-4.55060396554596,-1.87123671444251,
25.74855645122));
#28488=CARTESIAN_POINT('Ctrl Pts',(-4.4944314471968,-2.00240084949664,25.7565324253232));
#28489=CARTESIAN_POINT('Ctrl Pts',(-4.40034139238856,-2.19812086833262,
25.7687240375858));
#28490=CARTESIAN_POINT('Ctrl Pts',(-4.36652104575094,-2.26456034090919,
25.7729152997698));
#28491=CARTESIAN_POINT('Ctrl Pts',(-4.30104537182488,-2.38626143498539,
25.7807053323999));
#28492=CARTESIAN_POINT('Ctrl Pts',(-4.26980158285057,-2.44172669635751,
25.7843004517781));
#28493=CARTESIAN_POINT('Ctrl Pts',(-4.2043133732387,-2.55288148334038,25.791603956434));
#28494=CARTESIAN_POINT('Ctrl Pts',(-4.17001752754772,-2.6085261176518,25.7953120739215));
#28495=CARTESIAN_POINT('Ctrl Pts',(-4.01705790516058,-2.84597212864427,
25.8113729266473));
#28496=CARTESIAN_POINT('Ctrl Pts',(-3.88753937882274,-3.02048782914107,
25.8238035693995));
#28497=CARTESIAN_POINT('Ctrl Pts',(-3.69736190117411,-3.24415643752122,
25.8406007897869));
#28498=CARTESIAN_POINT('Ctrl Pts',(-3.64645131567586,-3.30127687115357,
25.8449728920762));
#28499=CARTESIAN_POINT('Ctrl Pts',(-3.58238140833934,-3.36987058295376,
25.8503200040556));
#28500=CARTESIAN_POINT('Ctrl Pts',(-3.57046700460818,-3.38249163677978,
25.851307998478));
#28501=CARTESIAN_POINT('Ctrl Pts',(-3.53572481569087,-3.41890630385694,
25.8541704363925));
#28502=CARTESIAN_POINT('Ctrl Pts',(-3.51272413658165,-3.44253387118795,
25.8560425433234));
#28503=CARTESIAN_POINT('Ctrl Pts',(-3.4639499993639,-3.49163954099752,25.8599635783725));
#28504=CARTESIAN_POINT('Ctrl Pts',(-3.43812898162748,-3.51706773077636,
25.8620115186904));
#28505=CARTESIAN_POINT('Ctrl Pts',(-3.31963520249257,-3.63120675998014,
25.8712922229284));
#28506=CARTESIAN_POINT('Ctrl Pts',(-3.22379343426538,-3.71655715237029,
25.8784793836466));
#28507=CARTESIAN_POINT('Ctrl Pts',(-3.05546061576027,-3.85504707898954,
25.8906915275745));
#28508=CARTESIAN_POINT('Ctrl Pts',(-2.98465202713447,-3.91012528812961,
25.8957138257999));
#28509=CARTESIAN_POINT('Ctrl Pts',(-2.84802385193446,-4.01052626171237,
25.9052261529284));
#28510=CARTESIAN_POINT('Ctrl Pts',(-2.78252866025655,-4.05624146875458,
25.9097127091704));
#28511=CARTESIAN_POINT('Ctrl Pts',(-2.66304590075251,-4.1353834612991,25.9177856209571));
#28512=CARTESIAN_POINT('Ctrl Pts',(-2.60946906248705,-4.16939815161943,
25.9213667842976));
#28513=CARTESIAN_POINT('Ctrl Pts',(-2.49988940170245,-4.23602807884815,
25.9286211505654));
#28514=CARTESIAN_POINT('Ctrl Pts',(-2.44387001459963,-4.26859228993453,
25.9322939985358));
#28515=CARTESIAN_POINT('Ctrl Pts',(-2.37879808908558,-4.3047178296398,25.9365227741421));
#28516=CARTESIAN_POINT('Ctrl Pts',(-2.37035838399485,-4.30937084416066,
25.9370705199698));
#28517=CARTESIAN_POINT('Ctrl Pts',(-2.18705071069695,-4.40973139603089,
25.9489519640084));
#28518=CARTESIAN_POINT('Ctrl Pts',(-2.00653981441087,-4.49474334129122,
25.9603577960101));
#28519=CARTESIAN_POINT('Ctrl Pts',(-1.74893341503838,-4.59744454929035,
25.9762310078727));
#28520=CARTESIAN_POINT('Ctrl Pts',(-1.67581759305062,-4.62459727881428,
25.9806917174213));
#28521=CARTESIAN_POINT('Ctrl Pts',(-1.58673872780013,-4.65528804670007,
25.9860670813078));
#28522=CARTESIAN_POINT('Ctrl Pts',(-1.57136454106792,-4.66049998061225,
25.9869927041249));
#28523=CARTESIAN_POINT('Ctrl Pts',(-1.54674636598691,-4.66871001162847,
25.9884714059344));
#28524=CARTESIAN_POINT('Ctrl Pts',(-1.5375188261714,-4.67175698780145,25.9890248862812));
#28525=CARTESIAN_POINT('Ctrl Pts',(-1.52192544953536,-4.67685478896045,
25.9899588673247));
#28526=CARTESIAN_POINT('Ctrl Pts',(-1.51556435619285,-4.67892001143318,
25.9903394984017));
#28527=CARTESIAN_POINT('Ctrl Pts',(-1.50464115804381,-4.68244177561402,
25.9909924665278));
#28528=CARTESIAN_POINT('Ctrl Pts',(-1.50008110489058,-4.68390463986185,
25.9912648646033));
#28529=CARTESIAN_POINT('Ctrl Pts',(-1.46381173816561,-4.69548144812348,
25.9934298924547));
#28530=CARTESIAN_POINT('Ctrl Pts',(-1.43200240630764,-4.70528001028981,
25.9953192834575));
#28531=CARTESIAN_POINT('Ctrl Pts',(-1.3586682919955,-4.72705734302042,25.9996522344145));
#28532=CARTESIAN_POINT('Ctrl Pts',(-1.31708006187238,-4.73881322923037,
26.0020928535323));
#28533=CARTESIAN_POINT('Ctrl Pts',(-1.15859548088905,-4.78136506264894,
26.0113415311648));
#28534=CARTESIAN_POINT('Ctrl Pts',(-1.0407318244373,-4.80839611628701,26.018113728618));
#28535=CARTESIAN_POINT('Ctrl Pts',(-0.803965475358392,-4.85358218279611,
26.0316176166877));
#28536=CARTESIAN_POINT('Ctrl Pts',(-0.68515453877262,-4.87177416621673,
26.0383447839683));
#28537=CARTESIAN_POINT('Ctrl Pts',(-0.495750199940035,-4.89370894214521,
26.0490564875577));
#28538=CARTESIAN_POINT('Ctrl Pts',(-0.425537172511849,-4.90031360823001,
26.0530244097853));
#28539=CARTESIAN_POINT('Ctrl Pts',(-0.290476346275886,-4.9100935398953,
26.0606629847065));
#28540=CARTESIAN_POINT('Ctrl Pts',(-0.225659827915283,-4.91349901821122,
26.0643313804438));
#28541=CARTESIAN_POINT('Ctrl Pts',(-0.101281824537473,-4.91756756016072,
26.071382255988));
#28542=CARTESIAN_POINT('Ctrl Pts',(-0.0417382149532846,-4.91843334272117,
26.0747627611501));
#28543=CARTESIAN_POINT('Ctrl Pts',(0.234591691365004,-4.91743291183178,
26.0904821790489));
#28544=CARTESIAN_POINT('Ctrl Pts',(0.451086288873915,-4.90231563740987,
26.1028989425571));
#28545=CARTESIAN_POINT('Ctrl Pts',(0.729249590932683,-4.86430568448546,
26.1189585800842));
#28546=CARTESIAN_POINT('Ctrl Pts',(0.792452379629289,-4.85440975576246,
26.1226137092565));
#28547=CARTESIAN_POINT('Ctrl Pts',(0.860793676013052,-4.84233898201005,
26.1265694001584));
#28548=CARTESIAN_POINT('Ctrl Pts',(0.866141335162508,-4.84138531382986,
26.1268789522083));
#28549=CARTESIAN_POINT('Ctrl Pts',(0.874551674958665,-4.83987108551856,
26.1273658202207));
#28550=CARTESIAN_POINT('Ctrl Pts',(0.877615419377672,-4.83931647366641,
26.1275431844897));
#28551=CARTESIAN_POINT('Ctrl Pts',(0.882438829332563,-4.83843858862532,
26.1278224277101));
#28552=CARTESIAN_POINT('Ctrl Pts',(0.884198847748647,-4.83811726408688,
26.1279243230252));
#28553=CARTESIAN_POINT('Ctrl Pts',(0.886972856960731,-4.8376092521557,26.12808492582));
#28554=CARTESIAN_POINT('Ctrl Pts',(0.887986964688287,-4.83742320621956,
26.1281436387854));
#28555=CARTESIAN_POINT('Ctrl Pts',(0.893133086309332,-4.83647743749058,
26.1284415827391));
#28556=CARTESIAN_POINT('Ctrl Pts',(0.897264186507807,-4.83571273887016,
26.1286807705489));
#28557=CARTESIAN_POINT('Ctrl Pts',(0.904777232580385,-4.83431205694023,
26.1291157875209));
#28558=CARTESIAN_POINT('Ctrl Pts',(0.908159499733299,-4.83367781586063,
26.1293116322337));
#28559=CARTESIAN_POINT('Ctrl Pts',(0.914339297063946,-4.83251226804212,
26.1296694736812));
#28560=CARTESIAN_POINT('Ctrl Pts',(0.917137036981733,-4.83198208050818,
26.1298314807881));
#28561=CARTESIAN_POINT('Ctrl Pts',(0.952632174762279,-4.82522361277532,
26.1318869216686));
#28562=CARTESIAN_POINT('Ctrl Pts',(0.985266196142221,-4.81866594857339,
26.1337771670697));
#28563=CARTESIAN_POINT('Ctrl Pts',(1.05808748839538,-4.80326212061486,26.1379949237472));
#28564=CARTESIAN_POINT('Ctrl Pts',(1.09823546317319,-4.79424186320412,26.1403199402036));
#28565=CARTESIAN_POINT('Ctrl Pts',(1.28373735212449,-4.75011169454736,26.1510724301594));
#28566=CARTESIAN_POINT('Ctrl Pts',(1.42755670843052,-4.7088879343418,26.1594393002119));
#28567=CARTESIAN_POINT('Ctrl Pts',(1.71143664854336,-4.61331422892605,26.1762199744508));
#28568=CARTESIAN_POINT('Ctrl Pts',(1.85133244635808,-4.55897477595555,26.1846252365243));
#28569=CARTESIAN_POINT('Ctrl Pts',(2.05452876874757,-4.46915008430794,26.1971434030274));
#28570=CARTESIAN_POINT('Ctrl Pts',(2.1198821306596,-4.43852346288277,26.2012184279503));
#28571=CARTESIAN_POINT('Ctrl Pts',(2.25009330177091,-4.37397039416366,26.20944709754));
#28572=CARTESIAN_POINT('Ctrl Pts',(2.31491523994003,-4.34001199742697,26.2136000244399));
#28573=CARTESIAN_POINT('Ctrl Pts',(2.51357490332917,-4.23022243736658,26.2265147976526));
#28574=CARTESIAN_POINT('Ctrl Pts',(2.6446293533403,-4.1495512085368,26.2353072501324));
#28575=CARTESIAN_POINT('Ctrl Pts',(2.88713303167341,-3.98411553545176,26.2521118233183));
#28576=CARTESIAN_POINT('Ctrl Pts',(2.99917130923328,-3.90047251353154,26.2601137333992));
#28577=CARTESIAN_POINT('Ctrl Pts',(3.13986554985452,-3.78578544069449,26.2704450151212));
#28578=CARTESIAN_POINT('Ctrl Pts',(3.17189798434813,-3.758987936902,26.272817110337));
#28579=CARTESIAN_POINT('Ctrl Pts',(3.23618731368198,-3.70379817253545,26.2776164356285));
#28580=CARTESIAN_POINT('Ctrl Pts',(3.26842124194076,-3.67538458879895,26.2800431605997));
#28581=CARTESIAN_POINT('Ctrl Pts',(3.38062651664995,-3.57383422029942,26.2885730710926));
#28582=CARTESIAN_POINT('Ctrl Pts',(3.45854956636096,-3.49847996069592,26.2946482350454));
#28583=CARTESIAN_POINT('Ctrl Pts',(3.64587904095812,-3.30494520139774,26.3097404047203));
#28584=CARTESIAN_POINT('Ctrl Pts',(3.75209073661534,-3.18385164988183,26.3187467637863));
#28585=CARTESIAN_POINT('Ctrl Pts',(3.90158449887951,-2.99551965493498,26.3322748885748));
#28586=CARTESIAN_POINT('Ctrl Pts',(3.94948008914669,-2.93208226831146,26.3367559177101));
#28587=CARTESIAN_POINT('Ctrl Pts',(4.03607887990098,-2.81140872363503,26.3451550564722));
#28588=CARTESIAN_POINT('Ctrl Pts',(4.07515431866081,-2.75446344510613,26.3490689653624));
#28589=CARTESIAN_POINT('Ctrl Pts',(4.17586748288883,-2.60085617079348,26.3595050471999));
#28590=CARTESIAN_POINT('Ctrl Pts',(4.23534647895956,-2.50283074145014,26.3660414440821));
#28591=CARTESIAN_POINT('Ctrl Pts',(4.36011015746943,-2.2800073449136,26.380640774059));
#28592=CARTESIAN_POINT('Ctrl Pts',(4.42357082275289,-2.15430155508098,26.3887061156512));
#28593=CARTESIAN_POINT('Ctrl Pts',(4.51259338007746,-1.95738650523794,26.4010583221707));
#28594=CARTESIAN_POINT('Ctrl Pts',(4.542052407799,-1.88802041228342,26.4053575015165));
#28595=CARTESIAN_POINT('Ctrl Pts',(4.58372911427865,-1.78325793209245,26.4117648966076));
#28596=CARTESIAN_POINT('Ctrl Pts',(4.59715532277651,-1.74835478078894,26.4138854410428));
#28597=CARTESIAN_POINT('Ctrl Pts',(4.62834401390971,-1.66443169034465,26.4189498397435));
#28598=CARTESIAN_POINT('Ctrl Pts',(4.64572764167704,-1.61527580757656,26.4218892312632));
#28599=CARTESIAN_POINT('Ctrl Pts',(4.71423170970352,-1.41130490566337,26.4339958058489));
#28600=CARTESIAN_POINT('Ctrl Pts',(4.75842065735715,-1.25427101848321,26.4431067195492));
#28601=CARTESIAN_POINT('Ctrl Pts',(4.81481354507434,-1.00741564395819,26.4573007741237));
#28602=CARTESIAN_POINT('Ctrl Pts',(4.83247565071357,-0.918963898365818,
26.4623610283136));
#28603=CARTESIAN_POINT('Ctrl Pts',(4.8609006102615,-0.752960594551082,26.4718384525242));
#28604=CARTESIAN_POINT('Ctrl Pts',(4.87226325181618,-0.675540531863483,
26.4762506224585));
#28605=CARTESIAN_POINT('Ctrl Pts',(4.89011642676261,-0.529767593658105,
26.4845567575378));
#28606=CARTESIAN_POINT('Ctrl Pts',(4.89703209295423,-0.461485545991866,
26.4884468296596));
#28607=CARTESIAN_POINT('Ctrl Pts',(4.91200254672783,-0.274773983746103,
26.4990905819884));
#28608=CARTESIAN_POINT('Ctrl Pts',(4.91720269088325,-0.156162962670973,
26.5058602653956));
#28609=CARTESIAN_POINT('Ctrl Pts',(4.91914573379363,0.0987920828655218,
26.5204390560551));
#28610=CARTESIAN_POINT('Ctrl Pts',(4.9145199352676,0.235049807511419,26.528247709637));
#28611=CARTESIAN_POINT('Ctrl Pts',(4.90017711414828,0.424678402147387,26.5391168377062));
#28612=CARTESIAN_POINT('Ctrl Pts',(4.89522942812055,0.478347583147858,26.5421929967283));
#28613=CARTESIAN_POINT('Ctrl Pts',(4.88467037024237,0.575405393523894,26.5477523830584));
#28614=CARTESIAN_POINT('Ctrl Pts',(4.87936024028821,0.61882121655799,26.5502378518366));
#28615=CARTESIAN_POINT('Ctrl Pts',(4.86793498053317,0.702910586215343,26.5550466184873));
#28616=CARTESIAN_POINT('Ctrl Pts',(4.86188736587435,0.743589639034716,26.5573703689379));
#28617=CARTESIAN_POINT('Ctrl Pts',(4.83143540358408,0.932134065475232,26.5681403476853));
#28618=CARTESIAN_POINT('Ctrl Pts',(4.80079073392387,1.07891211142336,26.5765256467456));
#28619=CARTESIAN_POINT('Ctrl Pts',(4.72693526481078,1.36632375563199,26.5931501917273));
#28620=CARTESIAN_POINT('Ctrl Pts',(4.68402463959099,1.50687427726627,26.6013807250745));
#28621=CARTESIAN_POINT('Ctrl Pts',(4.61052791486324,1.71391904922801,26.6137579780051));
#28622=CARTESIAN_POINT('Ctrl Pts',(4.58464580641479,1.78199574295386,26.6178693593295));
#28623=CARTESIAN_POINT('Ctrl Pts',(4.53331723578677,1.90847385561338,26.6255964773817));
#28624=CARTESIAN_POINT('Ctrl Pts',(4.50822918027319,1.9670046169679,26.629208851209));
#28625=CARTESIAN_POINT('Ctrl Pts',(4.41576030385953,2.17166644270623,26.6419776718008));
#28626=CARTESIAN_POINT('Ctrl Pts',(4.34235331671887,2.31496017985609,26.6511724253238));
#28627=CARTESIAN_POINT('Ctrl Pts',(4.21167834579522,2.54187716135869,26.6661615330596));
#28628=CARTESIAN_POINT('Ctrl Pts',(4.15861871017481,2.62778700683347,26.6719418772543));
#28629=CARTESIAN_POINT('Ctrl Pts',(4.06767856992004,2.76536910764251,26.6813601378892));
#28630=CARTESIAN_POINT('Ctrl Pts',(4.03136622085359,2.81804219039155,26.6850061787983));
#28631=CARTESIAN_POINT('Ctrl Pts',(3.97235678848928,2.90016290534226,26.6907493160788));
#28632=CARTESIAN_POINT('Ctrl Pts',(3.95033592998315,2.93008693012193,26.6928544350659));
#28633=CARTESIAN_POINT('Ctrl Pts',(3.89257787131946,3.00673924381634,26.6982798803932));
#28634=CARTESIAN_POINT('Ctrl Pts',(3.85633758185636,3.05308105731361,26.70159325527));
#28635=CARTESIAN_POINT('Ctrl Pts',(3.70678678051953,3.23740484613984,26.7149364741965));
#28636=CARTESIAN_POINT('Ctrl Pts',(3.58683284525733,3.3698203452651,26.7249072239713));
#28637=CARTESIAN_POINT('Ctrl Pts',(3.40327167194179,3.5515185244322,26.7393977259043));
#28638=CARTESIAN_POINT('Ctrl Pts',(3.34524290805063,3.60622955867942,26.7438777186817));
#28639=CARTESIAN_POINT('Ctrl Pts',(3.23139855942059,3.70845165417342,26.752496386426));
#28640=CARTESIAN_POINT('Ctrl Pts',(3.17580067471761,3.75617361557201,26.7566321014895));
#28641=CARTESIAN_POINT('Ctrl Pts',(3.07013305238742,3.84284876891761,26.7643682024507));
#28642=CARTESIAN_POINT('Ctrl Pts',(3.02033536837647,3.88210996381428,26.7679650237071));
#28643=CARTESIAN_POINT('Ctrl Pts',(2.86426643508893,4.00033584702172,26.7790958408212));
#28644=CARTESIAN_POINT('Ctrl Pts',(2.75555660580643,4.07598038924907,26.7866531499899));
#28645=CARTESIAN_POINT('Ctrl Pts',(2.51700580286307,4.22806362256582,26.802839336601));
#28646=CARTESIAN_POINT('Ctrl Pts',(2.38643430220917,4.30311188126951,26.8114653101268));
#28647=CARTESIAN_POINT('Ctrl Pts',(2.20574939255053,4.39620671937522,26.8230577787829));
#28648=CARTESIAN_POINT('Ctrl Pts',(2.15848624081726,4.41960418392969,26.8260592723019));
#28649=CARTESIAN_POINT('Ctrl Pts',(2.07684420374067,4.45839872436785,26.8311878713766));
#28650=CARTESIAN_POINT('Ctrl Pts',(2.04264841659635,4.47416902981631,26.8333189737312));
#28651=CARTESIAN_POINT('Ctrl Pts',(1.9557553649703,4.51303824362907,26.8386945536448));
#28652=CARTESIAN_POINT('Ctrl Pts',(1.90282765404571,4.53560803664727,26.8419329612138));
#28653=CARTESIAN_POINT('Ctrl Pts',(1.69357365133645,4.62053185482621,26.8546215721765));
#28654=CARTESIAN_POINT('Ctrl Pts',(1.53448539735802,4.67577387874527,26.8640236731188));
#28655=CARTESIAN_POINT('Ctrl Pts',(1.29536194768947,4.74528577345838,26.8779932710233));
#28656=CARTESIAN_POINT('Ctrl Pts',(1.21730286033883,4.76590738805358,26.8825278833075));
#28657=CARTESIAN_POINT('Ctrl Pts',(1.06704415092572,4.80167014653708,26.8912274125101));
#28658=CARTESIAN_POINT('Ctrl Pts',(0.994941911260006,4.81712672050747,26.8953891865255));
#28659=CARTESIAN_POINT('Ctrl Pts',(0.860488589443576,4.84280194404223,26.9031366822528));
#28660=CARTESIAN_POINT('Ctrl Pts',(0.798235177612503,4.85345153192027,26.9067186302735));
#28661=CARTESIAN_POINT('Ctrl Pts',(0.614608929264103,4.88123560884879,26.9172754554385));
#28662=CARTESIAN_POINT('Ctrl Pts',(0.492781691930183,4.89503532013962,26.9242692969759));
#28663=CARTESIAN_POINT('Ctrl Pts',(0.189299844147326,4.91796647922178,26.9416768905423));
#28664=CARTESIAN_POINT('Ctrl Pts',(0.00741124822885696,4.92160283021055,
26.9521002709487));
#28665=CARTESIAN_POINT('Ctrl Pts',(-0.217658076684673,4.913623276149,26.9649235858452));
#28666=CARTESIAN_POINT('Ctrl Pts',(-0.261033246241738,4.91150999605861,
26.9673911142584));
#28667=CARTESIAN_POINT('Ctrl Pts',(-0.340050833136463,4.90661045407957,
26.9718770381134));
#28668=CARTESIAN_POINT('Ctrl Pts',(-0.375701643491329,4.90400948423775,
26.9738974383605));
#28669=CARTESIAN_POINT('Ctrl Pts',(-0.491658626285695,4.89427772315574,
26.9804626746688));
#28670=CARTESIAN_POINT('Ctrl Pts',(-0.571818979186006,4.8855609641989,26.9849915547972));
#28671=CARTESIAN_POINT('Ctrl Pts',(-0.801651984965655,4.85483425670535,
26.9979981257927));
#28672=CARTESIAN_POINT('Ctrl Pts',(-0.950569965781884,4.8278854908312,27.0064540580447));
#28673=CARTESIAN_POINT('Ctrl Pts',(-1.14467393831461,4.78342936621185,27.0176311561061));
#28674=CARTESIAN_POINT('Ctrl Pts',(-1.19118034920191,4.77206079887855,27.0203208314883));
#28675=CARTESIAN_POINT('Ctrl Pts',(-1.31421137649138,4.74007507728931,27.0274730647507));
#28676=CARTESIAN_POINT('Ctrl Pts',(-1.39041576096083,4.71828433768648,27.0319413595728));
#28677=CARTESIAN_POINT('Ctrl Pts',(-1.53203342596999,4.67405965262473,27.040331209171));
#28678=CARTESIAN_POINT('Ctrl Pts',(-1.59756500433706,4.65206899845181,27.0442486564887));
#28679=CARTESIAN_POINT('Ctrl Pts',(-1.7751779802153,4.58827118192,27.0549716373847));
#28680=CARTESIAN_POINT('Ctrl Pts',(-1.88623141693507,4.5437451225111,27.0617934797819));
#28681=CARTESIAN_POINT('Ctrl Pts',(-2.12047679604748,4.43975715565054,27.0764478925027));
#28682=CARTESIAN_POINT('Ctrl Pts',(-2.24303742141698,4.37911504145828,27.0842798403112));
#28683=CARTESIAN_POINT('Ctrl Pts',(-2.41023352067622,4.28752477156363,27.0951758467351));
#28684=CARTESIAN_POINT('Ctrl Pts',(-2.45712482674021,4.26082526582539,27.0982556273639));
#28685=CARTESIAN_POINT('Ctrl Pts',(-2.54124283435571,4.21107869534848,27.1038205485562));
#28686=CARTESIAN_POINT('Ctrl Pts',(-2.57861928832987,4.18829578077866,27.1063079375272));
#28687=CARTESIAN_POINT('Ctrl Pts',(-2.65049120055705,4.14315924749024,27.1111171747242));
#28688=CARTESIAN_POINT('Ctrl Pts',(-2.68502037060214,4.12086614758497,27.1134394906808));
#28689=CARTESIAN_POINT('Ctrl Pts',(-2.80913679515193,4.03851040077335,27.1218392195867));
#28690=CARTESIAN_POINT('Ctrl Pts',(-2.8970223957585,3.97593731245132,27.1278873569205));
#28691=CARTESIAN_POINT('Ctrl Pts',(-2.99065558434452,3.90451793965808,27.134486478428));
#28692=CARTESIAN_POINT('Ctrl Pts',(-2.99851268673053,3.89848724929369,27.1350414598712));
#28693=CARTESIAN_POINT('Ctrl Pts',(-3.14411574666091,3.78602956644793,27.1453493582073));
#28694=CARTESIAN_POINT('Ctrl Pts',(-3.27613278389825,3.67238844288121,27.1550890698183));
#28695=CARTESIAN_POINT('Ctrl Pts',(-3.45534262376687,3.50075382597196,27.1690642405637));
#28696=CARTESIAN_POINT('Ctrl Pts',(-3.50767444370431,3.44831695537903,27.1732449953358));
#28697=CARTESIAN_POINT('Ctrl Pts',(-3.60811517231498,3.3430214468718,27.181480680634));
#28698=CARTESIAN_POINT('Ctrl Pts',(-3.65629604267182,3.29025630919129,27.1855338221875));
#28699=CARTESIAN_POINT('Ctrl Pts',(-3.82946513058828,3.0921081296754,27.2004996309676));
#28700=CARTESIAN_POINT('Ctrl Pts',(-3.94707078820502,2.94050442093864,27.2114682040348));
#28701=CARTESIAN_POINT('Ctrl Pts',(-4.10059238470354,2.71673904660358,27.227001027709));
#28702=CARTESIAN_POINT('Ctrl Pts',(-4.14405712253853,2.64996597019552,27.2315581508474));
#28703=CARTESIAN_POINT('Ctrl Pts',(-4.20005209579265,2.55919401502383,27.2376435628737));
#28704=CARTESIAN_POINT('Ctrl Pts',(-4.21403390123245,2.53610526270841,27.2391821707683));
#28705=CARTESIAN_POINT('Ctrl Pts',(-4.24973472362664,2.47604052547092,27.243160224577));
#28706=CARTESIAN_POINT('Ctrl Pts',(-4.27116161117316,2.43889328452574,27.2455966174518));
#28707=CARTESIAN_POINT('Ctrl Pts',(-4.31252859415273,2.36495889888351,27.2503965622793));
#28708=CARTESIAN_POINT('Ctrl Pts',(-4.33249050729194,2.32818803435896,27.2527601703785));
#28709=CARTESIAN_POINT('Ctrl Pts',(-4.41608745863257,2.16939891621032,27.2628775788631));
#28710=CARTESIAN_POINT('Ctrl Pts',(-4.47505587469502,2.04499287394127,27.2705816853467));
#28711=CARTESIAN_POINT('Ctrl Pts',(-4.59136235872545,1.77041276027475,27.2872868489375));
#28712=CARTESIAN_POINT('Ctrl Pts',(-4.64671467407092,1.61957140937564,27.2962808524593));
#28713=CARTESIAN_POINT('Ctrl Pts',(-4.71606775494272,1.39752583687116,27.309388817397));
#28714=CARTESIAN_POINT('Ctrl Pts',(-4.73603295104073,1.32829411728723,27.313457166485));
#28715=CARTESIAN_POINT('Ctrl Pts',(-4.75770540297722,1.24642777435912,27.3182521627716));
#28716=CARTESIAN_POINT('Ctrl Pts',(-4.76089362727495,1.23419397003609,27.3189682926657));
#28717=CARTESIAN_POINT('Ctrl Pts',(-4.76403458719828,1.22194824541733,27.3196847251172));
#28718=CARTESIAN_POINT('Origin',(0.,0.,-3.23514056400928));
#28719=CARTESIAN_POINT('',(-4.76403458343061,1.22194826010642,29.4150832822139));
#28720=CARTESIAN_POINT('',(-4.76403458843593,1.2219482405921,29.0701077704777));
#28721=CARTESIAN_POINT('',(-4.76403458704967,1.22194824599672,-3.23514056400928));
#28722=CARTESIAN_POINT('Ctrl Pts',(-4.76403458343061,1.22194826010642,29.4150832822139));
#28723=CARTESIAN_POINT('Ctrl Pts',(-4.75082584336757,1.27344544416756,29.4121019759593));
#28724=CARTESIAN_POINT('Ctrl Pts',(-4.73678161207201,1.32473039678181,29.4091233894005));
#28725=CARTESIAN_POINT('Ctrl Pts',(-4.68989367983414,1.48565729250495,29.3997331065548));
#28726=CARTESIAN_POINT('Ctrl Pts',(-4.65405535264088,1.59438040222996,29.3933236026385));
#28727=CARTESIAN_POINT('Ctrl Pts',(-4.5842473291198,1.78367109953656,29.3819867965666));
#28728=CARTESIAN_POINT('Ctrl Pts',(-4.55186153069621,1.86476875787112,29.3770706029348));
#28729=CARTESIAN_POINT('Ctrl Pts',(-4.49658445658056,1.99315440738091,29.3691746899046));
#28730=CARTESIAN_POINT('Ctrl Pts',(-4.47506460434152,2.04101273644553,29.3662056059117));
#28731=CARTESIAN_POINT('Ctrl Pts',(-4.41840090257451,2.16182149582261,29.3586406872943));
#28732=CARTESIAN_POINT('Ctrl Pts',(-4.38221394979193,2.23426484378479,29.3540381212687));
#28733=CARTESIAN_POINT('Ctrl Pts',(-4.25402715683615,2.47577786470135,29.3384558359654));
#28734=CARTESIAN_POINT('Ctrl Pts',(-4.15389876209381,2.64033084521303,29.3274286720098));
#28735=CARTESIAN_POINT('Ctrl Pts',(-4.00976788111575,2.84862181633944,29.3129425178816));
#28736=CARTESIAN_POINT('Ctrl Pts',(-3.97422233823533,2.89800648793335,29.3094669669052));
#28737=CARTESIAN_POINT('Ctrl Pts',(-3.91546259315499,2.97652850453381,29.303878226607));
#28738=CARTESIAN_POINT('Ctrl Pts',(-3.89281773616238,3.00608372522347,29.3017599355913));
#28739=CARTESIAN_POINT('Ctrl Pts',(-3.85979261480422,3.04818782764127,29.2987220076966));
#28740=CARTESIAN_POINT('Ctrl Pts',(-3.84968231971051,3.06094660238635,29.2977987136193));
#28741=CARTESIAN_POINT('Ctrl Pts',(-3.81364002311545,3.10596945523011,29.2945312207628));
#28742=CARTESIAN_POINT('Ctrl Pts',(-3.7873641024971,3.1379562913966,29.2921926494902));
#28743=CARTESIAN_POINT('Ctrl Pts',(-3.65545957550888,3.29445883444423,29.2806525508195));
#28744=CARTESIAN_POINT('Ctrl Pts',(-3.54407850142492,3.41399363134801,29.2715230835065));
#28745=CARTESIAN_POINT('Ctrl Pts',(-3.35529150774579,3.5973858078391,29.2567757000638));
#28746=CARTESIAN_POINT('Ctrl Pts',(-3.2815211618636,3.66480346020288,29.2511743138697));
#28747=CARTESIAN_POINT('Ctrl Pts',(-3.14452200048387,3.78254971726782,29.2410160553056));
#28748=CARTESIAN_POINT('Ctrl Pts',(-3.08200894919188,3.83365642771109,29.2364667532505));
#28749=CARTESIAN_POINT('Ctrl Pts',(-2.96738571182935,3.92274878474073,29.2282618180793));
#28750=CARTESIAN_POINT('Ctrl Pts',(-2.9157326205245,3.96129261211287,29.2246119273679));
#28751=CARTESIAN_POINT('Ctrl Pts',(-2.78609656380595,4.05411817099791,29.2155605683656));
#28752=CARTESIAN_POINT('Ctrl Pts',(-2.70727015443826,4.10717618130111,29.2101508682175));
#28753=CARTESIAN_POINT('Ctrl Pts',(-2.48719807153855,4.24621693888233,29.1952893204701));
#28754=CARTESIAN_POINT('Ctrl Pts',(-2.3430759033633,4.32741347774685,29.1858158160558));
#28755=CARTESIAN_POINT('Ctrl Pts',(-2.14345300429715,4.42697734971275,29.1730611964079));
#28756=CARTESIAN_POINT('Ctrl Pts',(-2.09131518082595,4.45184457596452,29.1697627445903));
#28757=CARTESIAN_POINT('Ctrl Pts',(-1.997716071379,4.49447959439262,29.1639034027648));
#28758=CARTESIAN_POINT('Ctrl Pts',(-1.95642550501508,4.51260630152774,29.161339700742));
#28759=CARTESIAN_POINT('Ctrl Pts',(-1.89493118927968,4.53859983222549,29.1575547135367));
#28760=CARTESIAN_POINT('Ctrl Pts',(-1.87491566104948,4.54690487237889,29.1563279768096));
#28761=CARTESIAN_POINT('Ctrl Pts',(-1.80349534186036,4.57598751204332,29.1519682444504));
#28762=CARTESIAN_POINT('Ctrl Pts',(-1.75179456962918,4.59602796441462,29.1488442631436));
#28763=CARTESIAN_POINT('Ctrl Pts',(-1.54469427979363,4.6723026010606,29.136433634258));
#28764=CARTESIAN_POINT('Ctrl Pts',(-1.38684215392434,4.72156346145487,29.1271998802425));
#28765=CARTESIAN_POINT('Ctrl Pts',(-1.14372278208686,4.78418673568879,29.1131227926476));
#28766=CARTESIAN_POINT('Ctrl Pts',(-1.06009065201677,4.80341047135995,29.1083063374818));
#28767=CARTESIAN_POINT('Ctrl Pts',(-0.948245608302949,4.82605585951622,
29.1018826139212));
#28768=CARTESIAN_POINT('Ctrl Pts',(-0.920444222794154,4.83143532676495,
29.1002873237115));
#28769=CARTESIAN_POINT('Ctrl Pts',(-0.834829466712585,4.84723567528032,
29.0953779563197));
#28770=CARTESIAN_POINT('Ctrl Pts',(-0.776874931367547,4.85686104231159,
29.0920593253163));
#28771=CARTESIAN_POINT('Ctrl Pts',(-0.647467285981693,4.87597816647436,
29.0846534864372));
#28772=CARTESIAN_POINT('Ctrl Pts',(-0.575950000280785,4.88494200591665,
29.0805635427757));
#28773=CARTESIAN_POINT('Ctrl Pts',(-0.320595731570073,4.91126187245817,
29.0659594553486));
#28774=CARTESIAN_POINT('Ctrl Pts',(-0.136010932940788,4.91983477811692,
29.0553953648375));
#28775=CARTESIAN_POINT('Ctrl Pts',(0.128969922322148,4.9172154037837,29.0402273090635));
#28776=CARTESIAN_POINT('Ctrl Pts',(0.209293466004387,4.91445184518138,29.035630124057));
#28777=CARTESIAN_POINT('Ctrl Pts',(0.331999682883111,4.90721617874198,29.0286163117156));
#28778=CARTESIAN_POINT('Ctrl Pts',(0.374451813036639,4.90415948940137,29.0261914875896));
#28779=CARTESIAN_POINT('Ctrl Pts',(0.444122588101571,4.89823303472761,29.0222165631893));
#28780=CARTESIAN_POINT('Ctrl Pts',(0.471366341021327,4.89568642010676,29.0206633895326));
#28781=CARTESIAN_POINT('Ctrl Pts',(0.533789692564847,4.8893254835398,29.0171080507327));
#28782=CARTESIAN_POINT('Ctrl Pts',(0.568952290553136,4.8853585783892,29.015107954135));
#28783=CARTESIAN_POINT('Ctrl Pts',(0.682748953676971,4.87127521771701,29.0086383936479));
#28784=CARTESIAN_POINT('Ctrl Pts',(0.761182511036733,4.85963679702101,29.0041843237681));
#28785=CARTESIAN_POINT('Ctrl Pts',(0.879189315227419,4.83919910814305,28.9974659577898));
#28786=CARTESIAN_POINT('Ctrl Pts',(0.918990840490816,4.83179859963066,28.9951970610114));
#28787=CARTESIAN_POINT('Ctrl Pts',(1.11574588411971,4.79269578224991,28.9839568545066));
#28788=CARTESIAN_POINT('Ctrl Pts',(1.2711762602996,4.75383341187199,28.9749977294899));
#28789=CARTESIAN_POINT('Ctrl Pts',(1.49978563207011,4.68465837064174,28.9615593314483));
#28790=CARTESIAN_POINT('Ctrl Pts',(1.57457944470942,4.6600515412891,28.9571204311089));
#28791=CARTESIAN_POINT('Ctrl Pts',(1.71315975420425,4.61074187319669,28.9488026946925));
#28792=CARTESIAN_POINT('Ctrl Pts',(1.77708439254845,4.58648317189403,28.9449279747287));
#28793=CARTESIAN_POINT('Ctrl Pts',(1.94791002130315,4.5175490791475,28.9344623280718));
#28794=CARTESIAN_POINT('Ctrl Pts',(2.05377163748794,4.47041660688822,28.9278564696221));
#28795=CARTESIAN_POINT('Ctrl Pts',(2.28381650759807,4.35809700366819,28.9132212837328));
#28796=CARTESIAN_POINT('Ctrl Pts',(2.40707758460842,4.29124746150916,28.9051901541277));
#28797=CARTESIAN_POINT('Ctrl Pts',(2.57392232021584,4.19130750527635,28.8940737030792));
#28798=CARTESIAN_POINT('Ctrl Pts',(2.62006419385679,4.16261917593578,28.8909724060079));
#28799=CARTESIAN_POINT('Ctrl Pts',(2.70259286869878,4.10939166475372,28.8853798551658));
#28800=CARTESIAN_POINT('Ctrl Pts',(2.73914463873038,4.08511869793034,28.8828863050773));
#28801=CARTESIAN_POINT('Ctrl Pts',(2.80419498356768,4.04065500701107,28.8784208550286));
#28802=CARTESIAN_POINT('Ctrl Pts',(2.83281234032829,4.0206438116517,28.8764466805228));
#28803=CARTESIAN_POINT('Ctrl Pts',(2.92273426468888,3.95632763152877,28.8702077623125));
#28804=CARTESIAN_POINT('Ctrl Pts',(2.98323148779616,3.91091217116087,28.865956981962));
#28805=CARTESIAN_POINT('Ctrl Pts',(3.19073765697843,3.74751911508068,28.8511373988682));
#28806=CARTESIAN_POINT('Ctrl Pts',(3.33199236294721,3.62250370720793,28.8406103638568));
#28807=CARTESIAN_POINT('Ctrl Pts',(3.49433961987341,3.4612714790846,28.8277491265928));
#28808=CARTESIAN_POINT('Ctrl Pts',(3.52260509811511,3.43250097306734,28.8254798459358));
#28809=CARTESIAN_POINT('Ctrl Pts',(3.60038496075583,3.35135871342138,28.8191472682971));
#28810=CARTESIAN_POINT('Ctrl Pts',(3.64910650179652,3.29824175468706,28.8150782253401));
#28811=CARTESIAN_POINT('Ctrl Pts',(3.73824307419844,3.19667006027388,28.8074279991796));
#28812=CARTESIAN_POINT('Ctrl Pts',(3.77892734082992,3.14847086682724,28.8038500848095));
#28813=CARTESIAN_POINT('Ctrl Pts',(3.90291797670219,2.99571098362214,28.7926642794351));
#28814=CARTESIAN_POINT('Ctrl Pts',(3.98289523673599,2.88852865508529,28.7850324642389));
#28815=CARTESIAN_POINT('Ctrl Pts',(4.12587220363088,2.6796690481053,28.7705504119382));
#28816=CARTESIAN_POINT('Ctrl Pts',(4.18972615988816,2.57869006361858,28.7637086143219));
#28817=CARTESIAN_POINT('Ctrl Pts',(4.27547465437232,2.43147964609988,28.7539747655522));
#28818=CARTESIAN_POINT('Ctrl Pts',(4.30042347123166,2.38707662618484,28.7510688997632));
#28819=CARTESIAN_POINT('Ctrl Pts',(4.34470492693294,2.30531786396045,28.7457760470853));
#28820=CARTESIAN_POINT('Ctrl Pts',(4.36425667661212,2.26808621327702,28.7433871316244));
#28821=CARTESIAN_POINT('Ctrl Pts',(4.40224367665935,2.19343862986354,28.7386420950249));
#28822=CARTESIAN_POINT('Ctrl Pts',(4.42068526302609,2.15602974686191,28.7362860852714));
#28823=CARTESIAN_POINT('Ctrl Pts',(4.49702822495673,1.9960688725973,28.7262933768309));
#28824=CARTESIAN_POINT('Ctrl Pts',(4.55032673259614,1.87138484245546,28.7187045513967));
#28825=CARTESIAN_POINT('Ctrl Pts',(4.65613028612378,1.59251760921237,28.7019953268884));
#28826=CARTESIAN_POINT('Ctrl Pts',(4.70626642038934,1.43760811619959,28.6928819578242));
#28827=CARTESIAN_POINT('Ctrl Pts',(4.76720336013819,1.21162842505632,28.6796929239233));
#28828=CARTESIAN_POINT('Ctrl Pts',(4.78427446455127,1.14236115624937,28.6756647116931));
#28829=CARTESIAN_POINT('Ctrl Pts',(4.81566182351191,1.00192358554424,28.667516885903));
#28830=CARTESIAN_POINT('Ctrl Pts',(4.82992114587517,0.930758415957353,28.6633978956885));
#28831=CARTESIAN_POINT('Ctrl Pts',(4.87211086684007,0.692998708541581,28.649658617036));
#28832=CARTESIAN_POINT('Ctrl Pts',(4.89303442400027,0.525285032389969,28.6399989006004));
#28833=CARTESIAN_POINT('Ctrl Pts',(4.91438654770056,0.23176079275549,28.6231518094096));
#28834=CARTESIAN_POINT('Ctrl Pts',(4.91869803143934,0.106388047788207,28.615975747272));
#28835=CARTESIAN_POINT('Ctrl Pts',(4.91805402182035,-0.0602012732167473,
28.6064947129578));
#28836=CARTESIAN_POINT('Ctrl Pts',(4.91737739574035,-0.101386193032589,
28.6041553037917));
#28837=CARTESIAN_POINT('Ctrl Pts',(4.91494826580533,-0.185155898626823,
28.5994084498092));
#28838=CARTESIAN_POINT('Ctrl Pts',(4.91315941543167,-0.227736201860754,
28.5970015557087));
#28839=CARTESIAN_POINT('Ctrl Pts',(4.90404400537677,-0.39335244500484,28.5876524074803));
#28840=CARTESIAN_POINT('Ctrl Pts',(4.89264699589848,-0.516119898883973,
28.5807479683299));
#28841=CARTESIAN_POINT('Ctrl Pts',(4.86121339365576,-0.756263048734239,
28.5671794639173));
#28842=CARTESIAN_POINT('Ctrl Pts',(4.84150376345247,-0.873596328068323,
28.5605199581225));
#28843=CARTESIAN_POINT('Ctrl Pts',(4.79940138535841,-1.07845537266142,28.5487701412546));
#28844=CARTESIAN_POINT('Ctrl Pts',(4.77881536090128,-1.16629461163767,28.5436919260915));
#28845=CARTESIAN_POINT('Ctrl Pts',(4.73868641570457,-1.31854323022843,28.5347984421455));
#28846=CARTESIAN_POINT('Ctrl Pts',(4.72021547604169,-1.3832103681458,28.5309916830454));
#28847=CARTESIAN_POINT('Ctrl Pts',(4.67344532373865,-1.53508803583103,28.5219736806671));
#28848=CARTESIAN_POINT('Ctrl Pts',(4.6440222416752,-1.62192588725829,28.5167560722468));
#28849=CARTESIAN_POINT('Ctrl Pts',(4.58912224889926,-1.77018438931629,28.5077341915746));
#28850=CARTESIAN_POINT('Ctrl Pts',(4.56479503071419,-1.8320049237038,28.5039373566651));
#28851=CARTESIAN_POINT('Ctrl Pts',(4.48504799691656,-2.02319861718643,28.4920855497587));
#28852=CARTESIAN_POINT('Ctrl Pts',(4.42532283772658,-2.15069899606934,28.484021710605));
#28853=CARTESIAN_POINT('Ctrl Pts',(4.3331186173798,-2.32737954618943,28.4726467235227));
#28854=CARTESIAN_POINT('Ctrl Pts',(4.30509942384662,-2.37880885568943,28.4693108595645));
#28855=CARTESIAN_POINT('Ctrl Pts',(4.25800538593239,-2.46169146782939,28.4638988307489));
#28856=CARTESIAN_POINT('Ctrl Pts',(4.23948465038511,-2.49345236290626,28.4618164869513));
#28857=CARTESIAN_POINT('Ctrl Pts',(4.18864551776687,-2.57843131621966,28.4562204857773));
#28858=CARTESIAN_POINT('Ctrl Pts',(4.15566981960058,-2.63124833810635,28.4527151949306));
#28859=CARTESIAN_POINT('Ctrl Pts',(4.02684667137273,-2.82911869896542,28.4394477574002));
#28860=CARTESIAN_POINT('Ctrl Pts',(3.92433486848256,-2.96968063394021,28.4297369522528));
#28861=CARTESIAN_POINT('Ctrl Pts',(3.76484475588937,-3.16564987382452,28.4155602963498));
#28862=CARTESIAN_POINT('Ctrl Pts',(3.71363169563772,-3.22557508585818,28.4111319328015));
#28863=CARTESIAN_POINT('Ctrl Pts',(3.61256757647745,-3.33823295370424,28.402606133697));
#28864=CARTESIAN_POINT('Ctrl Pts',(3.56294609548388,-3.39114415914643,28.3985115485807));
#28865=CARTESIAN_POINT('Ctrl Pts',(3.46821995864917,-3.48777516600229,28.3908519508957));
#28866=CARTESIAN_POINT('Ctrl Pts',(3.42341261555455,-3.53176602362439,28.3872904166371));
#28867=CARTESIAN_POINT('Ctrl Pts',(3.28739847880043,-3.66028065542001,28.3766528290028));
#28868=CARTESIAN_POINT('Ctrl Pts',(3.19381649631292,-3.74221575795378,28.3695570047693));
#28869=CARTESIAN_POINT('Ctrl Pts',(2.97791420174895,-3.91724432883539,28.3536589291943));
#28870=CARTESIAN_POINT('Ctrl Pts',(2.85413078134223,-4.00833055703138,28.3448557107084));
#28871=CARTESIAN_POINT('Ctrl Pts',(2.70404869273423,-4.10828646808451,28.3345674504822));
#28872=CARTESIAN_POINT('Ctrl Pts',(2.68168889447427,-4.1229166520633,28.3330443747271));
#28873=CARTESIAN_POINT('Ctrl Pts',(2.62345898189416,-4.16034280572474,28.3291036352203));
#28874=CARTESIAN_POINT('Ctrl Pts',(2.58741042650245,-4.18285747201517,28.3266889765835));
#28875=CARTESIAN_POINT('Ctrl Pts',(2.51577288142438,-4.22631929151112,28.321941617306));
#28876=CARTESIAN_POINT('Ctrl Pts',(2.48020287929744,-4.24729109786057,28.3196088159887));
#28877=CARTESIAN_POINT('Ctrl Pts',(2.32000592830706,-4.33904326669952,28.3091996452963));
#28878=CARTESIAN_POINT('Ctrl Pts',(2.19258353294268,-4.40480446241282,28.3011779419278));
#28879=CARTESIAN_POINT('Ctrl Pts',(1.92174134904492,-4.52991432187993,28.2844642346539));
#28880=CARTESIAN_POINT('Ctrl Pts',(1.77801908751773,-4.58823069536822,28.2757796773237));
#28881=CARTESIAN_POINT('Ctrl Pts',(1.56428110258131,-4.66340305399406,28.2630129381502));
#28882=CARTESIAN_POINT('Ctrl Pts',(1.49626818032756,-4.68566801954334,28.2589722982437));
#28883=CARTESIAN_POINT('Ctrl Pts',(1.35859224421439,-4.72743480499193,28.2508266400555));
#28884=CARTESIAN_POINT('Ctrl Pts',(1.28893619601291,-4.746899623988,28.2467223836671));
#28885=CARTESIAN_POINT('Ctrl Pts',(1.05730812633487,-4.80615181408327,28.2331198366327));
#28886=CARTESIAN_POINT('Ctrl Pts',(0.893743505257881,-4.83923723718358,
28.223583210395));
#28887=CARTESIAN_POINT('Ctrl Pts',(0.639430687359732,-4.87734361969033,
28.2088625556191));
#28888=CARTESIAN_POINT('Ctrl Pts',(0.549691649591653,-4.88827082062962,
28.2036892891148));
#28889=CARTESIAN_POINT('Ctrl Pts',(0.399903521268695,-4.90233287734534,
28.1951008670836));
#28890=CARTESIAN_POINT('Ctrl Pts',(0.340006440079352,-4.9068509464964,28.1916789501077));
#28891=CARTESIAN_POINT('Ctrl Pts',(0.243352693047611,-4.91236327573058,
28.1861820595237));
#28892=CARTESIAN_POINT('Ctrl Pts',(0.206641871403309,-4.91404443027282,
28.1841003788821));
#28893=CARTESIAN_POINT('Ctrl Pts',(0.109335115299174,-4.91740818138489,
28.1785975410169));
#28894=CARTESIAN_POINT('Ctrl Pts',(0.0487209742579251,-4.91838223281956,
28.175184110936));
#28895=CARTESIAN_POINT('Ctrl Pts',(-0.187692170263738,-4.91781039979649,
28.1618972305394));
#28896=CARTESIAN_POINT('Ctrl Pts',(-0.363339583257405,-4.90796010438973,
28.1520783582331));
#28897=CARTESIAN_POINT('Ctrl Pts',(-0.616677363874846,-4.88007623812464,
28.1377786726159));
#28898=CARTESIAN_POINT('Ctrl Pts',(-0.695051742352843,-4.86953159773891,
28.1333362667401));
#28899=CARTESIAN_POINT('Ctrl Pts',(-0.844885963560833,-4.84568148718336,
28.1247896521021));
#28900=CARTESIAN_POINT('Ctrl Pts',(-0.916372183786456,-4.83267247249283,
28.1206883399193));
#28901=CARTESIAN_POINT('Ctrl Pts',(-1.04898444224154,-4.80549147280676,
28.1130259636676));
#28902=CARTESIAN_POINT('Ctrl Pts',(-1.11017852766317,-4.79172413481118,
28.109468431861));
#28903=CARTESIAN_POINT('Ctrl Pts',(-1.29047034106932,-4.74752325757581,
28.0989160919381));
#28904=CARTESIAN_POINT('Ctrl Pts',(-1.40870815750662,-4.71379162498846,
28.0919021062682));
#28905=CARTESIAN_POINT('Ctrl Pts',(-1.66886780773246,-4.62890783711941,
28.0762496413292));
#28906=CARTESIAN_POINT('Ctrl Pts',(-1.80995355126799,-4.57558475579388,
28.0676102402097));
#28907=CARTESIAN_POINT('Ctrl Pts',(-2.00168774356557,-4.49286117612384,
28.0556922182234));
#28908=CARTESIAN_POINT('Ctrl Pts',(-2.05459707093001,-4.46891333115277,
28.0523844514683));
#28909=CARTESIAN_POINT('Ctrl Pts',(-2.14030123789195,-4.42827801956524,
28.0469997925566));
#28910=CARTESIAN_POINT('Ctrl Pts',(-2.17335440202981,-4.41214984870694,
28.0449168938041));
#28911=CARTESIAN_POINT('Ctrl Pts',(-2.26239313806218,-4.36746037239851,
28.0392872755184));
#28912=CARTESIAN_POINT('Ctrl Pts',(-2.31801726630154,-4.3381941994672,28.0357491525871));
#28913=CARTESIAN_POINT('Ctrl Pts',(-2.46725521424797,-4.2559838569226,28.0261756144991));
#28914=CARTESIAN_POINT('Ctrl Pts',(-2.55971819137861,-4.2010224823229,28.0201554799623));
#28915=CARTESIAN_POINT('Ctrl Pts',(-2.77277881973725,-4.06472858171268,
28.0059856983017));
#28916=CARTESIAN_POINT('Ctrl Pts',(-2.8917168285538,-3.98099157645261,27.9978382151075));
#28917=CARTESIAN_POINT('Ctrl Pts',(-3.06393422329267,-3.84794856499916,
27.9855780091501));
#28918=CARTESIAN_POINT('Ctrl Pts',(-3.12011853845704,-3.80253352789468,
27.9814997558853));
#28919=CARTESIAN_POINT('Ctrl Pts',(-3.22998344081184,-3.70965240351697,
27.9733557472801));
#28920=CARTESIAN_POINT('Ctrl Pts',(-3.28366786876934,-3.66221779127964,
27.9692911497143));
#28921=CARTESIAN_POINT('Ctrl Pts',(-3.46519603675754,-3.49462117479818,
27.9552372996803));
#28922=CARTESIAN_POINT('Ctrl Pts',(-3.58763409094668,-3.36880407902093,
27.9452038028274));
#28923=CARTESIAN_POINT('Ctrl Pts',(-3.76027709422345,-3.17128543387896,
27.9301867077049));
#28924=CARTESIAN_POINT('Ctrl Pts',(-3.81572401225558,-3.1043494527562,27.9252134911518));
#28925=CARTESIAN_POINT('Ctrl Pts',(-3.90562272710818,-2.98977316165656,
27.9169009698753));
#28926=CARTESIAN_POINT('Ctrl Pts',(-3.94104672394121,-2.94292087592703,
27.9135553547005));
#28927=CARTESIAN_POINT('Ctrl Pts',(-3.99726567535598,-2.86572881244737,
27.9081337858815));
#28928=CARTESIAN_POINT('Ctrl Pts',(-4.0185741382421,-2.83577087210833,27.9060515934832));
#28929=CARTESIAN_POINT('Ctrl Pts',(-4.07494777897715,-2.75460257606128,
27.9004668685001));
#28930=CARTESIAN_POINT('Ctrl Pts',(-4.10938286800527,-2.70296269616736,
27.8969726252212));
#28931=CARTESIAN_POINT('Ctrl Pts',(-4.23665238355761,-2.50404948110928,
27.8837030140401));
#28932=CARTESIAN_POINT('Ctrl Pts',(-4.32262202227835,-2.35253620214854,
27.8739793669459));
#28933=CARTESIAN_POINT('Ctrl Pts',(-4.43559540137678,-2.1262392522269,27.8597880819054));
#28934=CARTESIAN_POINT('Ctrl Pts',(-4.46911147023485,-2.05485825172903,
27.8553580398559));
#28935=CARTESIAN_POINT('Ctrl Pts',(-4.53014206231349,-1.91631384345852,
27.8468297530431));
#28936=CARTESIAN_POINT('Ctrl Pts',(-4.55791459892568,-1.84928640286371,
27.8427343642298));
#28937=CARTESIAN_POINT('Ctrl Pts',(-4.60693621162391,-1.72315495123165,
27.835074441021));
#28938=CARTESIAN_POINT('Ctrl Pts',(-4.62855565957063,-1.66421051614048,
27.8315133914064));
#28939=CARTESIAN_POINT('Ctrl Pts',(-4.68954478183092,-1.48753507241695,
27.8208882987025));
#28940=CARTESIAN_POINT('Ctrl Pts',(-4.72559198590939,-1.3687112895878,27.8138045739214));
#28941=CARTESIAN_POINT('Ctrl Pts',(-4.79612881753825,-1.09998073693306,
27.7979125073896));
#28942=CARTESIAN_POINT('Ctrl Pts',(-4.82816152421967,-0.949560843799994,
27.7891030807693));
#28943=CARTESIAN_POINT('Ctrl Pts',(-4.8574396520405,-0.771478708199486,
27.7788060671457));
#28944=CARTESIAN_POINT('Ctrl Pts',(-4.86156593947712,-0.745034225156998,
27.7772804870861));
#28945=CARTESIAN_POINT('Ctrl Pts',(-4.87169198966455,-0.67646898112936,
27.7733346555453));
#28946=CARTESIAN_POINT('Ctrl Pts',(-4.87736146312451,-0.634301456955381,
27.7709174104673));
#28947=CARTESIAN_POINT('Ctrl Pts',(-4.88744892573398,-0.551114924222624,
27.766169708302));
#28948=CARTESIAN_POINT('Ctrl Pts',(-4.89189935573698,-0.510103324827477,
27.7638391295451));
#28949=CARTESIAN_POINT('Ctrl Pts',(-4.91076504978367,-0.313183595528192,
27.7526850318103));
#28950=CARTESIAN_POINT('Ctrl Pts',(-4.91824595464928,-0.156700958163355,
27.7439276774648));
#28951=CARTESIAN_POINT('Ctrl Pts',(-4.91825379372826,0.14683102211351,27.7269217677402));
#28952=CARTESIAN_POINT('Ctrl Pts',(-4.91167091055946,0.293713875980202,
27.718683709383));
#28953=CARTESIAN_POINT('Ctrl Pts',(-4.89283750911437,0.503348143663679,
27.7068200120076));
#28954=CARTESIAN_POINT('Ctrl Pts',(-4.88592836520935,0.566499907694041,
27.7032326011517));
#28955=CARTESIAN_POINT('Ctrl Pts',(-4.86865561443171,0.700341104485991,
27.6955935757652));
#28956=CARTESIAN_POINT('Ctrl Pts',(-4.85797112896173,0.770974387565499,
27.6915406377498));
#28957=CARTESIAN_POINT('Ctrl Pts',(-4.83897493905174,0.880382960974645,
27.685224379158));
#28958=CARTESIAN_POINT('Ctrl Pts',(-4.83172631538794,0.919333132115322,
27.6829681573647));
#28959=CARTESIAN_POINT('Ctrl Pts',(-4.80643809105385,1.04664653224309,27.6755675693476));
#28960=CARTESIAN_POINT('Ctrl Pts',(-4.7864392512841,1.13459872400571,27.6704137044303));
#28961=CARTESIAN_POINT('Ctrl Pts',(-4.76403458666814,1.22194824748421,27.665253726697));
#28962=CARTESIAN_POINT('Ctrl Pts',(-4.76403458719828,1.22194824541733,27.3196847251172));
#28963=CARTESIAN_POINT('Ctrl Pts',(-4.77910664015462,1.16318652465431,27.3231225619925));
#28964=CARTESIAN_POINT('Ctrl Pts',(-4.79309037920283,1.10415033058226,27.3265674431487));
#28965=CARTESIAN_POINT('Ctrl Pts',(-4.83800512637114,0.897560678186405,
27.3385971236683));
#28966=CARTESIAN_POINT('Ctrl Pts',(-4.86324160138916,0.7488584231117,27.347214074077));
#28967=CARTESIAN_POINT('Ctrl Pts',(-4.89374282737757,0.500382881879463,
27.3615443944353));
#28968=CARTESIAN_POINT('Ctrl Pts',(-4.9028718385305,0.401185446940015,27.3672467937488));
#28969=CARTESIAN_POINT('Ctrl Pts',(-4.91287943812325,0.238393742513765,
27.3765605922703));
#28970=CARTESIAN_POINT('Ctrl Pts',(-4.91554805580891,0.174938281813134,
27.3801799444996));
#28971=CARTESIAN_POINT('Ctrl Pts',(-4.91782876595764,0.0743157801970953,
27.3858959242168));
#28972=CARTESIAN_POINT('Ctrl Pts',(-4.91824975924163,0.0371746791460664,
27.3880004070586));
#28973=CARTESIAN_POINT('Ctrl Pts',(-4.91825038350036,-0.0591733338559681,
27.3934466552362));
#28974=CARTESIAN_POINT('Ctrl Pts',(-4.9171817109405,-0.118374257695531,
27.3967813210792));
#28975=CARTESIAN_POINT('Ctrl Pts',(-4.91187445633915,-0.265299510453831,
27.4050456816419));
#28976=CARTESIAN_POINT('Ctrl Pts',(-4.9063546617951,-0.352956948820379,
27.4099661560081));
#28977=CARTESIAN_POINT('Ctrl Pts',(-4.88301364469107,-0.612563181497254,
27.4245690237881));
#28978=CARTESIAN_POINT('Ctrl Pts',(-4.8584730876663,-0.783769267478875,
27.4342428868047));
#28979=CARTESIAN_POINT('Ctrl Pts',(-4.81091144111903,-1.02448809335753,
27.4480673149166));
#28980=CARTESIAN_POINT('Ctrl Pts',(-4.79527870697443,-1.09532949785959,
27.4521629199823));
#28981=CARTESIAN_POINT('Ctrl Pts',(-4.76083643912707,-1.23649288348221,
27.4603891778399));
#28982=CARTESIAN_POINT('Ctrl Pts',(-4.74202117946711,-1.3067950173025,27.4645188864308));
#28983=CARTESIAN_POINT('Ctrl Pts',(-4.64245842199569,-1.6482759436614,27.4847555348174));
#28984=CARTESIAN_POINT('Ctrl Pts',(-4.53997421977378,-1.91255445917514,
27.5010039107848));
#28985=CARTESIAN_POINT('Ctrl Pts',(-4.39463029901634,-2.20875940860351,
27.5198042747874));
#28986=CARTESIAN_POINT('Ctrl Pts',(-4.37331470323292,-2.25066927095974,
27.5224778509426));
#28987=CARTESIAN_POINT('Ctrl Pts',(-4.33312522327585,-2.32696078842439,
27.527366802253));
#28988=CARTESIAN_POINT('Ctrl Pts',(-4.31443491596287,-2.36143433030609,
27.5295840067727));
#28989=CARTESIAN_POINT('Ctrl Pts',(-4.24644045659418,-2.48334493347704,
27.537460588288));
#28990=CARTESIAN_POINT('Ctrl Pts',(-4.19487397899062,-2.56949242933904,
27.5430936468505));
#28991=CARTESIAN_POINT('Ctrl Pts',(-4.0231019911428,-2.83748672226185,27.5609372813293));
#28992=CARTESIAN_POINT('Ctrl Pts',(-3.89343225242221,-3.01294948038046,
27.5731146645195));
#28993=CARTESIAN_POINT('Ctrl Pts',(-3.70788460697584,-3.23195765169718,
27.5893012497431));
#28994=CARTESIAN_POINT('Ctrl Pts',(-3.66210834404674,-3.28373580776761,
27.5932064897484));
#28995=CARTESIAN_POINT('Ctrl Pts',(-3.56315170049135,-3.39102333201989,
27.6014757949685));
#28996=CARTESIAN_POINT('Ctrl Pts',(-3.50973027259484,-3.44628531884541,
27.6058411116085));
#28997=CARTESIAN_POINT('Ctrl Pts',(-3.4228426786759,-3.53205001566902,27.6127933091156));
#28998=CARTESIAN_POINT('Ctrl Pts',(-3.39021222726756,-3.56338186800688,
27.6153726607297));
#28999=CARTESIAN_POINT('Ctrl Pts',(-3.25940096587514,-3.68556382399977,
27.6255909525159));
#29000=CARTESIAN_POINT('Ctrl Pts',(-3.15796386571308,-3.77284232720343,
27.6332502647967));
#29001=CARTESIAN_POINT('Ctrl Pts',(-2.97191923716549,-3.92015309130047,
27.6468317229035));
#29002=CARTESIAN_POINT('Ctrl Pts',(-2.88873190932659,-3.98185039197198,
27.652751621383));
#29003=CARTESIAN_POINT('Ctrl Pts',(-2.77000195668949,-4.06422813092343,
27.6609748508818));
#29004=CARTESIAN_POINT('Ctrl Pts',(-2.73605455053267,-4.08715875627356,
27.6633011676505));
#29005=CARTESIAN_POINT('Ctrl Pts',(-2.66510113670529,-4.13380580959951,
27.6681100472185));
#29006=CARTESIAN_POINT('Ctrl Pts',(-2.62805568685837,-4.15745570133223,
27.6705916441454));
#29007=CARTESIAN_POINT('Ctrl Pts',(-2.54454908869513,-4.20920426839388,
27.6761276461851));
#29008=CARTESIAN_POINT('Ctrl Pts',(-2.49792954644835,-4.23703654608929,
27.6791790489374));
#29009=CARTESIAN_POINT('Ctrl Pts',(-2.33045925713928,-4.33329292100694,
27.6900211157437));
#29010=CARTESIAN_POINT('Ctrl Pts',(-2.20718288335394,-4.39736418719206,
27.6977861998675));
#29011=CARTESIAN_POINT('Ctrl Pts',(-1.98447673868918,-4.50138527487068,
27.7115696326598));
#29012=CARTESIAN_POINT('Ctrl Pts',(-1.88614371151672,-4.54346551083741,
27.717574829586));
#29013=CARTESIAN_POINT('Ctrl Pts',(-1.72724240243759,-4.60541685865395,
27.7271894087988));
#29014=CARTESIAN_POINT('Ctrl Pts',(-1.66752417403003,-4.62737439351549,
27.7307829767372));
#29015=CARTESIAN_POINT('Ctrl Pts',(-1.53849391678187,-4.67199475104879,
27.73851258233));
#29016=CARTESIAN_POINT('Ctrl Pts',(-1.46906988242569,-4.69428716614386,
27.742650320869));
#29017=CARTESIAN_POINT('Ctrl Pts',(-1.22864869051116,-4.76563174826191,
27.7569185713084));
#29018=CARTESIAN_POINT('Ctrl Pts',(-1.05550294794784,-4.80694660336261,
27.7670942024636));
#29019=CARTESIAN_POINT('Ctrl Pts',(-0.874285127402896,-4.83992236715171,
27.7776380610375));
#29020=CARTESIAN_POINT('Ctrl Pts',(-0.868065124335707,-4.84104182423246,
27.7779998260933));
#29021=CARTESIAN_POINT('Ctrl Pts',(-0.754704902465243,-4.86121854857971,
27.7845905317701));
#29022=CARTESIAN_POINT('Ctrl Pts',(-0.646962526460831,-4.87672688904921,
27.7908147037166));
#29023=CARTESIAN_POINT('Ctrl Pts',(-0.496658874532557,-4.89329234176036,
27.799422628598));
#29024=CARTESIAN_POINT('Ctrl Pts',(-0.45446533803561,-4.89739127410771,
27.8018308083105));
#29025=CARTESIAN_POINT('Ctrl Pts',(-0.370069509806744,-4.90448989954287,
27.8066287791068));
#29026=CARTESIAN_POINT('Ctrl Pts',(-0.327870910336513,-4.9074915525872,
27.8090183894714));
#29027=CARTESIAN_POINT('Ctrl Pts',(-0.146909841241898,-4.91801904687589,
27.819237007519));
#29028=CARTESIAN_POINT('Ctrl Pts',(-0.00789989540734039,-4.92020652804115,
27.8270158579821));
#29029=CARTESIAN_POINT('Ctrl Pts',(0.284002930291091,-4.91242778017491,
27.8433742517987));
#29030=CARTESIAN_POINT('Ctrl Pts',(0.436713707293883,-4.90121258153072,
27.8519468360676));
#29031=CARTESIAN_POINT('Ctrl Pts',(0.661331175253825,-4.87413410312265,
27.864691344429));
#29032=CARTESIAN_POINT('Ctrl Pts',(0.733805651596501,-4.86375074189372,
27.8688239785514));
#29033=CARTESIAN_POINT('Ctrl Pts',(0.877179276310579,-4.83993211356035,
27.8770509599861));
#29034=CARTESIAN_POINT('Ctrl Pts',(0.948068523726121,-4.82654661819982,
27.8811439799378));
#29035=CARTESIAN_POINT('Ctrl Pts',(1.15863519648576,-4.78196878133797,27.8933870235219));
#29036=CARTESIAN_POINT('Ctrl Pts',(1.29727150988756,-4.74623500225425,27.9015626863158));
#29037=CARTESIAN_POINT('Ctrl Pts',(1.58643060053522,-4.65808600591162,27.9188647782499));
#29038=CARTESIAN_POINT('Ctrl Pts',(1.73636811638668,-4.60429732463017,27.927985182208));
#29039=CARTESIAN_POINT('Ctrl Pts',(1.91707041808016,-4.52938737170299,27.9391141958223));
#29040=CARTESIAN_POINT('Ctrl Pts',(1.95055176319624,-4.5150699669035,27.9411820112999));
#29041=CARTESIAN_POINT('Ctrl Pts',(2.02255444516446,-4.48332953897129,27.9456397871455));
#29042=CARTESIAN_POINT('Ctrl Pts',(2.06101648713512,-4.46577891681136,27.9480278258118));
#29043=CARTESIAN_POINT('Ctrl Pts',(2.22480973452424,-4.3884715576397,27.9582382582339));
#29044=CARTESIAN_POINT('Ctrl Pts',(2.34780725451158,-4.32391754107525,27.9660105519726));
#29045=CARTESIAN_POINT('Ctrl Pts',(2.60049118808474,-4.17733430289584,27.9823754677308));
#29046=CARTESIAN_POINT('Ctrl Pts',(2.72940375384149,-4.09426803169487,27.9909611339227));
#29047=CARTESIAN_POINT('Ctrl Pts',(2.91383420081883,-3.96284125572686,28.003718286534));
#29048=CARTESIAN_POINT('Ctrl Pts',(2.97248648528547,-3.91903872114196,28.0078503109845));
#29049=CARTESIAN_POINT('Ctrl Pts',(3.08696388672708,-3.82949627216603,28.0160772341931));
#29050=CARTESIAN_POINT('Ctrl Pts',(3.14280357230726,-3.78380407513375,28.02017081168));
#29051=CARTESIAN_POINT('Ctrl Pts',(3.32147034195998,-3.63092122824225,28.0335467222205));
#29052=CARTESIAN_POINT('Ctrl Pts',(3.4399764785869,-3.51885134876122,28.0428655863589));
#29053=CARTESIAN_POINT('Ctrl Pts',(3.64559122903578,-3.30407211351771,28.0598866260259));
#29054=CARTESIAN_POINT('Ctrl Pts',(3.73447134754491,-3.2032721210055,28.0675768165405));
#29055=CARTESIAN_POINT('Ctrl Pts',(3.84557456830109,-3.06635008590321,28.0776134155582));
#29056=CARTESIAN_POINT('Ctrl Pts',(3.87161659684506,-3.03340264294529,28.0799989003056));
#29057=CARTESIAN_POINT('Ctrl Pts',(3.92328721785823,-2.96628128885746,28.084797167374));
#29058=CARTESIAN_POINT('Ctrl Pts',(3.94889901175741,-2.93209889512633,28.0872095684976));
#29059=CARTESIAN_POINT('Ctrl Pts',(3.98986705139168,-2.87591091834472,28.0911292349841));
#29060=CARTESIAN_POINT('Ctrl Pts',(4.00549405280397,-2.85410583221753,28.0926393691978));
#29061=CARTESIAN_POINT('Ctrl Pts',(4.10967540892214,-2.70619571221932,28.1028137701286));
#29062=CARTESIAN_POINT('Ctrl Pts',(4.19243997129744,-2.57611624429883,28.1114274060668));
#29063=CARTESIAN_POINT('Ctrl Pts',(4.3307752579448,-2.33432280005618,28.1270417462924));
#29064=CARTESIAN_POINT('Ctrl Pts',(4.38846439105853,-2.22397324877504,28.1340280022549));
#29065=CARTESIAN_POINT('Ctrl Pts',(4.46906365041017,-2.0544232361273,28.1446126969438));
#29066=CARTESIAN_POINT('Ctrl Pts',(4.49511763558463,-1.99677291606188,28.1481863014903));
#29067=CARTESIAN_POINT('Ctrl Pts',(4.54903526955737,-1.87106058262689,28.1559316198618));
#29068=CARTESIAN_POINT('Ctrl Pts',(4.57649907058771,-1.8028437737091,28.1601053044635));
#29069=CARTESIAN_POINT('Ctrl Pts',(4.63073524212418,-1.6588919832399,28.1688588076293));
#29070=CARTESIAN_POINT('Ctrl Pts',(4.65720268325658,-1.58306490147948,28.1734393486251));
#29071=CARTESIAN_POINT('Ctrl Pts',(4.70976921594585,-1.41971558076114,28.1832454113134));
#29072=CARTESIAN_POINT('Ctrl Pts',(4.73531140851136,-1.33204510402438,28.1884715648637));
#29073=CARTESIAN_POINT('Ctrl Pts',(4.78958757012964,-1.12438690326965,28.2007582338738));
#29074=CARTESIAN_POINT('Ctrl Pts',(4.81627724596558,-1.00392680529061,28.2078151586513));
#29075=CARTESIAN_POINT('Ctrl Pts',(4.84572218818662,-0.842507910818403,
28.2171516126431));
#29076=CARTESIAN_POINT('Ctrl Pts',(4.85253542969403,-0.802336009036839,
28.2194652432138));
#29077=CARTESIAN_POINT('Ctrl Pts',(4.8657060745939,-0.718363381883734,28.2242786989092));
#29078=CARTESIAN_POINT('Ctrl Pts',(4.87197301337525,-0.674552127083557,
28.2267774183482));
#29079=CARTESIAN_POINT('Ctrl Pts',(4.88468395043512,-0.576243554208115,
28.2323629679027));
#29080=CARTESIAN_POINT('Ctrl Pts',(4.89080890646822,-0.521710883021132,
28.235446709414));
#29081=CARTESIAN_POINT('Ctrl Pts',(4.90957613459096,-0.32499216151347,28.2465377996089));
#29082=CARTESIAN_POINT('Ctrl Pts',(4.91693984605702,-0.182374478022377,
28.2545184644196));
#29083=CARTESIAN_POINT('Ctrl Pts',(4.91901000778737,0.0744768507860042,
28.2689243698687));
#29084=CARTESIAN_POINT('Ctrl Pts',(4.91595770000967,0.188588645362122,28.2753357668821));
#29085=CARTESIAN_POINT('Ctrl Pts',(4.90470715233717,0.371167568836646,28.2856561716284));
#29086=CARTESIAN_POINT('Ctrl Pts',(4.89903447178249,0.439748470178235,28.2895466610095));
#29087=CARTESIAN_POINT('Ctrl Pts',(4.88360393041411,0.58828634100926,28.2980117794138));
#29088=CARTESIAN_POINT('Ctrl Pts',(4.87331705197115,0.668168286972844,28.3025888262391));
#29089=CARTESIAN_POINT('Ctrl Pts',(4.8366481225033,0.906547112142942,28.3163318323835));
#29090=CARTESIAN_POINT('Ctrl Pts',(4.80445739636777,1.06403993018608,28.3255272030696));
#29091=CARTESIAN_POINT('Ctrl Pts',(4.73761872025567,1.32514335527237,28.340954341513));
#29092=CARTESIAN_POINT('Ctrl Pts',(4.70712491068458,1.42968931271677,28.3471808706842));
#29093=CARTESIAN_POINT('Ctrl Pts',(4.66017496057225,1.57279835443528,28.3557532613764));
#29094=CARTESIAN_POINT('Ctrl Pts',(4.64665897807504,1.61229207254418,28.358124155228));
#29095=CARTESIAN_POINT('Ctrl Pts',(4.61820498123549,1.69210342842257,28.3629236100915));
#29096=CARTESIAN_POINT('Ctrl Pts',(4.60323773958668,1.73240688994969,28.3653516546656));
#29097=CARTESIAN_POINT('Ctrl Pts',(4.57797811034502,1.79778579336996,28.3693021325725));
#29098=CARTESIAN_POINT('Ctrl Pts',(4.56800355722883,1.82298130805904,28.3708274386453));
#29099=CARTESIAN_POINT('Ctrl Pts',(4.52769759397163,1.92238504865047,28.3768593199991));
#29100=CARTESIAN_POINT('Ctrl Pts',(4.49576183275263,1.99592972571498,28.381353508632));
#29101=CARTESIAN_POINT('Ctrl Pts',(4.38092286391547,2.24363406392164,28.3966522881875));
#29102=CARTESIAN_POINT('Ctrl Pts',(4.28958227150522,2.41368220504275,28.4074395892206));
#29103=CARTESIAN_POINT('Ctrl Pts',(4.15493754422802,2.63244670094294,28.4219187033801));
#29104=CARTESIAN_POINT('Ctrl Pts',(4.12032001285049,2.6863068532354,28.4255342467014));
#29105=CARTESIAN_POINT('Ctrl Pts',(4.04437768201028,2.79953973034755,28.4332522700233));
#29106=CARTESIAN_POINT('Ctrl Pts',(4.00277455314677,2.85870761861537,28.4373561820006));
#29107=CARTESIAN_POINT('Ctrl Pts',(3.93600042075573,2.94935674138122,28.4437608182109));
#29108=CARTESIAN_POINT('Ctrl Pts',(3.91172149589689,2.98148275417654,28.4460542928108));
#29109=CARTESIAN_POINT('Ctrl Pts',(3.76930565852005,3.16519375123499,28.4593089850434));
#29110=CARTESIAN_POINT('Ctrl Pts',(3.64275957807015,3.31004808286288,28.4703238265961));
#29111=CARTESIAN_POINT('Ctrl Pts',(3.45581488703851,3.50029769952538,28.4855725612512));
#29112=CARTESIAN_POINT('Ctrl Pts',(3.40236244327276,3.55227680707081,28.489827317804));
#29113=CARTESIAN_POINT('Ctrl Pts',(3.32213028544329,3.62682455259156,28.4960546674957));
#29114=CARTESIAN_POINT('Ctrl Pts',(3.29625847313596,3.65035424186864,28.4980393804124));
#29115=CARTESIAN_POINT('Ctrl Pts',(3.23639542235603,3.70364259294379,28.5025772213728));
#29116=CARTESIAN_POINT('Ctrl Pts',(3.20224066367408,3.73321290359667,28.5051273548071));
#29117=CARTESIAN_POINT('Ctrl Pts',(3.124363064727,3.79878209935102,28.5108626629883));
#29118=CARTESIAN_POINT('Ctrl Pts',(3.08041601933012,3.83450482160636,28.5140444825973));
#29119=CARTESIAN_POINT('Ctrl Pts',(2.91370875684388,3.96529828432435,28.5259347697592));
#29120=CARTESIAN_POINT('Ctrl Pts',(2.78708621106047,4.05529774066534,28.5346129459366));
#29121=CARTESIAN_POINT('Ctrl Pts',(2.56895289199282,4.19529086741223,28.5491583369249));
#29122=CARTESIAN_POINT('Ctrl Pts',(2.47973018609867,4.2486376927477,28.5550018884223));
#29123=CARTESIAN_POINT('Ctrl Pts',(2.32922551944268,4.33226843972326,28.5647200173306));
#29124=CARTESIAN_POINT('Ctrl Pts',(2.26888255180403,4.36417382575838,28.5685806733646));
#29125=CARTESIAN_POINT('Ctrl Pts',(2.13276396672084,4.43255799619636,28.5772188586075));
#29126=CARTESIAN_POINT('Ctrl Pts',(2.0566774316101,4.46836997392018,28.5820000482211));
#29127=CARTESIAN_POINT('Ctrl Pts',(1.85033588765594,4.55910237034454,28.5948509739652));
#29128=CARTESIAN_POINT('Ctrl Pts',(1.71856967190759,4.61038772860394,28.6029387109716));
#29129=CARTESIAN_POINT('Ctrl Pts',(1.47068824604421,4.69476134028943,28.6179279555619));
#29130=CARTESIAN_POINT('Ctrl Pts',(1.35520716814436,4.72938917808434,28.6248232913193));
#29131=CARTESIAN_POINT('Ctrl Pts',(1.19872264178285,4.77010926744782,28.6340250560022));
#29132=CARTESIAN_POINT('Ctrl Pts',(1.15874622440408,4.77997757778943,28.6363634428941));
#29133=CARTESIAN_POINT('Ctrl Pts',(1.07612275012614,4.79927600229902,28.6411688102927));
#29134=CARTESIAN_POINT('Ctrl Pts',(1.03346447869706,4.80864238131384,28.643634952647));
#29135=CARTESIAN_POINT('Ctrl Pts',(0.987976504581639,4.81799679797234,28.6462520646928));
#29136=CARTESIAN_POINT('Ctrl Pts',(0.985265733875814,4.81855187297385,28.646407979021));
#29137=CARTESIAN_POINT('Ctrl Pts',(0.979138229391013,4.81980119364637,28.6467603064267));
#29138=CARTESIAN_POINT('Ctrl Pts',(0.97572122229174,4.82049409448077,28.6469567077));
#29139=CARTESIAN_POINT('Ctrl Pts',(0.967957982456228,4.82205973190601,28.6474027543141));
#29140=CARTESIAN_POINT('Ctrl Pts',(0.963611299782327,4.82293022724261,28.6476523805736));
#29141=CARTESIAN_POINT('Ctrl Pts',(0.89733369705242,4.83611024079225,28.6514568960207));
#29142=CARTESIAN_POINT('Ctrl Pts',(0.835172132741159,4.84723195573967,28.6550019207052));
#29143=CARTESIAN_POINT('Ctrl Pts',(0.565439360243222,4.89014867084298,28.6703193184863));
#29144=CARTESIAN_POINT('Ctrl Pts',(0.356166504937161,4.90982896225183,28.6820466056942));
#29145=CARTESIAN_POINT('Ctrl Pts',(0.0718565180112681,4.91828865017303,
28.6980644157156));
#29146=CARTESIAN_POINT('Ctrl Pts',(-0.00260559164015547,4.91881282876319,
28.7022663170975));
#29147=CARTESIAN_POINT('Ctrl Pts',(-0.102471169947986,4.91724812293407,
28.7079185593585));
#29148=CARTESIAN_POINT('Ctrl Pts',(-0.127888523762721,4.91665271921554,
28.7093585874028));
#29149=CARTESIAN_POINT('Ctrl Pts',(-0.217155594013457,4.91386894483474,
28.7144217171674));
#29150=CARTESIAN_POINT('Ctrl Pts',(-0.280965825585294,4.91063363047964,
28.7180512531133));
#29151=CARTESIAN_POINT('Ctrl Pts',(-0.429180193272093,4.90022045396422,
28.7265100472542));
#29152=CARTESIAN_POINT('Ctrl Pts',(-0.513497897093821,4.89210341733593,
28.7313437472703));
#29153=CARTESIAN_POINT('Ctrl Pts',(-0.762648780010405,4.86160585268035,
28.7456943287239));
#29154=CARTESIAN_POINT('Ctrl Pts',(-0.926603012511395,4.8330375120958,28.7552290214487));
#29155=CARTESIAN_POINT('Ctrl Pts',(-1.14469831378069,4.78352747945629,28.7679927519579));
#29156=CARTESIAN_POINT('Ctrl Pts',(-1.20037664019074,4.76986010368093,28.7712579791606));
#29157=CARTESIAN_POINT('Ctrl Pts',(-1.29014985538233,4.74615195106764,28.7765292355202));
#29158=CARTESIAN_POINT('Ctrl Pts',(-1.32439671379123,4.73670965661069,28.77854135565));
#29159=CARTESIAN_POINT('Ctrl Pts',(-1.36179459480854,4.72596128003796,28.7807405335028));
#29160=CARTESIAN_POINT('Ctrl Pts',(-1.36504950452029,4.72502215752535,28.7809319566299));
#29161=CARTESIAN_POINT('Ctrl Pts',(-1.3715141144292,4.72314971916441,28.7813121837065));
#29162=CARTESIAN_POINT('Ctrl Pts',(-1.3747238385518,4.72221649265107,28.7815009885362));
#29163=CARTESIAN_POINT('Ctrl Pts',(-1.38126323497621,4.72030793234563,28.781885696161));
#29164=CARTESIAN_POINT('Ctrl Pts',(-1.38459283172663,4.71933234587507,28.7820815961177));
#29165=CARTESIAN_POINT('Ctrl Pts',(-1.39151162511814,4.71729715671113,28.7824887193799));
#29166=CARTESIAN_POINT('Ctrl Pts',(-1.3951006506325,4.71623697901138,28.782699936512));
#29167=CARTESIAN_POINT('Ctrl Pts',(-1.40267892084696,4.71398899366806,28.7831459864932));
#29168=CARTESIAN_POINT('Ctrl Pts',(-1.40666787529463,4.7128002160153,28.7833808092733));
#29169=CARTESIAN_POINT('Ctrl Pts',(-1.41275565697022,4.71097753370377,28.7837392460887));
#29170=CARTESIAN_POINT('Ctrl Pts',(-1.41485557539758,4.71034728763562,28.7838628960867));
#29171=CARTESIAN_POINT('Ctrl Pts',(-1.41992992337434,4.70882063004978,28.7841617172675));
#29172=CARTESIAN_POINT('Ctrl Pts',(-1.42290392711492,4.70792280390154,28.7843368746921));
#29173=CARTESIAN_POINT('Ctrl Pts',(-1.43022165360188,4.70570607788711,28.7847679187994));
#29174=CARTESIAN_POINT('Ctrl Pts',(-1.434564406371,4.70438398028115,28.785023775135));
#29175=CARTESIAN_POINT('Ctrl Pts',(-1.44545804675964,4.70105105853871,28.7856657161714));
#29176=CARTESIAN_POINT('Ctrl Pts',(-1.45200657750312,4.69903255138802,28.786051730575));
#29177=CARTESIAN_POINT('Ctrl Pts',(-1.46872298743884,4.69384163538837,28.7870374484657));
#29178=CARTESIAN_POINT('Ctrl Pts',(-1.47888482673903,4.6906498677499,28.7876369846345));
#29179=CARTESIAN_POINT('Ctrl Pts',(-1.55713229242439,4.66579329752412,28.7922562884239));
#29180=CARTESIAN_POINT('Ctrl Pts',(-1.62474931117814,4.64268003105917,28.7962645004704));
#29181=CARTESIAN_POINT('Ctrl Pts',(-1.88541671192035,4.54718466822189,28.811825196722));
#29182=CARTESIAN_POINT('Ctrl Pts',(-2.07434217828095,4.46416711954959,28.8233469248984));
#29183=CARTESIAN_POINT('Ctrl Pts',(-2.31408634113183,4.34030464060959,28.8385548453371));
#29184=CARTESIAN_POINT('Ctrl Pts',(-2.37010044196303,4.3099725930651,28.8421513388132));
#29185=CARTESIAN_POINT('Ctrl Pts',(-2.48153187233769,4.2468023037472,28.8494009983861));
#29186=CARTESIAN_POINT('Ctrl Pts',(-2.53692491444979,4.21394614370595,28.8530536517444));
#29187=CARTESIAN_POINT('Ctrl Pts',(-2.65383921936443,4.14145790538518,28.8608736196204));
#29188=CARTESIAN_POINT('Ctrl Pts',(-2.71515354863834,4.10152133284737,28.8650423667111));
#29189=CARTESIAN_POINT('Ctrl Pts',(-2.88662013502916,3.98430766146196,28.8768995480995));
#29190=CARTESIAN_POINT('Ctrl Pts',(-2.99452400915693,3.90385821332883,28.884603488743));
#29191=CARTESIAN_POINT('Ctrl Pts',(-3.17846201463924,3.75460196662519,28.8981602068985));
#29192=CARTESIAN_POINT('Ctrl Pts',(-3.25589964909399,3.68765163061946,28.9040110664808));
#29193=CARTESIAN_POINT('Ctrl Pts',(-3.36131336781451,3.59060325587615,28.9121645545975));
#29194=CARTESIAN_POINT('Ctrl Pts',(-3.39108694317198,3.56249753738953,28.91448957866));
#29195=CARTESIAN_POINT('Ctrl Pts',(-3.42326688529033,3.53135125039662,28.9170258180568));
#29196=CARTESIAN_POINT('Ctrl Pts',(-3.42602426245999,3.52867617877976,28.9172433301593));
#29197=CARTESIAN_POINT('Ctrl Pts',(-3.46123304208364,3.49443818120701,28.9200232042756));
#29198=CARTESIAN_POINT('Ctrl Pts',(-3.49325056492841,3.46243164976422,28.9225780511367));
#29199=CARTESIAN_POINT('Ctrl Pts',(-3.55376359562376,3.40024551650027,28.9274652764312));
#29200=CARTESIAN_POINT('Ctrl Pts',(-3.58232785172381,3.37013834466104,28.9297982582826));
#29201=CARTESIAN_POINT('Ctrl Pts',(-3.69141267097097,3.25220716644448,28.9388189721813));
#29202=CARTESIAN_POINT('Ctrl Pts',(-3.76911279712212,3.16182983409066,28.9454853046441));
#29203=CARTESIAN_POINT('Ctrl Pts',(-3.92593905871077,2.96541094130583,28.9595701864866));
#29204=CARTESIAN_POINT('Ctrl Pts',(-4.00422415830557,2.85881930647059,28.966985760214));
#29205=CARTESIAN_POINT('Ctrl Pts',(-4.11130943689565,2.69997098343283,28.9777840104923));
#29206=CARTESIAN_POINT('Ctrl Pts',(-4.14360505763804,2.65014068205228,28.9811368928025));
#29207=CARTESIAN_POINT('Ctrl Pts',(-4.19105812528317,2.57393450913857,28.9862172341388));
#29208=CARTESIAN_POINT('Ctrl Pts',(-4.20688628874769,2.54798249757374,28.987939229281));
#29209=CARTESIAN_POINT('Ctrl Pts',(-4.25547606531191,2.46662709552304,28.9933131560861));
#29210=CARTESIAN_POINT('Ctrl Pts',(-4.28739118937481,2.41072653934366,28.9969710587362));
#29211=CARTESIAN_POINT('Ctrl Pts',(-4.36036909069504,2.27686747961953,29.0056535591906));
#29212=CARTESIAN_POINT('Ctrl Pts',(-4.40045223983104,2.19840032675795,29.0106833445267));
#29213=CARTESIAN_POINT('Ctrl Pts',(-4.50925167170404,1.97050088067716,29.0251254555451));
#29214=CARTESIAN_POINT('Ctrl Pts',(-4.57261031405347,1.8186422181361,29.0345521930793));
#29215=CARTESIAN_POINT('Ctrl Pts',(-4.6463560602586,1.6135132112343,29.0469868174237));
#29216=CARTESIAN_POINT('Ctrl Pts',(-4.66364523893352,1.56283802791021,29.05003482225));
#29217=CARTESIAN_POINT('Ctrl Pts',(-4.69060112825528,1.47939522869703,29.0550111931308));
#29218=CARTESIAN_POINT('Ctrl Pts',(-4.7007598099838,1.44679176879886,29.0569447754866));
#29219=CARTESIAN_POINT('Ctrl Pts',(-4.72483473814913,1.36659372332528,29.0616762149042));
#29220=CARTESIAN_POINT('Ctrl Pts',(-4.73837233632022,1.31888945107595,29.0644698259977));
#29221=CARTESIAN_POINT('Ctrl Pts',(-4.75555358007278,1.2546628245821,29.0682088437209));
#29222=CARTESIAN_POINT('Ctrl Pts',(-4.75983637069872,1.23831591791709,29.0691585809229));
#29223=CARTESIAN_POINT('Ctrl Pts',(-4.76403458843593,1.2219482405921,29.0701077704777));
#29224=CARTESIAN_POINT('Origin',(0.,0.,-3.23514056400928));
#29225=CARTESIAN_POINT('',(-4.76403458668766,1.2219482474081,31.1654428831549));
#29226=CARTESIAN_POINT('',(-4.76403458704967,1.22194824599672,30.8199238152312));
#29227=CARTESIAN_POINT('',(-4.76403458704967,1.22194824599672,-3.23514056400928));
#29228=CARTESIAN_POINT('',(-4.91824995130769,0.000107359571118153,29.4853029780633));
#29229=CARTESIAN_POINT('Ctrl Pts',(-4.76403458668766,1.2219482474081,31.1654428831549));
#29230=CARTESIAN_POINT('Ctrl Pts',(-4.75747531537793,1.24752101241618,31.1639437083435));
#29231=CARTESIAN_POINT('Ctrl Pts',(-4.7507100794633,1.27304118690602,31.1624431868895));
#29232=CARTESIAN_POINT('Ctrl Pts',(-4.70273686558152,1.44829827449206,31.1521070958768));
#29233=CARTESIAN_POINT('Ctrl Pts',(-4.65466277484179,1.59606243649511,31.1432307642279));
#29234=CARTESIAN_POINT('Ctrl Pts',(-4.54929617340791,1.87439009344354,31.1261951866103));
#29235=CARTESIAN_POINT('Ctrl Pts',(-4.49316021950789,2.00522960892285,31.1180465608187));
#29236=CARTESIAN_POINT('Ctrl Pts',(-4.41349333381479,2.17070710999003,31.1075938485764));
#29237=CARTESIAN_POINT('Ctrl Pts',(-4.39508779041059,2.20773552225107,31.1052452508279));
#29238=CARTESIAN_POINT('Ctrl Pts',(-4.35685174862786,2.28228538330546,31.1004994382882));
#29239=CARTESIAN_POINT('Ctrl Pts',(-4.33699813998058,2.31979113722606,31.0981026882424));
#29240=CARTESIAN_POINT('Ctrl Pts',(-4.26391079915593,2.45364287839366,31.0895062631372));
#29241=CARTESIAN_POINT('Ctrl Pts',(-4.20793129825726,2.54845312823083,31.0833358918565));
#29242=CARTESIAN_POINT('Ctrl Pts',(-4.0474840780041,2.80047475603626,31.0665956161659));
#29243=CARTESIAN_POINT('Ctrl Pts',(-3.93707598730645,2.95367869615756,31.0560402687495));
#29244=CARTESIAN_POINT('Ctrl Pts',(-3.77348996620301,3.15515043602749,31.0414138581479));
#29245=CARTESIAN_POINT('Ctrl Pts',(-3.72765689908364,3.20917040534007,31.0374130690057));
#29246=CARTESIAN_POINT('Ctrl Pts',(-3.63212474204785,3.31695800390257,31.0292569899486));
#29247=CARTESIAN_POINT('Ctrl Pts',(-3.58235967906493,3.37064378152434,31.0251020008058));
#29248=CARTESIAN_POINT('Ctrl Pts',(-3.47559637167496,3.48078217889091,31.0163730626085));
#29249=CARTESIAN_POINT('Ctrl Pts',(-3.41837758207695,3.53699155275009,31.0117983289139));
#29250=CARTESIAN_POINT('Ctrl Pts',(-3.22484868904486,3.71802186933397,30.9966545487602));
#29251=CARTESIAN_POINT('Ctrl Pts',(-3.08287878122176,3.83656019996987,30.9860566616643));
#29252=CARTESIAN_POINT('Ctrl Pts',(-2.8920143667442,3.978473184575,30.9724897751801));
#29253=CARTESIAN_POINT('Ctrl Pts',(-2.84894350929977,4.00942850673985,30.9694704631617));
#29254=CARTESIAN_POINT('Ctrl Pts',(-2.77807365240271,4.05864448870143,30.9645738548085));
#29255=CARTESIAN_POINT('Ctrl Pts',(-2.75057567527664,4.0773302274215,30.9626912872225));
#29256=CARTESIAN_POINT('Ctrl Pts',(-2.67134815790107,4.1300015467316,30.9573148163061));
#29257=CARTESIAN_POINT('Ctrl Pts',(-2.61916359822708,4.1632914792067,30.9538300409974));
#29258=CARTESIAN_POINT('Ctrl Pts',(-2.48500337199467,4.24535483080896,30.9449925147789));
#29259=CARTESIAN_POINT('Ctrl Pts',(-2.40221169471751,4.29274487466121,30.939650674331));
#29260=CARTESIAN_POINT('Ctrl Pts',(-2.17852872115839,4.41228252387011,30.9254424417252));
#29261=CARTESIAN_POINT('Ctrl Pts',(-2.03544626049433,4.48008729879932,30.9165799502979));
#29262=CARTESIAN_POINT('Ctrl Pts',(-1.82246262903994,4.56870449987658,30.9035845490042));
#29263=CARTESIAN_POINT('Ctrl Pts',(-1.75497333668192,4.59505160679282,30.8994948981396));
#29264=CARTESIAN_POINT('Ctrl Pts',(-1.61981661652591,4.64440324797767,30.8913501275608));
#29265=CARTESIAN_POINT('Ctrl Pts',(-1.55218051364651,4.66744286472769,30.8872962796406));
#29266=CARTESIAN_POINT('Ctrl Pts',(-1.34069098583087,4.73437922629607,30.8746785770657));
#29267=CARTESIAN_POINT('Ctrl Pts',(-1.19531061153262,4.77315729089733,30.8660850747287));
#29268=CARTESIAN_POINT('Ctrl Pts',(-0.90228417064475,4.8370887566735,30.8489178906732));
#29269=CARTESIAN_POINT('Ctrl Pts',(-0.754805171813162,4.86228487674438,
30.8403533381151));
#29270=CARTESIAN_POINT('Ctrl Pts',(-0.565824311542138,4.8857648611962,30.8295161727133));
#29271=CARTESIAN_POINT('Ctrl Pts',(-0.525180080183103,4.89030074459523,
30.8271936406343));
#29272=CARTESIAN_POINT('Ctrl Pts',(-0.441726505655083,4.89856171191949,
30.822443908699));
#29273=CARTESIAN_POINT('Ctrl Pts',(-0.398915374270311,4.90223374935372,
30.8200174234302));
#29274=CARTESIAN_POINT('Ctrl Pts',(-0.328959622948482,4.90731158583249,
30.8160642960322));
#29275=CARTESIAN_POINT('Ctrl Pts',(-0.301841996113542,4.90905417103023,
30.814534818718));
#29276=CARTESIAN_POINT('Ctrl Pts',(-0.194050481796607,4.91508433199235,
30.8084640918898));
#29277=CARTESIAN_POINT('Ctrl Pts',(-0.113290324852295,4.91760867010689,
30.803935327558));
#29278=CARTESIAN_POINT('Ctrl Pts',(0.159168546390112,4.91940936694677,30.7886683059716));
#29279=CARTESIAN_POINT('Ctrl Pts',(0.350749640771354,4.90947010715552,30.777946326266));
#29280=CARTESIAN_POINT('Ctrl Pts',(0.604314000039364,4.88139449940297,30.7635663169093));
#29281=CARTESIAN_POINT('Ctrl Pts',(0.667227018044355,4.87319357990585,30.7599835039854));
#29282=CARTESIAN_POINT('Ctrl Pts',(0.800709250460242,4.85316035979293,30.7523428035817));
#29283=CARTESIAN_POINT('Ctrl Pts',(0.871214505773545,4.84100050686251,30.7482835406051));
#29284=CARTESIAN_POINT('Ctrl Pts',(1.09794506296865,4.79678316629855,30.7351437485202));
#29285=CARTESIAN_POINT('Ctrl Pts',(1.25288238607207,4.75866543109589,30.7260285979407));
#29286=CARTESIAN_POINT('Ctrl Pts',(1.53814217159968,4.67358591925001,30.7089884859344));
#29287=CARTESIAN_POINT('Ctrl Pts',(1.6688694393235,4.62851618701025,30.7010750264283));
#29288=CARTESIAN_POINT('Ctrl Pts',(1.836219632701,4.56280709568751,30.6908418920887));
#29289=CARTESIAN_POINT('Ctrl Pts',(1.87471996684793,4.54712395183278,30.6884805799674));
#29290=CARTESIAN_POINT('Ctrl Pts',(1.95188771987945,4.51454290638366,30.6837356486427));
#29291=CARTESIAN_POINT('Ctrl Pts',(1.99054581427608,4.49763168137312,30.6813523786775));
#29292=CARTESIAN_POINT('Ctrl Pts',(2.07561292067222,4.45910691741121,30.6760882171418));
#29293=CARTESIAN_POINT('Ctrl Pts',(2.12191180179166,4.43726197876472,30.6732098881597));
#29294=CARTESIAN_POINT('Ctrl Pts',(2.27638670229846,4.36140624034259,30.6635466975161));
#29295=CARTESIAN_POINT('Ctrl Pts',(2.38291030268977,4.30413051792195,30.6567823524661));
#29296=CARTESIAN_POINT('Ctrl Pts',(2.60027529792051,4.17671239505201,30.6426621986406));
#29297=CARTESIAN_POINT('Ctrl Pts',(2.71064012418522,4.10594539304553,30.6353097755382));
#29298=CARTESIAN_POINT('Ctrl Pts',(2.86980891315586,3.99466755691141,30.6243616261251));
#29299=CARTESIAN_POINT('Ctrl Pts',(2.92086974028756,3.95748555791618,30.6207943183749));
#29300=CARTESIAN_POINT('Ctrl Pts',(3.02852364592336,3.87587435989815,30.6131464294742));
#29301=CARTESIAN_POINT('Ctrl Pts',(3.08488657032127,3.8311659079648,30.6090642900197));
#29302=CARTESIAN_POINT('Ctrl Pts',(3.17117214094017,3.75958305794207,30.6026864109259));
#29303=CARTESIAN_POINT('Ctrl Pts',(3.20178045922284,3.73355050629159,30.6003978001166));
#29304=CARTESIAN_POINT('Ctrl Pts',(3.37871767862999,3.57928821865468,30.5870119455222));
#29305=CARTESIAN_POINT('Ctrl Pts',(3.51765245924632,3.44284148755095,30.5758598417647));
#29306=CARTESIAN_POINT('Ctrl Pts',(3.69848522217757,3.24284222763085,30.5604475568804));
#29307=CARTESIAN_POINT('Ctrl Pts',(3.74755180551059,3.18601229112869,30.5561640899859));
#29308=CARTESIAN_POINT('Ctrl Pts',(3.81896963361591,3.09936108751663,30.5497818390881));
#29309=CARTESIAN_POINT('Ctrl Pts',(3.84231402129371,3.07037314203322,30.5476709332088));
#29310=CARTESIAN_POINT('Ctrl Pts',(3.89623069721223,3.00184397405024,30.5427376361647));
#29311=CARTESIAN_POINT('Ctrl Pts',(3.9265337328691,2.9620961864868,30.5399190173322));
#29312=CARTESIAN_POINT('Ctrl Pts',(3.99574295663878,2.86838730947251,30.5333622522042));
#29313=CARTESIAN_POINT('Ctrl Pts',(4.03417071841867,2.81408497662551,30.52962909689));
#29314=CARTESIAN_POINT('Ctrl Pts',(4.19833314793241,2.57183047101487,30.5132213320537));
#29315=CARTESIAN_POINT('Ctrl Pts',(4.31211955121054,2.37611803777547,30.5005917090974));
#29316=CARTESIAN_POINT('Ctrl Pts',(4.44221423223513,2.1120085215405,30.4839877415829));
#29317=CARTESIAN_POINT('Ctrl Pts',(4.47111281545186,2.05012129744831,30.4801279288461));
#29318=CARTESIAN_POINT('Ctrl Pts',(4.52959758855043,1.91775099326645,30.471928519319));
#29319=CARTESIAN_POINT('Ctrl Pts',(4.55884843365432,1.84713939787589,30.467587558904));
#29320=CARTESIAN_POINT('Ctrl Pts',(4.62542245390094,1.67520287119621,30.4570881917116));
#29321=CARTESIAN_POINT('Ctrl Pts',(4.66107748433156,1.57327488035465,30.4509214655097));
#29322=CARTESIAN_POINT('Ctrl Pts',(4.7446797778377,1.306399974715,30.4349201464463));
#29323=CARTESIAN_POINT('Ctrl Pts',(4.78739440141907,1.13996608300871,30.4250781393178));
#29324=CARTESIAN_POINT('Ctrl Pts',(4.82952520913053,0.930911086693913,30.4129400434828));
#29325=CARTESIAN_POINT('Ctrl Pts',(4.83721676751018,0.890080443924282,30.4105800675428));
#29326=CARTESIAN_POINT('Ctrl Pts',(4.85167922569719,0.807572975481787,30.4058350728294));
#29327=CARTESIAN_POINT('Ctrl Pts',(4.858432663947,0.765896549925473,30.4034504152531));
#29328=CARTESIAN_POINT('Ctrl Pts',(4.86854280318443,0.697978178813625,30.3995796172955));
#29329=CARTESIAN_POINT('Ctrl Pts',(4.87222582391646,0.671787239702785,30.3980906525679));
#29330=CARTESIAN_POINT('Ctrl Pts',(4.89623220584169,0.490477300675998,30.3878044091572));
#29331=CARTESIAN_POINT('Ctrl Pts',(4.90935555213833,0.334494400992546,30.3790597983883));
#29332=CARTESIAN_POINT('Ctrl Pts',(4.91947459127942,0.0553193741177052,
30.3634003525522));
#29333=CARTESIAN_POINT('Ctrl Pts',(4.91932063394959,-0.0676347365759319,
30.3565012782735));
#29334=CARTESIAN_POINT('Ctrl Pts',(4.91213242227513,-0.25312390782555,30.3460350832642));
#29335=CARTESIAN_POINT('Ctrl Pts',(4.90850518984122,-0.315742525446427,
30.3424920372609));
#29336=CARTESIAN_POINT('Ctrl Pts',(4.89809360166084,-0.450711053718308,
30.3348272133237));
#29337=CARTESIAN_POINT('Ctrl Pts',(4.89090144516376,-0.523014600482981,
30.3307035633953));
#29338=CARTESIAN_POINT('Ctrl Pts',(4.87254250870178,-0.673620520373063,
30.3220708429589));
#29339=CARTESIAN_POINT('Ctrl Pts',(4.8610833637056,-0.751866652358065,30.3175611244853));
#29340=CARTESIAN_POINT('Ctrl Pts',(4.81808231297128,-1.00308087681873,30.3029983105498));
#29341=CARTESIAN_POINT('Ctrl Pts',(4.77915247976308,-1.174644586987,30.2929189763384));
#29342=CARTESIAN_POINT('Ctrl Pts',(4.71455997206945,-1.40206329645317,30.2794222431633));
#29343=CARTESIAN_POINT('Ctrl Pts',(4.6969222462346,-1.46006121678644,30.275968597111));
#29344=CARTESIAN_POINT('Ctrl Pts',(4.66687678524039,-1.55267335795665,30.2704400636562));
#29345=CARTESIAN_POINT('Ctrl Pts',(4.65514530592551,-1.58749982878772,30.2683582742569));
#29346=CARTESIAN_POINT('Ctrl Pts',(4.62321379020557,-1.67889394644738,30.2628864638555));
#29347=CARTESIAN_POINT('Ctrl Pts',(4.60236591329271,-1.73522873487296,30.259503956053));
#29348=CARTESIAN_POINT('Ctrl Pts',(4.54757305528337,-1.87534859517788,30.2510477491439));
#29349=CARTESIAN_POINT('Ctrl Pts',(4.51234029602041,-1.9586062071877,30.2459838294301));
#29350=CARTESIAN_POINT('Ctrl Pts',(4.40563612213864,-2.19256966591863,30.2315776129323));
#29351=CARTESIAN_POINT('Ctrl Pts',(4.32876809807629,-2.34067453818446,30.2222417888935));
#29352=CARTESIAN_POINT('Ctrl Pts',(4.20799355066273,-2.54699886581245,30.2087733311054));
#29353=CARTESIAN_POINT('Ctrl Pts',(4.17008838194017,-2.60859649475921,30.204690531341));
#29354=CARTESIAN_POINT('Ctrl Pts',(4.0920031424588,-2.72943464719803,30.1965462826716));
#29355=CARTESIAN_POINT('Ctrl Pts',(4.05186057758402,-2.78867870358175,30.1924860373212));
#29356=CARTESIAN_POINT('Ctrl Pts',(3.90299964121195,-2.99837050147047,30.177858376316));
#29357=CARTESIAN_POINT('Ctrl Pts',(3.78707936746813,-3.14351079058454,30.1672398971431));
#29358=CARTESIAN_POINT('Ctrl Pts',(3.63267188146699,-3.31586734446963,30.153994238295));
#29359=CARTESIAN_POINT('Ctrl Pts',(3.60163224687229,-3.34955615245243,30.1513730208839));
#29360=CARTESIAN_POINT('Ctrl Pts',(3.51826088620866,-3.43754413051739,30.1444428580303));
#29361=CARTESIAN_POINT('Ctrl Pts',(3.46514280449843,-3.49108218910521,30.1401386862681));
#29362=CARTESIAN_POINT('Ctrl Pts',(3.38568068009294,-3.56757150125414,30.1338667449964));
#29363=CARTESIAN_POINT('Ctrl Pts',(3.36029009124276,-3.59149698991795,30.13188658925));
#29364=CARTESIAN_POINT('Ctrl Pts',(3.30234063612166,-3.64495008103297,30.1274222110345));
#29365=CARTESIAN_POINT('Ctrl Pts',(3.26963613202736,-3.67431550025022,30.1249406476618));
#29366=CARTESIAN_POINT('Ctrl Pts',(3.19552588414164,-3.73908608464441,30.1193945683724));
#29367=CARTESIAN_POINT('Ctrl Pts',(3.15391660508507,-3.77424966673595,30.1163330881093));
#29368=CARTESIAN_POINT('Ctrl Pts',(3.0024456320413,-3.898001905774,30.1053547203128));
#29369=CARTESIAN_POINT('Ctrl Pts',(2.88936721758554,-3.98254389682634,30.0974639975508));
#29370=CARTESIAN_POINT('Ctrl Pts',(2.67784462600841,-4.12693006687821,30.08310115895));
#29371=CARTESIAN_POINT('Ctrl Pts',(2.58063615465586,-4.18840305810381,30.0766419043654));
#29372=CARTESIAN_POINT('Ctrl Pts',(2.42238011074505,-4.2808789617415,30.066301301867));
#29373=CARTESIAN_POINT('Ctrl Pts',(2.36268521310744,-4.31411271659658,30.0624389758384));
#29374=CARTESIAN_POINT('Ctrl Pts',(2.23257113084391,-4.38303992352201,30.0540934005721));
#29375=CARTESIAN_POINT('Ctrl Pts',(2.16194566632971,-4.41830324378555,30.0496080682049));
#29376=CARTESIAN_POINT('Ctrl Pts',(1.94563120670292,-4.51988030742191,30.0359933051998));
#29377=CARTESIAN_POINT('Ctrl Pts',(1.79752642820525,-4.58079650503639,30.0268339467352));
#29378=CARTESIAN_POINT('Ctrl Pts',(1.60371963417071,-4.64966113206032,30.0150609270679));
#29379=CARTESIAN_POINT('Ctrl Pts',(1.56051110414909,-4.66434029818212,30.0124496790555));
#29380=CARTESIAN_POINT('Ctrl Pts',(1.44526002767175,-4.70171361508314,30.005522549396));
#29381=CARTESIAN_POINT('Ctrl Pts',(1.37288779678485,-4.7233533382413,30.0012114669173));
#29382=CARTESIAN_POINT('Ctrl Pts',(1.26638371390079,-4.7525439061861,29.9949316557589));
#29383=CARTESIAN_POINT('Ctrl Pts',(1.2326244756697,-4.76141137004005,29.9929505025669));
#29384=CARTESIAN_POINT('Ctrl Pts',(1.15618681874447,-4.78062164076533,29.9884873932739));
#29385=CARTESIAN_POINT('Ctrl Pts',(1.11345844758248,-4.79075375889872,29.9860080816439));
#29386=CARTESIAN_POINT('Ctrl Pts',(1.06940890741174,-4.80057800062057,29.9834649708523));
#29387=CARTESIAN_POINT('Ctrl Pts',(1.0682179059898,-4.80084316101012,29.9833962204472));
#29388=CARTESIAN_POINT('Ctrl Pts',(1.06551327634014,-4.80144425400972,29.9832401178028));
#29389=CARTESIAN_POINT('Ctrl Pts',(1.06399958756485,-4.80177991416559,29.983152767958));
#29390=CARTESIAN_POINT('Ctrl Pts',(1.06055042317784,-4.802543054591,29.9829537633351));
#29391=CARTESIAN_POINT('Ctrl Pts',(1.05861484715097,-4.80297008076242,29.9828421124938));
#29392=CARTESIAN_POINT('Ctrl Pts',(1.05418707035387,-4.80394412888943,29.9825867594659));
#29393=CARTESIAN_POINT('Ctrl Pts',(1.05169470064238,-4.80449038186596,29.9824430638311));
#29394=CARTESIAN_POINT('Ctrl Pts',(0.989865462182989,-4.81799108663865,
29.9788793523748));
#29395=CARTESIAN_POINT('Ctrl Pts',(0.930293736296707,-4.82984734747352,
29.9754686546393));
#29396=CARTESIAN_POINT('Ctrl Pts',(0.682099650101073,-4.87448177055396,
29.9613234338234));
#29397=CARTESIAN_POINT('Ctrl Pts',(0.491864966075864,-4.89733611519763,
29.9506295299418));
#29398=CARTESIAN_POINT('Ctrl Pts',(0.21949888699607,-4.91402435211442,29.9352827515274));
#29399=CARTESIAN_POINT('Ctrl Pts',(0.13810357490624,-4.91698508066162,29.9306929577632));
#29400=CARTESIAN_POINT('Ctrl Pts',(0.0511315716101662,-4.91798732577079,
29.925776122007));
#29401=CARTESIAN_POINT('Ctrl Pts',(0.0455900380226175,-4.91804181787991,
29.9254627861361));
#29402=CARTESIAN_POINT('Ctrl Pts',(0.0334229200019035,-4.91814089582433,
29.9247746970467));
#29403=CARTESIAN_POINT('Ctrl Pts',(0.0267973150226865,-4.9181814592938,
29.9243999188639));
#29404=CARTESIAN_POINT('Ctrl Pts',(0.00912120295854194,-4.91825395650327,
29.9233998468002));
#29405=CARTESIAN_POINT('Ctrl Pts',(-0.00192935498148004,-4.9182620359225,
29.9227744026962));
#29406=CARTESIAN_POINT('Ctrl Pts',(-0.0584732946038119,-4.91811280938267,
29.9195728506077));
#29407=CARTESIAN_POINT('Ctrl Pts',(-0.103962664961447,-4.91736153388182,
29.9169930353557));
#29408=CARTESIAN_POINT('Ctrl Pts',(-0.217646920461575,-4.91390578558918,
29.9105331018305));
#29409=CARTESIAN_POINT('Ctrl Pts',(-0.285807983913625,-4.91041280562472,
29.9066485207759));
#29410=CARTESIAN_POINT('Ctrl Pts',(-0.463973274432121,-4.89756029486546,
29.8964604732729));
#29411=CARTESIAN_POINT('Ctrl Pts',(-0.573773468573468,-4.88591360358744,
29.8901469859518));
#29412=CARTESIAN_POINT('Ctrl Pts',(-0.824046138394972,-4.850813445637,29.8756805854009));
#29413=CARTESIAN_POINT('Ctrl Pts',(-0.964080927585995,-4.82493437621554,
29.8675300954511));
#29414=CARTESIAN_POINT('Ctrl Pts',(-1.14309058440367,-4.78374712213418,
29.8570756480477));
#29415=CARTESIAN_POINT('Ctrl Pts',(-1.18326632280902,-4.7739683156292,29.85472715603));
#29416=CARTESIAN_POINT('Ctrl Pts',(-1.25860896504974,-4.75462032132464,
29.8503209951568));
#29417=CARTESIAN_POINT('Ctrl Pts',(-1.29380206662514,-4.74516460995912,
29.8482619749614));
#29418=CARTESIAN_POINT('Ctrl Pts',(-1.33275660035233,-4.7342326790389,29.845980008386));
#29419=CARTESIAN_POINT('Ctrl Pts',(-1.33662481011624,-4.73314201478103,
29.8457533761171));
#29420=CARTESIAN_POINT('Ctrl Pts',(-1.34498948779896,-4.73077247327524,
29.8452632298105));
#29421=CARTESIAN_POINT('Ctrl Pts',(-1.34948547883623,-4.72949192394501,
29.8449997317813));
#29422=CARTESIAN_POINT('Ctrl Pts',(-1.35672287348843,-4.72741940697912,
29.8445754880534));
#29423=CARTESIAN_POINT('Ctrl Pts',(-1.35946542348374,-4.72663146091334,
29.8444147060849));
#29424=CARTESIAN_POINT('Ctrl Pts',(-1.36649066691624,-4.72460645889999,
29.8440028021501));
#29425=CARTESIAN_POINT('Ctrl Pts',(-1.37077236860935,-4.72336596589306,
29.8437517107176));
#29426=CARTESIAN_POINT('Ctrl Pts',(-1.38190360390953,-4.72012461820929,
29.843098813186));
#29427=CARTESIAN_POINT('Ctrl Pts',(-1.38875048394198,-4.71811467383661,
29.8426970848728));
#29428=CARTESIAN_POINT('Ctrl Pts',(-1.45985156396179,-4.69707432662595,
29.838523902809));
#29429=CARTESIAN_POINT('Ctrl Pts',(-1.52371520757566,-4.67674736271437,
29.8347630660861));
#29430=CARTESIAN_POINT('Ctrl Pts',(-1.79332549445003,-4.58482488576176,
29.818792431599));
#29431=CARTESIAN_POINT('Ctrl Pts',(-1.99460731550415,-4.50090836886034,
29.806623722021));
#29432=CARTESIAN_POINT('Ctrl Pts',(-2.24256082913721,-4.37762426311005,
29.7910140444091));
#29433=CARTESIAN_POINT('Ctrl Pts',(-2.2949821369226,-4.35037126747936,29.7876777714377));
#29434=CARTESIAN_POINT('Ctrl Pts',(-2.40213268175558,-4.29218963006874,
29.7807773661977));
#29435=CARTESIAN_POINT('Ctrl Pts',(-2.45678558507369,-4.26114277177896,
29.7772129157356));
#29436=CARTESIAN_POINT('Ctrl Pts',(-2.57248588014391,-4.19245050055632,
29.7695651184003));
#29437=CARTESIAN_POINT('Ctrl Pts',(-2.63333530200902,-4.15449995182853,
29.7654803060246));
#29438=CARTESIAN_POINT('Ctrl Pts',(-2.80064675331285,-4.04499814984928,
29.7540673346843));
#29439=CARTESIAN_POINT('Ctrl Pts',(-2.90517184214477,-3.97059296435249,
29.7467251352135));
#29440=CARTESIAN_POINT('Ctrl Pts',(-3.09281361627793,-3.82564195891981,
29.7331533973296));
#29441=CARTESIAN_POINT('Ctrl Pts',(-3.17672659235729,-3.75625358796593,
29.7269275545366));
#29442=CARTESIAN_POINT('Ctrl Pts',(-3.28965870601234,-3.65637589943658,
29.718345808016));
#29443=CARTESIAN_POINT('Ctrl Pts',(-3.32069309855417,-3.62821395717062,
29.7159652553322));
#29444=CARTESIAN_POINT('Ctrl Pts',(-3.35347088896619,-3.59769708924375,
29.7134281816362));
#29445=CARTESIAN_POINT('Ctrl Pts',(-3.35557604286721,-3.59573369003486,
29.7132651363252));
#29446=CARTESIAN_POINT('Ctrl Pts',(-3.38822643278234,-3.56522823433971,
29.7107347520871));
#29447=CARTESIAN_POINT('Ctrl Pts',(-3.41840850072128,-3.53629949211714,
29.7083739758083));
#29448=CARTESIAN_POINT('Ctrl Pts',(-3.45025032786775,-3.50499127797175,
29.7058571756585));
#29449=CARTESIAN_POINT('Ctrl Pts',(-3.45228062840131,-3.50299152816395,
29.7056965839487));
#29450=CARTESIAN_POINT('Ctrl Pts',(-3.46240967550334,-3.49299753779086,
29.7048948211928));
#29451=CARTESIAN_POINT('Ctrl Pts',(-3.47048240991077,-3.48497695879883,
29.7042539703571));
#29452=CARTESIAN_POINT('Ctrl Pts',(-3.51240214971891,-3.44303794267927,
29.7009162286683));
#29453=CARTESIAN_POINT('Ctrl Pts',(-3.5457801345098,-3.40865404806003,29.6982245705546));
#29454=CARTESIAN_POINT('Ctrl Pts',(-3.68739863510194,-3.25843620557217,
29.6866401274311));
#29455=CARTESIAN_POINT('Ctrl Pts',(-3.79050595290947,-3.13789418341467,
29.6777796324722));
#29456=CARTESIAN_POINT('Ctrl Pts',(-3.9486059775107,-2.93387280179996,29.6632921670813));
#29457=CARTESIAN_POINT('Ctrl Pts',(-4.00719539490756,-2.85332849633604,
29.6576922071448));
#29458=CARTESIAN_POINT('Ctrl Pts',(-4.08910679468821,-2.73321913042239,
29.6494865026446));
#29459=CARTESIAN_POINT('Ctrl Pts',(-4.1143845920288,-2.69501773285806,29.6468973165264));
#29460=CARTESIAN_POINT('Ctrl Pts',(-4.14810390777172,-2.64247864418189,
29.6433626446547));
#29461=CARTESIAN_POINT('Ctrl Pts',(-4.15701185161429,-2.62844286187267,
29.6424208796467));
#29462=CARTESIAN_POINT('Ctrl Pts',(-4.20755422117715,-2.54790625883081,
29.6370311783321));
#29463=CARTESIAN_POINT('Ctrl Pts',(-4.24766344702677,-2.48046242978804,
29.6325721896692));
#29464=CARTESIAN_POINT('Ctrl Pts',(-4.3317425213843,-2.33105878309729,29.6228046503494));
#29465=CARTESIAN_POINT('Ctrl Pts',(-4.37503593334096,-2.24875269162539,
29.6174934452591));
#29466=CARTESIAN_POINT('Ctrl Pts',(-4.49794751591431,-1.99808004554011,
29.601522019668));
#29467=CARTESIAN_POINT('Ctrl Pts',(-4.57036468051255,-1.82636889336943,
29.5908457800909));
#29468=CARTESIAN_POINT('Ctrl Pts',(-4.64467458684734,-1.61784344218231,
29.5782559940762));
#29469=CARTESIAN_POINT('Ctrl Pts',(-4.65612234394557,-1.584595904262,29.5762599249588));
#29470=CARTESIAN_POINT('Ctrl Pts',(-4.67449806939939,-1.5293084754238,29.5729603718675));
#29471=CARTESIAN_POINT('Ctrl Pts',(-4.68162898859386,-1.50733759874811,
29.5716542142019));
#29472=CARTESIAN_POINT('Ctrl Pts',(-4.70948606665194,-1.41940295962438,
29.5664449569709));
#29473=CARTESIAN_POINT('Ctrl Pts',(-4.72897514321561,-1.35305507856757,
29.5625556342458));
#29474=CARTESIAN_POINT('Ctrl Pts',(-4.81388319122366,-1.03970832326431,
29.5443271335567));
#29475=CARTESIAN_POINT('Ctrl Pts',(-4.86138849432607,-0.788267845529706,
29.5300833764657));
#29476=CARTESIAN_POINT('Ctrl Pts',(-4.89654818846978,-0.466523700483106,
29.5118331429605));
#29477=CARTESIAN_POINT('Ctrl Pts',(-4.90254299392909,-0.398623358220403,
29.507981847529));
#29478=CARTESIAN_POINT('Ctrl Pts',(-4.91059576867979,-0.279102874042,29.5011959178355));
#29479=CARTESIAN_POINT('Ctrl Pts',(-4.91325529364975,-0.227533683441403,
29.4982658407896));
#29480=CARTESIAN_POINT('Ctrl Pts',(-4.91720189917998,-0.117275649014002,
29.4919940337311));
#29481=CARTESIAN_POINT('Ctrl Pts',(-4.91825128049374,-0.0585862957523841,
29.4886512846965));
#29482=CARTESIAN_POINT('Ctrl Pts',(-4.91824999882741,0.000107397491747315,
29.4853030582774));
#29483=CARTESIAN_POINT('Ctrl Pts',(-4.91824999882813,0.000107364256212508,
29.4853030601734));
#29484=CARTESIAN_POINT('Ctrl Pts',(-4.91824536563938,0.212349141886051,
29.4731955663798));
#29485=CARTESIAN_POINT('Ctrl Pts',(-4.90450219779015,0.424366907549726,
29.4610215256331));
#29486=CARTESIAN_POINT('Ctrl Pts',(-4.8713386361668,0.679146533038959,29.446355223248));
#29487=CARTESIAN_POINT('Ctrl Pts',(-4.86496664387682,0.723380759594618,
29.4438080300108));
#29488=CARTESIAN_POINT('Ctrl Pts',(-4.85290081965428,0.799750775122579,
29.4394109504458));
#29489=CARTESIAN_POINT('Ctrl Pts',(-4.84748836227862,0.831928044753747,
29.4375585114712));
#29490=CARTESIAN_POINT('Ctrl Pts',(-4.83441170691769,0.905203931302206,
29.433341770966));
#29491=CARTESIAN_POINT('Ctrl Pts',(-4.82654285598595,0.946263611344807,
29.4309802071808));
#29492=CARTESIAN_POINT('Ctrl Pts',(-4.80203008909085,1.06589898087157,29.4240954527912));
#29493=CARTESIAN_POINT('Ctrl Pts',(-4.78398537213812,1.14416571360072,29.4195863166346));
#29494=CARTESIAN_POINT('Ctrl Pts',(-4.76403458343061,1.22194826010642,29.4150832822139));
#29495=CARTESIAN_POINT('',(-4.91824999938284,-7.79148190512436E-5,29.1398594360263));
#29496=CARTESIAN_POINT('Ctrl Pts',(-4.76403458843593,1.2219482405921,29.0701077704777));
#29497=CARTESIAN_POINT('Ctrl Pts',(-4.802042410005,1.07376636956748,29.0787010901888));
#29498=CARTESIAN_POINT('Ctrl Pts',(-4.83311838314403,0.923882229251823,
29.0872522276148));
#29499=CARTESIAN_POINT('Ctrl Pts',(-4.87533993350278,0.658508237472935,
29.1023205217532));
#29500=CARTESIAN_POINT('Ctrl Pts',(-4.88948270101306,0.543627632427015,
29.1088198289951));
#29501=CARTESIAN_POINT('Ctrl Pts',(-4.90547693217398,0.360684861074001,
29.119178406903));
#29502=CARTESIAN_POINT('Ctrl Pts',(-4.90999061135142,0.292898552021269,
29.1230182534322));
#29503=CARTESIAN_POINT('Ctrl Pts',(-4.91653386527548,0.150046150226172,
29.131121967292));
#29504=CARTESIAN_POINT('Ctrl Pts',(-4.91825135989444,0.0749831078358474,
29.1353869217918));
#29505=CARTESIAN_POINT('Ctrl Pts',(-4.91824999919212,-8.91444442064763E-5,
29.1396622504236));
#29506=CARTESIAN_POINT('Ctrl Pts',(-4.91824999938284,-7.79148190512436E-5,
29.1398594360263));
#29507=CARTESIAN_POINT('Ctrl Pts',(-4.91824765848413,-0.147843451538412,
29.1482253307768));
#29508=CARTESIAN_POINT('Ctrl Pts',(-4.91158170501074,-0.295582196842949,
29.1565912255273));
#29509=CARTESIAN_POINT('Ctrl Pts',(-4.89828533696788,-0.442700598763389,
29.1649571202777));
#29510=CARTESIAN_POINT('Ctrl Pts',(-4.88498458454875,-0.589867511858225,
29.1733257736184));
#29511=CARTESIAN_POINT('Ctrl Pts',(-4.86504907810585,-0.736413378442218,
29.1816944269591));
#29512=CARTESIAN_POINT('Ctrl Pts',(-4.83856387762818,-0.881749774375791,
29.1900630802997));
#29513=CARTESIAN_POINT('Ctrl Pts',(-4.83420068304682,-0.905692616558404,
29.1914417394094));
#29514=CARTESIAN_POINT('Ctrl Pts',(-4.829659845967,-0.929602652504876,29.192820398519));
#29515=CARTESIAN_POINT('Ctrl Pts',(-4.82494188036517,-0.953477274820037,
29.1941990576287));
#29516=CARTESIAN_POINT('Ctrl Pts',(-4.79702989473963,-1.09472207631175,
29.2023553513574));
#29517=CARTESIAN_POINT('Ctrl Pts',(-4.76290624681523,-1.23476683647118,
29.2105116450862));
#29518=CARTESIAN_POINT('Ctrl Pts',(-4.7226989765346,-1.3730613385931,29.218667938815));
#29519=CARTESIAN_POINT('Ctrl Pts',(-4.6824999011205,-1.51132765414629,29.2268225701644));
#29520=CARTESIAN_POINT('Ctrl Pts',(-4.63621977031956,-1.64784410216371,
29.2349772015138));
#29521=CARTESIAN_POINT('Ctrl Pts',(-4.58403679062399,-1.78207456766143,
29.2431318328631));
#29522=CARTESIAN_POINT('Ctrl Pts',(-4.53185195965433,-1.91630979519814,
29.251286753511));
#29523=CARTESIAN_POINT('Ctrl Pts',(-4.47376397850035,-2.04825856467408,
29.2594416741589));
#29524=CARTESIAN_POINT('Ctrl Pts',(-4.40999979152046,-2.17740324728552,
29.2675965948068));
#29525=CARTESIAN_POINT('Ctrl Pts',(-4.34623935342989,-2.30654033709063,
29.2757510360022));
#29526=CARTESIAN_POINT('Ctrl Pts',(-4.27680352617805,-2.43287337019581,
29.2839054771976));
#29527=CARTESIAN_POINT('Ctrl Pts',(-4.20196592304876,-2.55590794905391,
29.2920599183931));
#29528=CARTESIAN_POINT('Ctrl Pts',(-4.12710987323732,-2.67897285464183,
29.3002163695725));
#29529=CARTESIAN_POINT('Ctrl Pts',(-4.04684956074285,-2.79873739519221,
29.3083728207519));
#29530=CARTESIAN_POINT('Ctrl Pts',(-3.96150309315888,-2.91473434559526,
29.3165292719314));
#29531=CARTESIAN_POINT('Ctrl Pts',(-3.90329093529433,-2.99385223974859,
29.3220925323347));
#29532=CARTESIAN_POINT('Ctrl Pts',(-3.84271352873989,-3.07121795879998,
29.327655792738));
#29533=CARTESIAN_POINT('Ctrl Pts',(-3.77988294458199,-3.14669159400126,
29.3332190531413));
#29534=CARTESIAN_POINT('Ctrl Pts',(-3.68776705167079,-3.25734345871013,
29.3413753468701));
#29535=CARTESIAN_POINT('Ctrl Pts',(-3.59077176250648,-3.36396837172811,
29.349531640599));
#29536=CARTESIAN_POINT('Ctrl Pts',(-3.48927286645023,-3.46614453333299,
29.3576879343279));
#29537=CARTESIAN_POINT('Ctrl Pts',(-3.38779465744623,-3.56829986984838,
29.3658425656773));
#29538=CARTESIAN_POINT('Ctrl Pts',(-3.28181490841962,-3.66600802653415,
29.3739971970268));
#29539=CARTESIAN_POINT('Ctrl Pts',(-3.17174670474582,-3.75888359801604,
29.3821518283762));
#29540=CARTESIAN_POINT('Ctrl Pts',(-3.06167459622795,-3.85176246440612,
29.3903067490242));
#29541=CARTESIAN_POINT('Ctrl Pts',(-2.94751399615763,-3.93980818385149,
29.3984616696721));
#29542=CARTESIAN_POINT('Ctrl Pts',(-2.82971193284848,-4.02267491100075,
29.40661659032));
#29543=CARTESIAN_POINT('Ctrl Pts',(-2.71191679547886,-4.10553676616454,
29.4147710315155));
#29544=CARTESIAN_POINT('Ctrl Pts',(-2.59048089746017,-4.18322004642729,
29.422925472711));
#29545=CARTESIAN_POINT('Ctrl Pts',(-2.4658811222088,-4.25542164228579,29.4310799139065));
#29546=CARTESIAN_POINT('Ctrl Pts',(-2.34125063442296,-4.32764103507849,
29.439236365086));
#29547=CARTESIAN_POINT('Ctrl Pts',(-2.21345500063114,-4.3943758754473,29.4473928162655));
#29548=CARTESIAN_POINT('Ctrl Pts',(-2.08299716353332,-4.45536820916208,
29.455549267445));
#29549=CARTESIAN_POINT('Ctrl Pts',(-1.99401595057698,-4.49696917354807,
29.4611125278479));
#29550=CARTESIAN_POINT('Ctrl Pts',(-1.90379676687354,-4.53589956732471,
29.4666757882507));
#29551=CARTESIAN_POINT('Ctrl Pts',(-1.81250498017415,-4.57209019588895,
29.4722390486536));
#29552=CARTESIAN_POINT('Ctrl Pts',(-1.67866213022207,-4.62514926115345,
29.4803953423824));
#29553=CARTESIAN_POINT('Ctrl Pts',(-1.54246275836423,-4.67233706997473,
29.4885516361112));
#29554=CARTESIAN_POINT('Ctrl Pts',(-1.40443870803326,-4.71346316182463,
29.49670792984));
#29555=CARTESIAN_POINT('Ctrl Pts',(-1.26644278914871,-4.7545808715379,29.5048625611894));
#29556=CARTESIAN_POINT('Ctrl Pts',(-1.1266232542291,-4.78963923346716,29.5130171925388));
#29557=CARTESIAN_POINT('Ctrl Pts',(-0.985527271686252,-4.81849759357236,
29.5211718238881));
#29558=CARTESIAN_POINT('Ctrl Pts',(-0.844426283539492,-4.84735697747369,
29.529326744536));
#29559=CARTESIAN_POINT('Ctrl Pts',(-0.70204908425379,-4.87001584867918,
29.5374816651839));
#29560=CARTESIAN_POINT('Ctrl Pts',(-0.558953707926475,-4.8863845340799,
29.5456365858317));
#29561=CARTESIAN_POINT('Ctrl Pts',(-0.415866744608908,-4.90275225711612,
29.5537910270272));
#29562=CARTESIAN_POINT('Ctrl Pts',(-0.272062021327598,-4.91283049712567,
29.5619454682226));
#29563=CARTESIAN_POINT('Ctrl Pts',(-0.128103328596984,-4.91658139358054,
29.570099909418));
#29564=CARTESIAN_POINT('Ctrl Pts',(0.0158908484375917,-4.92033321459194,
29.5782563605975));
#29565=CARTESIAN_POINT('Ctrl Pts',(0.160038736072495,-4.9177545666176,29.5864128117769));
#29566=CARTESIAN_POINT('Ctrl Pts',(0.303775278191233,-4.90885970902203,
29.5945692629564));
#29567=CARTESIAN_POINT('Ctrl Pts',(0.401813480797395,-4.90279280468265,
29.6001325233597));
#29568=CARTESIAN_POINT('Ctrl Pts',(0.499660302309726,-4.89378857294753,
29.605695783763));
#29569=CARTESIAN_POINT('Ctrl Pts',(0.597137429250602,-4.88186541734694,
29.6112590441663));
#29570=CARTESIAN_POINT('Ctrl Pts',(0.740048603910757,-4.864384883954,29.6194153378952));
#29571=CARTESIAN_POINT('Ctrl Pts',(0.882218417583596,-4.84062141879297,
29.627571631624));
#29572=CARTESIAN_POINT('Ctrl Pts',(1.02308874644461,-4.81066237428884,29.6357279253529));
#29573=CARTESIAN_POINT('Ctrl Pts',(1.16393036374331,-4.78070943590359,29.6438825567024));
#29574=CARTESIAN_POINT('Ctrl Pts',(1.30347269746603,-4.74456350686749,29.6520371880518));
#29575=CARTESIAN_POINT('Ctrl Pts',(1.44116800925092,-4.7023630050871,29.6601918194013));
#29576=CARTESIAN_POINT('Ctrl Pts',(1.57886820599569,-4.66016100617688,29.6683467400492));
#29577=CARTESIAN_POINT('Ctrl Pts',(1.71472092863266,-4.61190409917613,29.6765016606972));
#29578=CARTESIAN_POINT('Ctrl Pts',(1.84819330167373,-4.55778066411147,29.6846565813451));
#29579=CARTESIAN_POINT('Ctrl Pts',(1.98165782747046,-4.50366041112719,29.6928110225406));
#29580=CARTESIAN_POINT('Ctrl Pts',(2.11274197387535,-4.44367444675716,29.7009654637361));
#29581=CARTESIAN_POINT('Ctrl Pts',(2.24093261227665,-4.3780593976938,29.7091199049317));
#29582=CARTESIAN_POINT('Ctrl Pts',(2.36915484832234,-4.3124281752108,29.7172763561112));
#29583=CARTESIAN_POINT('Ctrl Pts',(2.49448185305424,-4.24116524781992,29.7254328072907));
#29584=CARTESIAN_POINT('Ctrl Pts',(2.61642433475618,-4.16455360909134,29.7335892584702));
#29585=CARTESIAN_POINT('Ctrl Pts',(2.69959748996079,-4.11229920496967,29.739152518873));
#29586=CARTESIAN_POINT('Ctrl Pts',(2.78119661061453,-4.05755744599145,29.7447157792758));
#29587=CARTESIAN_POINT('Ctrl Pts',(2.86107394730348,-4.00042984322451,29.7502790396786));
#29588=CARTESIAN_POINT('Ctrl Pts',(2.97818207691382,-3.91667508891653,29.7584353334074));
#29589=CARTESIAN_POINT('Ctrl Pts',(3.0916318601361,-3.82775880872764,29.7665916271362));
#29590=CARTESIAN_POINT('Ctrl Pts',(3.20097507904098,-3.73402485340666,29.774747920865));
#29591=CARTESIAN_POINT('Ctrl Pts',(3.31029601209859,-3.64031000252245,29.7829025522144));
#29592=CARTESIAN_POINT('Ctrl Pts',(3.41551179664554,-3.54177965304348,29.7910571835638));
#29593=CARTESIAN_POINT('Ctrl Pts',(3.51620777652833,-3.43881751984337,29.7992118149132));
#29594=CARTESIAN_POINT('Ctrl Pts',(3.61690732876088,-3.33585173389811,29.807366735561));
#29595=CARTESIAN_POINT('Ctrl Pts',(3.71308651880639,-3.22845408623791,29.8155216562089));
#29596=CARTESIAN_POINT('Ctrl Pts',(3.80436765529465,-3.11704504392347,29.8236765768568));
#29597=CARTESIAN_POINT('Ctrl Pts',(3.8956434250889,-3.00564255168349,29.8318310180522));
#29598=CARTESIAN_POINT('Ctrl Pts',(3.98202150608234,-2.89022939609205,29.8399854592477));
#29599=CARTESIAN_POINT('Ctrl Pts',(4.06316463869261,-2.7712589524218,29.8481399004431));
#29600=CARTESIAN_POINT('Ctrl Pts',(4.14432777223184,-2.65225918378817,29.8562963516225));
#29601=CARTESIAN_POINT('Ctrl Pts',(4.22025319011674,-2.52970065142921,29.864452802802));
#29602=CARTESIAN_POINT('Ctrl Pts',(4.29064675578168,-2.40406603062398,29.8726092539814));
#29603=CARTESIAN_POINT('Ctrl Pts',(4.33866000663017,-2.31837458273388,29.8781725143847));
#29604=CARTESIAN_POINT('Ctrl Pts',(4.38410064538988,-2.23125268526632,29.883735774788));
#29605=CARTESIAN_POINT('Ctrl Pts',(4.42688753864598,-2.1428601873853,29.8892990351913));
#29606=CARTESIAN_POINT('Ctrl Pts',(4.48961738478709,-2.01326798355508,29.8974553289202));
#29607=CARTESIAN_POINT('Ctrl Pts',(4.54666456236093,-1.88089510972097,29.9056116226491));
#29608=CARTESIAN_POINT('Ctrl Pts',(4.59780012777975,-1.74625801286308,29.913767916378));
#29609=CARTESIAN_POINT('Ctrl Pts',(4.64892527097563,-1.61164835713792,29.9219225477274));
#29610=CARTESIAN_POINT('Ctrl Pts',(4.69414108692694,-1.47477571168039,29.9300771790769));
#29611=CARTESIAN_POINT('Ctrl Pts',(4.73326718081661,-1.33617545910121,29.9382318104263));
#29612=CARTESIAN_POINT('Ctrl Pts',(4.77239466276659,-1.19757028945801,29.9463867310743));
#29613=CARTESIAN_POINT('Ctrl Pts',(4.8054318958188,-1.05723771108288,29.9545416517222));
#29614=CARTESIAN_POINT('Ctrl Pts',(4.83224853217211,-0.915727681038694,
29.9626965723702));
#29615=CARTESIAN_POINT('Ctrl Pts',(4.85906359189428,-0.774225970797069,
29.9708510135657));
#29616=CARTESIAN_POINT('Ctrl Pts',(4.87965872522313,-0.631547276370576,
29.9790054547612));
#29617=CARTESIAN_POINT('Ctrl Pts',(4.89395483540549,-0.488251094736334,
29.9871598959567));
#29618=CARTESIAN_POINT('Ctrl Pts',(4.90825446942869,-0.344919592100032,
29.9953163471362));
#29619=CARTESIAN_POINT('Ctrl Pts',(4.91625194430766,-0.200970631246002,
30.0034727983157));
#29620=CARTESIAN_POINT('Ctrl Pts',(4.91792005009626,-0.0569687928709609,
30.0116292494952));
#29621=CARTESIAN_POINT('Ctrl Pts',(4.91905781291457,0.0412503600095018,
30.017192509898));
#29622=CARTESIAN_POINT('Ctrl Pts',(4.91725212223471,0.139494017049788,30.0227557703008));
#29623=CARTESIAN_POINT('Ctrl Pts',(4.91250825778637,0.237582995352652,30.0283190307037));
#29624=CARTESIAN_POINT('Ctrl Pts',(4.90555328012063,0.381391205047743,30.0364753244324));
#29625=CARTESIAN_POINT('Ctrl Pts',(4.89227792431803,0.524920725092011,30.0446316181612));
#29626=CARTESIAN_POINT('Ctrl Pts',(4.87272838503889,0.667608529106876,30.05278791189));
#29627=CARTESIAN_POINT('Ctrl Pts',(4.85318283025969,0.81026725112974,30.0609425432394));
#29628=CARTESIAN_POINT('Ctrl Pts',(4.8273656884833,0.952084268009815,30.0690971745888));
#29629=CARTESIAN_POINT('Ctrl Pts',(4.79537484388121,1.09250316666418,30.0772518059382));
#29630=CARTESIAN_POINT('Ctrl Pts',(4.76338286435311,1.23292704690194,30.085406726586));
#29631=CARTESIAN_POINT('Ctrl Pts',(4.72521681440178,1.3719523825493,30.0935616472339));
#29632=CARTESIAN_POINT('Ctrl Pts',(4.68102549561008,1.50903392007881,30.1017165678818));
#29633=CARTESIAN_POINT('Ctrl Pts',(4.63683677495964,1.6461073981702,30.1098710090772));
#29634=CARTESIAN_POINT('Ctrl Pts',(4.58662359776409,1.78123698854771,30.1180254502726));
#29635=CARTESIAN_POINT('Ctrl Pts',(4.53058433028458,1.91389359387606,30.1261798914681));
#29636=CARTESIAN_POINT('Ctrl Pts',(4.47453124971487,2.04658289766279,30.1343363426475));
#29637=CARTESIAN_POINT('Ctrl Pts',(4.41264933934322,2.17679768984758,30.1424927938269));
#29638=CARTESIAN_POINT('Ctrl Pts',(4.34518495526843,2.30402924612707,30.1506492450064));
#29639=CARTESIAN_POINT('Ctrl Pts',(4.2991696076251,2.39080991378888,30.1562125054097));
#29640=CARTESIAN_POINT('Ctrl Pts',(4.25055818921169,2.47620316099904,30.161775765813));
#29641=CARTESIAN_POINT('Ctrl Pts',(4.19944110460985,2.56005419306179,30.1673390262164));
#29642=CARTESIAN_POINT('Ctrl Pts',(4.12449836845348,2.68298815577239,30.1754953199452));
#29643=CARTESIAN_POINT('Ctrl Pts',(4.04413976298961,2.80265207148643,30.1836516136741));
#29644=CARTESIAN_POINT('Ctrl Pts',(3.95867534929238,2.91857371697288,30.1918079074029));
#29645=CARTESIAN_POINT('Ctrl Pts',(3.87322835457088,3.03447173582639,30.1999625387523));
#29646=CARTESIAN_POINT('Ctrl Pts',(3.78267782610433,3.14662873686053,30.2081171701018));
#29647=CARTESIAN_POINT('Ctrl Pts',(3.68737604260045,3.25460304537378,30.2162718014512));
#29648=CARTESIAN_POINT('Ctrl Pts',(3.59207087811443,3.3625811844471,30.2244267220991));
#29649=CARTESIAN_POINT('Ctrl Pts',(3.49201433992864,3.46637608069595,30.2325816427471));
#29650=CARTESIAN_POINT('Ctrl Pts',(3.38759807033757,3.56558022996892,30.240736563395));
#29651=CARTESIAN_POINT('Ctrl Pts',(3.28318793969473,3.66477854672996,30.2488910045905));
#29652=CARTESIAN_POINT('Ctrl Pts',(3.17441883372558,3.75938642666932,30.257045445786));
#29653=CARTESIAN_POINT('Ctrl Pts',(3.06171817888996,3.84903427570537,30.2651998869814));
#29654=CARTESIAN_POINT('Ctrl Pts',(2.94898974452789,3.93870422199363,30.2733563381609));
#29655=CARTESIAN_POINT('Ctrl Pts',(2.83232808672348,4.02341148575304,30.2815127893404));
#29656=CARTESIAN_POINT('Ctrl Pts',(2.71219301493423,4.10282733151688,30.2896692405199));
#29657=CARTESIAN_POINT('Ctrl Pts',(2.63025263753481,4.15699439760729,30.2952325009229));
#29658=CARTESIAN_POINT('Ctrl Pts',(2.54669703231131,4.20870065935219,30.3007957613258));
#29659=CARTESIAN_POINT('Ctrl Pts',(2.46167966931954,4.25785348129299,30.3063590217287));
#29660=CARTESIAN_POINT('Ctrl Pts',(2.33703574931766,4.32991641279615,30.3145153154575));
#29661=CARTESIAN_POINT('Ctrl Pts',(2.20920198048032,4.39651585529299,30.3226716091864));
#29662=CARTESIAN_POINT('Ctrl Pts',(2.07867663313013,4.45738561461523,30.3308279029152));
#29663=CARTESIAN_POINT('Ctrl Pts',(1.9481778888743,4.51824296773451,30.3389825342646));
#29664=CARTESIAN_POINT('Ctrl Pts',(1.81498896361117,4.57337282601228,30.3471371656141));
#29665=CARTESIAN_POINT('Ctrl Pts',(1.67963057200864,4.62255602497946,30.3552917969635));
#29666=CARTESIAN_POINT('Ctrl Pts',(1.5442673783522,4.67174096879874,30.3634467176114));
#29667=CARTESIAN_POINT('Ctrl Pts',(1.40673487758352,4.71497871334307,30.3716016382593));
#29668=CARTESIAN_POINT('Ctrl Pts',(1.26757198913018,4.75209893782448,30.3797565589072));
#29669=CARTESIAN_POINT('Ctrl Pts',(1.1284172824838,4.78921697989566,30.3879110001027));
#29670=CARTESIAN_POINT('Ctrl Pts',(0.987632703526648,4.82021813612847,30.3960654412981));
#29671=CARTESIAN_POINT('Ctrl Pts',(0.845770443741198,4.84498249934856,30.4042198824936));
#29672=CARTESIAN_POINT('Ctrl Pts',(0.703873216400462,4.86975296672378,30.4123763336731));
#29673=CARTESIAN_POINT('Ctrl Pts',(0.56089810720643,4.88828351140401,30.4205327848526));
#29674=CARTESIAN_POINT('Ctrl Pts',(0.417406182111368,4.90050560061257,30.4286892360321));
#29675=CARTESIAN_POINT('Ctrl Pts',(0.319534825135521,4.90884190563552,30.4342524964351));
#29676=CARTESIAN_POINT('Ctrl Pts',(0.221423210660194,4.91424447664097,30.4398157568382));
#29677=CARTESIAN_POINT('Ctrl Pts',(0.123250426401515,4.91670544113554,30.4453790172413));
#29678=CARTESIAN_POINT('Ctrl Pts',(-0.0206806511637789,4.92031346014232,
30.4535353109701));
#29679=CARTESIAN_POINT('Ctrl Pts',(-0.164797210693284,4.91759767932967,
30.461691604699));
#29680=CARTESIAN_POINT('Ctrl Pts',(-0.308534354211583,4.90856288691214,
30.4698478984278));
#29681=CARTESIAN_POINT('Ctrl Pts',(-0.452242201866507,4.8995299359257,30.4780025297772));
#29682=CARTESIAN_POINT('Ctrl Pts',(-0.595570453989007,4.88418056362306,
30.4861571611267));
#29683=CARTESIAN_POINT('Ctrl Pts',(-0.737957018130757,4.86257159349778,
30.4943117924761));
#29684=CARTESIAN_POINT('Ctrl Pts',(-0.88034863366171,4.84096185676001,30.502466713124));
#29685=CARTESIAN_POINT('Ctrl Pts',(-1.02179816294776,4.81309212432972,30.5106216337719));
#29686=CARTESIAN_POINT('Ctrl Pts',(-1.16175090970224,4.77907081829784,30.5187765544199));
#29687=CARTESIAN_POINT('Ctrl Pts',(-1.30169542821143,4.74505151248145,30.5269309956153));
#29688=CARTESIAN_POINT('Ctrl Pts',(-1.44014301527523,4.70488143660295,30.5350854368108));
#29689=CARTESIAN_POINT('Ctrl Pts',(-1.57655145314084,4.6587196286211,30.5432398780063));
#29690=CARTESIAN_POINT('Ctrl Pts',(-1.71299351425211,4.61254644223895,30.5513963291857));
#29691=CARTESIAN_POINT('Ctrl Pts',(-1.84739510458777,4.56037867967971,30.5595527803652));
#29692=CARTESIAN_POINT('Ctrl Pts',(-1.97923080588844,4.50242473335449,30.5677092315447));
#29693=CARTESIAN_POINT('Ctrl Pts',(-2.06915181695286,4.46289615803442,30.5732724919478));
#29694=CARTESIAN_POINT('Ctrl Pts',(-2.15787949060853,4.42067677153921,30.5788357523508));
#29695=CARTESIAN_POINT('Ctrl Pts',(-2.24525282018892,4.37584538528656,30.5843990127539));
#29696=CARTESIAN_POINT('Ctrl Pts',(-2.37335082180918,4.31011810882348,30.5925553064828));
#29697=CARTESIAN_POINT('Ctrl Pts',(-2.49858467956924,4.23874977504249,30.6007116002116));
#29698=CARTESIAN_POINT('Ctrl Pts',(-2.62046070707022,4.1620149861817,30.6088678939405));
#29699=CARTESIAN_POINT('Ctrl Pts',(-2.7423118943428,4.08529583706336,30.6170225252899));
#29700=CARTESIAN_POINT('Ctrl Pts',(-2.86080633362388,4.00321259306017,30.6251771566394));
#29701=CARTESIAN_POINT('Ctrl Pts',(-2.97547770934493,3.91608420028113,30.6333317879888));
#29702=CARTESIAN_POINT('Ctrl Pts',(-3.09015315321498,3.8289527164841,30.6414867086368));
#29703=CARTESIAN_POINT('Ctrl Pts',(-3.20100499340322,3.73677592521895,30.6496416292847));
#29704=CARTESIAN_POINT('Ctrl Pts',(-3.30759810670668,3.63991453567393,30.6577965499326));
#29705=CARTESIAN_POINT('Ctrl Pts',(-3.41418495307859,3.54305884090299,30.6659509911281));
#29706=CARTESIAN_POINT('Ctrl Pts',(-3.51651332644803,3.4415193246371,30.6741054323236));
#29707=CARTESIAN_POINT('Ctrl Pts',(-3.61418328788132,3.33569516354528,30.6822598735191));
#29708=CARTESIAN_POINT('Ctrl Pts',(-3.71187732393316,3.22984491791044,30.6904163246986));
#29709=CARTESIAN_POINT('Ctrl Pts',(-3.80491042634352,3.11970816295925,30.6985727758781));
#29710=CARTESIAN_POINT('Ctrl Pts',(-3.89292103043636,3.00571936702119,30.7067292270576));
#29711=CARTESIAN_POINT('Ctrl Pts',(-3.95295031253593,2.92797117226574,30.7122924874605));
#29712=CARTESIAN_POINT('Ctrl Pts',(-4.01064384535679,2.84843166674513,30.7178557478634));
#29713=CARTESIAN_POINT('Ctrl Pts',(-4.06589799008391,2.76724711522691,30.7234190082663));
#29714=CARTESIAN_POINT('Ctrl Pts',(-4.14691033137735,2.64821621486946,30.7315757312179));
#29715=CARTESIAN_POINT('Ctrl Pts',(-4.22270722572797,2.52560308161383,30.7397324541694));
#29716=CARTESIAN_POINT('Ctrl Pts',(-4.29298661487559,2.39988520287929,30.747889177121));
#29717=CARTESIAN_POINT('Ctrl Pts',(-4.36324999464958,2.27419596219239,30.7560440420025));
#29718=CARTESIAN_POINT('Ctrl Pts',(-4.42799821415893,2.14540367937789,30.7641989068841));
#29719=CARTESIAN_POINT('Ctrl Pts',(-4.48697450016212,2.01401164281514,30.7723537717656));
#29720=CARTESIAN_POINT('Ctrl Pts',(-4.54595262536498,1.88261550873781,30.78050889096));
#29721=CARTESIAN_POINT('Ctrl Pts',(-4.59915831640787,1.74861976248036,30.7886640101543));
#29722=CARTESIAN_POINT('Ctrl Pts',(-4.64638218564289,1.61254942480544,30.7968191293487));
#29723=CARTESIAN_POINT('Ctrl Pts',(-4.69097963986471,1.48404681047704,30.8045206913095));
#29724=CARTESIAN_POINT('Ctrl Pts',(-4.73024244860134,1.35369434642745,30.8122222532703));
#29725=CARTESIAN_POINT('Ctrl Pts',(-4.76403458704967,1.22194824599672,30.8199238152312));
#29726=CARTESIAN_POINT('Origin',(0.,0.,-3.23514056400928));
#29727=CARTESIAN_POINT('',(-4.76403458699526,1.22194824620887,32.9149784811847));
#29728=CARTESIAN_POINT('',(-4.7639087307945,1.22191632179108,32.5699348864137));
#29729=CARTESIAN_POINT('',(-4.76403458704967,1.22194824599672,-3.23514056400928));
#29730=CARTESIAN_POINT('Ctrl Pts',(-4.76403458699526,1.22194824620887,32.9149784811847));
#29731=CARTESIAN_POINT('Ctrl Pts',(-4.76018292856304,1.23696478561248,32.914096809347));
#29732=CARTESIAN_POINT('Ctrl Pts',(-4.75626023845671,1.25196323894184,32.913215832861));
#29733=CARTESIAN_POINT('Ctrl Pts',(-4.74299936564893,1.30170438629748,32.9102931210259));
#29734=CARTESIAN_POINT('Ctrl Pts',(-4.73335096376061,1.33636296809984,32.9082552859967));
#29735=CARTESIAN_POINT('Ctrl Pts',(-4.70648053371979,1.42894194166121,32.9028069210402));
#29736=CARTESIAN_POINT('Ctrl Pts',(-4.68856992295052,1.48665607831358,32.8994042528157));
#29737=CARTESIAN_POINT('Ctrl Pts',(-4.61433833648949,1.71115478318329,32.886114885965));
#29738=CARTESIAN_POINT('Ctrl Pts',(-4.55014354245029,1.87519686592309,32.8762831571679));
#29739=CARTESIAN_POINT('Ctrl Pts',(-4.4445569498971,2.10745185009664,32.8619688464675));
#29740=CARTESIAN_POINT('Ctrl Pts',(-4.41008908127384,2.17865874367186,32.8575247823227));
#29741=CARTESIAN_POINT('Ctrl Pts',(-4.34517185633154,2.30491144609587,32.8495277519827));
#29742=CARTESIAN_POINT('Ctrl Pts',(-4.31535542122827,2.36026327349465,32.8459798651798));
#29743=CARTESIAN_POINT('Ctrl Pts',(-4.25255231288962,2.47168188483448,32.8387452102819));
#29744=CARTESIAN_POINT('Ctrl Pts',(-4.21949797038691,2.52769643564737,32.835058580705));
#29745=CARTESIAN_POINT('Ctrl Pts',(-4.12707306785472,2.67745412836762,32.8250596862963));
#29746=CARTESIAN_POINT('Ctrl Pts',(-4.06562578694426,2.76986988618575,32.8187336113795));
#29747=CARTESIAN_POINT('Ctrl Pts',(-3.89306218684569,3.01127358511089,32.8017718474213));
#29748=CARTESIAN_POINT('Ctrl Pts',(-3.77654000587387,3.15617610581573,32.7911169611383));
#29749=CARTESIAN_POINT('Ctrl Pts',(-3.63442343299359,3.31373594136351,32.7790205807154));
#29750=CARTESIAN_POINT('Ctrl Pts',(-3.61658937575484,3.33319079522321,32.7775176231088));
#29751=CARTESIAN_POINT('Ctrl Pts',(-3.57633705161436,3.37639793655675,32.7741592419134));
#29752=CARTESIAN_POINT('Ctrl Pts',(-3.55383695770197,3.40007244587523,32.7723049630081));
#29753=CARTESIAN_POINT('Ctrl Pts',(-3.50208408780507,3.45345160756979,32.7680929386374));
#29754=CARTESIAN_POINT('Ctrl Pts',(-3.47268599138694,3.48301206161135,32.7657378992747));
#29755=CARTESIAN_POINT('Ctrl Pts',(-3.36516536396561,3.58841178598861,32.7572493145126));
#29756=CARTESIAN_POINT('Ctrl Pts',(-3.28490511314195,3.66202620814661,32.7511449553386));
#29757=CARTESIAN_POINT('Ctrl Pts',(-3.09565416227081,3.82437435529634,32.7371728841549));
#29758=CARTESIAN_POINT('Ctrl Pts',(-2.98517245241386,3.91122219310184,32.7293129700433));
#29759=CARTESIAN_POINT('Ctrl Pts',(-2.81526543242159,4.03338531598615,32.7175533308351));
#29760=CARTESIAN_POINT('Ctrl Pts',(-2.7585688035132,4.07237210951318,32.7136807670107));
#29761=CARTESIAN_POINT('Ctrl Pts',(-2.6468363617085,4.14579936914446,32.7061370505693));
#29762=CARTESIAN_POINT('Ctrl Pts',(-2.59189956983937,4.18036501229515,32.7024676775597));
#29763=CARTESIAN_POINT('Ctrl Pts',(-2.493951415639,4.23931975303067,32.6959886889768));
#29764=CARTESIAN_POINT('Ctrl Pts',(-2.45122605717117,4.26416655353984,32.6931831198771));
#29765=CARTESIAN_POINT('Ctrl Pts',(-2.28216540303006,4.35910265538149,32.6821579417854));
#29766=CARTESIAN_POINT('Ctrl Pts',(-2.15314288106775,4.42425470442737,32.6739061271532));
#29767=CARTESIAN_POINT('Ctrl Pts',(-1.92078185345519,4.52901447172894,32.6593188151783));
#29768=CARTESIAN_POINT('Ctrl Pts',(-1.81862210390815,4.57099428774983,32.6529947957574));
#29769=CARTESIAN_POINT('Ctrl Pts',(-1.68382211936691,4.62115163674049,32.6447788025502));
#29770=CARTESIAN_POINT('Ctrl Pts',(-1.65239019751979,4.63248378638489,32.6428720335531));
#29771=CARTESIAN_POINT('Ctrl Pts',(-1.60873744627857,4.64772109200645,32.6402369563724));
#29772=CARTESIAN_POINT('Ctrl Pts',(-1.59661324796914,4.65190000513202,32.6395064701106));
#29773=CARTESIAN_POINT('Ctrl Pts',(-1.57646755726513,4.65875569322073,32.6382950315472));
#29774=CARTESIAN_POINT('Ctrl Pts',(-1.56845526880095,4.66145928206874,32.6378138351496));
#29775=CARTESIAN_POINT('Ctrl Pts',(-1.52924068565654,4.67457891824853,32.6354617549767));
#29776=CARTESIAN_POINT('Ctrl Pts',(-1.49794121652518,4.68470247466156,32.6335938203768));
#29777=CARTESIAN_POINT('Ctrl Pts',(-1.42749105346604,4.7067107607663,32.6294116986244));
#29778=CARTESIAN_POINT('Ctrl Pts',(-1.38828878761749,4.71842253080182,32.6270999992584));
#29779=CARTESIAN_POINT('Ctrl Pts',(-1.26988528690195,4.75219246801465,32.6201569861744));
#29780=CARTESIAN_POINT('Ctrl Pts',(-1.19027218020022,4.77275541734493,32.6155406316724));
#29781=CARTESIAN_POINT('Ctrl Pts',(-0.967442638585062,4.82438656597629,
32.6027136715575));
#29782=CARTESIAN_POINT('Ctrl Pts',(-0.823298387203489,4.85106490491087,
32.5945208375277));
#29783=CARTESIAN_POINT('Ctrl Pts',(-0.604038665995732,4.88159027870891,
32.5820938449706));
#29784=CARTESIAN_POINT('Ctrl Pts',(-0.529673063597622,4.89021805896607,
32.5778855295306));
#29785=CARTESIAN_POINT('Ctrl Pts',(-0.392486488953327,4.90296816158783,
32.5701200485514));
#29786=CARTESIAN_POINT('Ctrl Pts',(-0.329727398983781,4.90758822378181,
32.5665667637238));
#29787=CARTESIAN_POINT('Ctrl Pts',(-0.203981771667592,4.91442209888197,
32.5594390330053));
#29788=CARTESIAN_POINT('Ctrl Pts',(-0.141006709061911,4.91663199026831,
32.5558652248059));
#29789=CARTESIAN_POINT('Ctrl Pts',(0.142638215829047,4.92113137197392,32.5397397685698));
#29790=CARTESIAN_POINT('Ctrl Pts',(0.363266470963693,4.9097774368799,32.5271056694717));
#29791=CARTESIAN_POINT('Ctrl Pts',(0.649454668650239,4.87564914118715,32.5106155754782));
#29792=CARTESIAN_POINT('Ctrl Pts',(0.716356795105859,4.8662695113464,32.5067545327153));
#29793=CARTESIAN_POINT('Ctrl Pts',(0.793427863182637,4.85384032499064,32.5023034779221));
#29794=CARTESIAN_POINT('Ctrl Pts',(0.803805554382793,4.85213255238824,32.5017040757773));
#29795=CARTESIAN_POINT('Ctrl Pts',(0.820567929498528,4.84931885125798,32.5007358256911));
#29796=CARTESIAN_POINT('Ctrl Pts',(0.826956036905678,4.84823357123718,32.500366809505));
#29797=CARTESIAN_POINT('Ctrl Pts',(0.837254210250674,4.84646306163683,32.4997719011601));
#29798=CARTESIAN_POINT('Ctrl Pts',(0.841165620263379,4.84578571747843,32.4995459401999));
#29799=CARTESIAN_POINT('Ctrl Pts',(0.847477672439167,4.84468477815542,32.4991812877789));
#29800=CARTESIAN_POINT('Ctrl Pts',(0.849878825761404,4.8442641326114,32.4990425695278));
#29801=CARTESIAN_POINT('Ctrl Pts',(0.853760958144185,4.84358106683526,32.4988182905467));
#29802=CARTESIAN_POINT('Ctrl Pts',(0.855242130736293,4.8433197522435,32.4987327195303));
#29803=CARTESIAN_POINT('Ctrl Pts',(0.860443616203352,4.84239962421464,32.4984322150544));
#29804=CARTESIAN_POINT('Ctrl Pts',(0.864163291764906,4.84173720295352,32.498217315764));
#29805=CARTESIAN_POINT('Ctrl Pts',(0.900114224704042,4.83529210472728,32.4961402760202));
#29806=CARTESIAN_POINT('Ctrl Pts',(0.932287951571422,4.82919191577159,32.4942812808667));
#29807=CARTESIAN_POINT('Ctrl Pts',(1.0057818365604,4.8144955100474,32.490035696042));
#29808=CARTESIAN_POINT('Ctrl Pts',(1.04705721484502,4.80568781375992,32.4876518998469));
#29809=CARTESIAN_POINT('Ctrl Pts',(1.237784048469,4.76241497201226,32.4766271864561));
#29810=CARTESIAN_POINT('Ctrl Pts',(1.38568612253881,4.72150195589864,32.4680480810393));
#29811=CARTESIAN_POINT('Ctrl Pts',(1.62996084104978,4.64146099469856,32.4536462924904));
#29812=CARTESIAN_POINT('Ctrl Pts',(1.72744002102068,4.60607026231088,32.4478354389095));
#29813=CARTESIAN_POINT('Ctrl Pts',(1.86049615142849,4.55294460933225,32.4397806885209));
#29814=CARTESIAN_POINT('Ctrl Pts',(1.89708635675511,4.53782038841545,32.4375525732523));
#29815=CARTESIAN_POINT('Ctrl Pts',(1.99914616857937,4.49418473312649,32.4312979293522));
#29816=CARTESIAN_POINT('Ctrl Pts',(2.06418286655256,4.46468708399541,32.4272656470407));
#29817=CARTESIAN_POINT('Ctrl Pts',(2.18583592533629,4.40628435941377,32.4196250876773));
#29818=CARTESIAN_POINT('Ctrl Pts',(2.24257937561657,4.37767725864049,32.4160197626599));
#29819=CARTESIAN_POINT('Ctrl Pts',(2.39664270532158,4.29622483668842,32.4061101028396));
#29820=CARTESIAN_POINT('Ctrl Pts',(2.49275652416012,4.24118008997661,32.3997920427883));
#29821=CARTESIAN_POINT('Ctrl Pts',(2.70086432245889,4.11247627398828,32.3857994867055));
#29822=CARTESIAN_POINT('Ctrl Pts',(2.81187257550138,4.03738799354103,32.3781237791633));
#29823=CARTESIAN_POINT('Ctrl Pts',(2.96262852986172,3.92617677435083,32.3674170679473));
#29824=CARTESIAN_POINT('Ctrl Pts',(3.00506197851664,3.89379435023872,32.3643706497929));
#29825=CARTESIAN_POINT('Ctrl Pts',(3.08100310135131,3.83386016017592,32.3588619565415));
#29826=CARTESIAN_POINT('Ctrl Pts',(3.11468945864057,3.80654350727084,32.3563974897815));
#29827=CARTESIAN_POINT('Ctrl Pts',(3.17501683146691,3.75628629235269,32.3519480826966));
#29828=CARTESIAN_POINT('Ctrl Pts',(3.20178139767933,3.73349896181448,32.3499610428675));
#29829=CARTESIAN_POINT('Ctrl Pts',(3.2866283975543,3.65967684559354,32.3436149107833));
#29830=CARTESIAN_POINT('Ctrl Pts',(3.34375294630614,3.6075583560906,32.3392704268443));
#29831=CARTESIAN_POINT('Ctrl Pts',(3.53372647687359,3.4258425243478,32.3245213267037));
#29832=CARTESIAN_POINT('Ctrl Pts',(3.6604598571039,3.29008408981024,32.3141552575836));
#29833=CARTESIAN_POINT('Ctrl Pts',(3.80506657998011,3.11645355866329,32.3014541254059));
#29834=CARTESIAN_POINT('Ctrl Pts',(3.83053158783609,3.08510002955052,32.2991815122524));
#29835=CARTESIAN_POINT('Ctrl Pts',(3.90038456975401,2.99689591143864,32.2928426034525));
#29836=CARTESIAN_POINT('Ctrl Pts',(3.94391223809736,2.9393776545411,32.2887705624053));
#29837=CARTESIAN_POINT('Ctrl Pts',(4.02308190031293,2.82983539840941,32.281119339032));
#29838=CARTESIAN_POINT('Ctrl Pts',(4.05901904386205,2.77804259343399,32.2775434505342));
#29839=CARTESIAN_POINT('Ctrl Pts',(4.16562944127532,2.61790834981748,32.266606251059));
#29840=CARTESIAN_POINT('Ctrl Pts',(4.23303249981231,2.50745845763278,32.2592230363756));
#29841=CARTESIAN_POINT('Ctrl Pts',(4.36330262097211,2.273737399233,32.2439150719001));
#29842=CARTESIAN_POINT('Ctrl Pts',(4.42548213529523,2.15020919278186,32.2359945087281));
#29843=CARTESIAN_POINT('Ctrl Pts',(4.50728083199563,1.96907700271781,32.22464834033));
#29844=CARTESIAN_POINT('Ctrl Pts',(4.53116625406901,1.91347256187222,32.2212006027623));
#29845=CARTESIAN_POINT('Ctrl Pts',(4.56789802601181,1.82341467905926,32.2156779749613));
#29846=CARTESIAN_POINT('Ctrl Pts',(4.58139456278496,1.78923373776153,32.2135962190511));
#29847=CARTESIAN_POINT('Ctrl Pts',(4.61597437639223,1.69870048477678,32.2081187551943));
#29848=CARTESIAN_POINT('Ctrl Pts',(4.63640890647218,1.64210698853568,32.2047305994798));
#29849=CARTESIAN_POINT('Ctrl Pts',(4.71263510317002,1.41822066592116,32.1914378081139));
#29850=CARTESIAN_POINT('Ctrl Pts',(4.76045126248027,1.24835244530733,32.1815886750155));
#29851=CARTESIAN_POINT('Ctrl Pts',(4.8224956688736,0.971702539606581,32.1656814287329));
#29852=CARTESIAN_POINT('Ctrl Pts',(4.8425250117809,0.866384096647093,32.1596569747165));
#29853=CARTESIAN_POINT('Ctrl Pts',(4.86959068225973,0.693451372460276,32.1497793112096));
#29854=CARTESIAN_POINT('Ctrl Pts',(4.87869507938473,0.626196778192807,32.145941542014));
#29855=CARTESIAN_POINT('Ctrl Pts',(4.89563000022488,0.478103625737029,32.1374908114927));
#29856=CARTESIAN_POINT('Ctrl Pts',(4.90285583936344,0.397216025658544,32.1328749618724));
#29857=CARTESIAN_POINT('Ctrl Pts',(4.92041646629665,0.124628013814521,32.1173075435281));
#29858=CARTESIAN_POINT('Ctrl Pts',(4.92153172102713,-0.0674884544777613,
32.1063090537897));
#29859=CARTESIAN_POINT('Ctrl Pts',(4.90918679588407,-0.301427036670187,
32.0929113966732));
#29860=CARTESIAN_POINT('Ctrl Pts',(4.90641202517168,-0.343648541149271,
32.0904935439874));
#29861=CARTESIAN_POINT('Ctrl Pts',(4.89863565198554,-0.442470216021985,
32.084836833841));
#29862=CARTESIAN_POINT('Ctrl Pts',(4.8931973174559,-0.499030324074055,32.081601070888));
#29863=CARTESIAN_POINT('Ctrl Pts',(4.88262133299154,-0.592070839501786,
32.0762856762812));
#29864=CARTESIAN_POINT('Ctrl Pts',(4.87805172631186,-0.628609855692929,
32.07420047991));
#29865=CARTESIAN_POINT('Ctrl Pts',(4.86435175545564,-0.728987976991618,
32.0684763348319));
#29866=CARTESIAN_POINT('Ctrl Pts',(4.85437550692771,-0.792704271327938,
32.0648466293617));
#29867=CARTESIAN_POINT('Ctrl Pts',(4.81332895339126,-1.02488492589481,32.05160072899));
#29868=CARTESIAN_POINT('Ctrl Pts',(4.7747169036367,-1.19189078407979,32.0420317813659));
#29869=CARTESIAN_POINT('Ctrl Pts',(4.71358837224592,-1.40492025934216,32.0295963251768));
#29870=CARTESIAN_POINT('Ctrl Pts',(4.69896440756757,-1.45308283903252,32.0267696845918));
#29871=CARTESIAN_POINT('Ctrl Pts',(4.67194198512438,-1.53740081787702,32.0217898143954));
#29872=CARTESIAN_POINT('Ctrl Pts',(4.65985647048045,-1.57365207107422,32.0196385019994));
#29873=CARTESIAN_POINT('Ctrl Pts',(4.62437344509401,-1.67609104737681,32.0135273384163));
#29874=CARTESIAN_POINT('Ctrl Pts',(4.59997975761903,-1.74192337387047,32.0095617136981));
#29875=CARTESIAN_POINT('Ctrl Pts',(4.54694043371693,-1.87616988835343,32.0013863474544));
#29876=CARTESIAN_POINT('Ctrl Pts',(4.51813961937075,-1.94450378304214,31.9971764500812));
#29877=CARTESIAN_POINT('Ctrl Pts',(4.42285734052015,-2.15701587907758,31.9839203144985));
#29878=CARTESIAN_POINT('Ctrl Pts',(4.35093476627361,-2.29864094116732,31.9748416627817));
#29879=CARTESIAN_POINT('Ctrl Pts',(4.20813272919024,-2.54903385339887,31.9583406935008));
#29880=CARTESIAN_POINT('Ctrl Pts',(4.13955608773341,-2.65895291696665,31.9509285618532));
#29881=CARTESIAN_POINT('Ctrl Pts',(4.04354906234367,-2.80010563883098,31.9412131265006));
#29882=CARTESIAN_POINT('Ctrl Pts',(4.01994996802421,-2.83388124665608,31.9388729832889));
#29883=CARTESIAN_POINT('Ctrl Pts',(3.9710925466402,-2.90196862377059,31.9341262255734));
#29884=CARTESIAN_POINT('Ctrl Pts',(3.94580716555951,-2.93625676265668,31.9317201548369));
#29885=CARTESIAN_POINT('Ctrl Pts',(3.84557476440126,-3.06854325311272,31.9223651272712));
#29886=CARTESIAN_POINT('Ctrl Pts',(3.76739601596059,-3.16403711250589,31.9154540826268));
#29887=CARTESIAN_POINT('Ctrl Pts',(3.57432088167013,-3.38256027600637,31.8991175607479));
#29888=CARTESIAN_POINT('Ctrl Pts',(3.45653911578827,-3.50283032408301,31.8897001418591));
#29889=CARTESIAN_POINT('Ctrl Pts',(3.27962601469965,-3.66585188926085,31.8761474393099));
#29890=CARTESIAN_POINT('Ctrl Pts',(3.22534946573542,-3.71369594000595,31.8720631359297));
#29891=CARTESIAN_POINT('Ctrl Pts',(3.11534787214414,-3.80642973586241,31.8639187889937));
#29892=CARTESIAN_POINT('Ctrl Pts',(3.05965912469724,-3.85133555797317,31.8598599640447));
#29893=CARTESIAN_POINT('Ctrl Pts',(2.86341742712058,-4.00263580087408,31.8457649633492));
#29894=CARTESIAN_POINT('Ctrl Pts',(2.71814028785715,-4.1026777396443,31.8356839266383));
#29895=CARTESIAN_POINT('Ctrl Pts',(2.46771310301434,-4.25597801744582,31.8188757304435));
#29896=CARTESIAN_POINT('Ctrl Pts',(2.36545500087633,-4.31365041671854,31.812160277848));
#29897=CARTESIAN_POINT('Ctrl Pts',(2.22286554409817,-4.38747288319392,31.8030177059554));
#29898=CARTESIAN_POINT('Ctrl Pts',(2.18423947857324,-4.4068296411166,31.8005627224517));
#29899=CARTESIAN_POINT('Ctrl Pts',(2.10873297993352,-4.44343170822524,31.7958079337076));
#29900=CARTESIAN_POINT('Ctrl Pts',(2.0718835719005,-4.46073297032506,31.7935077063911));
#29901=CARTESIAN_POINT('Ctrl Pts',(1.89035643111482,-4.54322755398639,31.7822633208131));
#29902=CARTESIAN_POINT('Ctrl Pts',(1.74279501859907,-4.60185079598211,31.7733882080577));
#29903=CARTESIAN_POINT('Ctrl Pts',(1.49518597957512,-4.68659956494461,31.7587253056825));
#29904=CARTESIAN_POINT('Ctrl Pts',(1.39669155875464,-4.7168897660678,31.7529510233837));
#29905=CARTESIAN_POINT('Ctrl Pts',(1.21651225788719,-4.76616187936163,31.7424488838611));
#29906=CARTESIAN_POINT('Ctrl Pts',(1.13515459040011,-4.78619107022724,31.7377289381991));
#29907=CARTESIAN_POINT('Ctrl Pts',(0.987357167351199,-4.81859626347323,
31.7291775912551));
#29908=CARTESIAN_POINT('Ctrl Pts',(0.921098137390741,-4.83169972288105,
31.7253522608998));
#29909=CARTESIAN_POINT('Ctrl Pts',(0.755088710929473,-4.86099094832161,
31.7157807794224));
#29910=CARTESIAN_POINT('Ctrl Pts',(0.65507024041673,-4.87547685333203,31.7100251178952));
#29911=CARTESIAN_POINT('Ctrl Pts',(0.397283520256164,-4.90473658301958,
31.6952074155762));
#29912=CARTESIAN_POINT('Ctrl Pts',(0.239118382497657,-4.91498700220826,
31.6861299678684));
#29913=CARTESIAN_POINT('Ctrl Pts',(0.00162993316986859,-4.91888603726153,
31.6725504439781));
#29914=CARTESIAN_POINT('Ctrl Pts',(-0.0774966152352732,-4.91827581665873,
31.668035089894));
#29915=CARTESIAN_POINT('Ctrl Pts',(-0.194215459421216,-4.91455813778132,
31.6613974300692));
#29916=CARTESIAN_POINT('Ctrl Pts',(-0.23184160426101,-4.91292691408511,
31.6592613797802));
#29917=CARTESIAN_POINT('Ctrl Pts',(-0.319382480133557,-4.90812378369549,
31.6543011786491));
#29918=CARTESIAN_POINT('Ctrl Pts',(-0.369274920689384,-4.90462234638863,
31.6514806837639));
#29919=CARTESIAN_POINT('Ctrl Pts',(-0.579434353461689,-4.88664836133908,
31.6396091066608));
#29920=CARTESIAN_POINT('Ctrl Pts',(-0.738994742042416,-4.86507594824511,
31.6306150444924));
#29921=CARTESIAN_POINT('Ctrl Pts',(-1.02549528895035,-4.81191914111337,
31.6142829566083));
#29922=CARTESIAN_POINT('Ctrl Pts',(-1.1527801836611,-4.78302243700408,31.6069607211795));
#29923=CARTESIAN_POINT('Ctrl Pts',(-1.34553160870584,-4.73112131137844,
31.5957037557488));
#29924=CARTESIAN_POINT('Ctrl Pts',(-1.41191201724013,-4.71173731081854,
31.5917960856352));
#29925=CARTESIAN_POINT('Ctrl Pts',(-1.55062423205501,-4.66803679412807,
31.5835561354923));
#29926=CARTESIAN_POINT('Ctrl Pts',(-1.62284347518102,-4.6434235092388,31.579222780513));
#29927=CARTESIAN_POINT('Ctrl Pts',(-1.79147463122629,-4.58153697966321,
31.5689939831573));
#29928=CARTESIAN_POINT('Ctrl Pts',(-1.88734188464374,-4.54288484641345,
31.5630917669334));
#29929=CARTESIAN_POINT('Ctrl Pts',(-2.09449406887103,-4.45167469675351,
31.5501427815741));
#29930=CARTESIAN_POINT('Ctrl Pts',(-2.20516966381219,-4.3979017539788,31.5430960680165));
#29931=CARTESIAN_POINT('Ctrl Pts',(-2.35920951919484,-4.31578170723857,
31.5331215532521));
#29932=CARTESIAN_POINT('Ctrl Pts',(-2.40432226589841,-4.29081295383114,
31.5301795111084));
#29933=CARTESIAN_POINT('Ctrl Pts',(-2.4857973875931,-4.24403010529337,31.5248309590377));
#29934=CARTESIAN_POINT('Ctrl Pts',(-2.52228627875029,-4.22244623056907,
31.5224224535096));
#29935=CARTESIAN_POINT('Ctrl Pts',(-2.58895037522541,-4.18184061595814,
31.5180000327539));
#29936=CARTESIAN_POINT('Ctrl Pts',(-2.61920642241261,-4.16295720984173,
31.515984355191));
#29937=CARTESIAN_POINT('Ctrl Pts',(-2.72761138505175,-4.09364979464148,
31.508725560008));
#29938=CARTESIAN_POINT('Ctrl Pts',(-2.8045322821114,-4.04134031442693,31.5035048204836));
#29939=CARTESIAN_POINT('Ctrl Pts',(-2.98211058633536,-3.91306658362485,
31.4912228687434));
#29940=CARTESIAN_POINT('Ctrl Pts',(-3.08142110118553,-3.83535104102186,
31.4841709378827));
#29941=CARTESIAN_POINT('Ctrl Pts',(-3.23825104032613,-3.7025964070266,31.472643003271));
#29942=CARTESIAN_POINT('Ctrl Pts',(-3.29761403155249,-3.64982622821028,
31.4681813515752));
#29943=CARTESIAN_POINT('Ctrl Pts',(-3.40890906717953,-3.54595890547476,
31.4596061964944));
#29944=CARTESIAN_POINT('Ctrl Pts',(-3.46103489451756,-3.49509983900012,
31.4554956530768));
#29945=CARTESIAN_POINT('Ctrl Pts',(-3.55585517044263,-3.39838185768247,
31.4478292706966));
#29946=CARTESIAN_POINT('Ctrl Pts',(-3.59883996381569,-3.35282806764481,
31.4442770372839));
#29947=CARTESIAN_POINT('Ctrl Pts',(-3.78848543252156,-3.14399837843591,
31.4282419773723));
#29948=CARTESIAN_POINT('Ctrl Pts',(-3.92498640670963,-2.97183895602579,
31.4156776589896));
#29949=CARTESIAN_POINT('Ctrl Pts',(-4.07718537579441,-2.75102109919743,
31.4003329315466));
#29950=CARTESIAN_POINT('Ctrl Pts',(-4.10424228942476,-2.71048942786026,
31.3975466365238));
#29951=CARTESIAN_POINT('Ctrl Pts',(-4.16419258859877,-2.61772656015373,
31.3912404470853));
#29952=CARTESIAN_POINT('Ctrl Pts',(-4.19671429913832,-2.56526440778693,
31.3877234786657));
#29953=CARTESIAN_POINT('Ctrl Pts',(-4.24701543741232,-2.48060355787563,
31.3821312994515));
#29954=CARTESIAN_POINT('Ctrl Pts',(-4.26543580505892,-2.44879390149749,
31.3800487968995));
#29955=CARTESIAN_POINT('Ctrl Pts',(-4.31250644559897,-2.36536596286729,
31.3746342415875));
#29956=CARTESIAN_POINT('Ctrl Pts',(-4.3405870209525,-2.31343303744498,31.3713093051831));
#29957=CARTESIAN_POINT('Ctrl Pts',(-4.4494291926429,-2.10317590795498,31.3580006141759));
#29958=CARTESIAN_POINT('Ctrl Pts',(-4.52251756330337,-1.94103182669218,
31.3480747426424));
#29959=CARTESIAN_POINT('Ctrl Pts',(-4.61529951089046,-1.70131848953204,
31.3336534107982));
#29960=CARTESIAN_POINT('Ctrl Pts',(-4.64213582261033,-1.62666807509976,
31.3291972816092));
#29961=CARTESIAN_POINT('Ctrl Pts',(-4.69010956012718,-1.48234643152991,
31.3206303173598));
#29962=CARTESIAN_POINT('Ctrl Pts',(-4.71152853707399,-1.41279061141428,
31.3165224240597));
#29963=CARTESIAN_POINT('Ctrl Pts',(-4.74850175640768,-1.2825129780289,31.3088572140402));
#29964=CARTESIAN_POINT('Ctrl Pts',(-4.76445396557959,-1.22191929837059,
31.3053034819171));
#29965=CARTESIAN_POINT('Ctrl Pts',(-4.81185372010229,-1.02680507536187,
31.2938897757146));
#29966=CARTESIAN_POINT('Ctrl Pts',(-4.83879327110196,-0.891259620807821,
31.2860034399518));
#29967=CARTESIAN_POINT('Ctrl Pts',(-4.8781202976721,-0.638028776126936,
31.2713401896921));
#29968=CARTESIAN_POINT('Ctrl Pts',(-4.8920374740413,-0.520680138724421,
31.2645731393547));
#29969=CARTESIAN_POINT('Ctrl Pts',(-4.90586920547575,-0.352420624249749,
31.2549273557728));
#29970=CARTESIAN_POINT('Ctrl Pts',(-4.90924112300201,-0.301835410350173,
31.2520349682412));
#29971=CARTESIAN_POINT('Ctrl Pts',(-4.9139717327666,-0.209338117679563,
31.2467628927219));
#29972=CARTESIAN_POINT('Ctrl Pts',(-4.91557762641747,-0.167443394703228,
31.2443813010125));
#29973=CARTESIAN_POINT('Ctrl Pts',(-4.91771536839545,-0.0837161899047983,
31.2396365451753));
#29974=CARTESIAN_POINT('Ctrl Pts',(-4.91824952237092,-0.0418871676881771,
31.2372735538595));
#29975=CARTESIAN_POINT('Ctrl Pts',(-4.91825149861551,0.131305456968749,
31.2275096094303));
#29976=CARTESIAN_POINT('Ctrl Pts',(-4.9129901901366,0.262615805166311,31.2201531886595));
#29977=CARTESIAN_POINT('Ctrl Pts',(-4.88944461670753,0.555917895767881,
31.2036689342295));
#29978=CARTESIAN_POINT('Ctrl Pts',(-4.86835359385957,0.717527581964215,
31.1945482689874));
#29979=CARTESIAN_POINT('Ctrl Pts',(-4.82640190675748,0.948808230003812,
31.1813057443297));
#29980=CARTESIAN_POINT('Ctrl Pts',(-4.81195860808438,1.01953254902896,31.1772308136538));
#29981=CARTESIAN_POINT('Ctrl Pts',(-4.78592903657929,1.13407097096521,31.170581542657));
#29982=CARTESIAN_POINT('Ctrl Pts',(-4.77528476076275,1.1780869639915,31.1680142019493));
#29983=CARTESIAN_POINT('Ctrl Pts',(-4.76403458668766,1.2219482474081,31.1654428831549));
#29984=CARTESIAN_POINT('',(-4.91824999844923,0.000123507507276638,30.8898594359908));
#29985=CARTESIAN_POINT('Ctrl Pts',(-4.76403458704967,1.22194824599672,30.8199238152312));
#29986=CARTESIAN_POINT('Ctrl Pts',(-4.79982283587317,1.08241986927238,30.8280803104528));
#29987=CARTESIAN_POINT('Ctrl Pts',(-4.82947448833597,0.94132853557534,30.8362368056745));
#29988=CARTESIAN_POINT('Ctrl Pts',(-4.85287721761797,0.799228236002976,
30.8443933008961));
#29989=CARTESIAN_POINT('Ctrl Pts',(-4.87013621133165,0.694432417212852,
30.8504085351904));
#29990=CARTESIAN_POINT('Ctrl Pts',(-4.88399762918098,0.589088131054119,
30.8564237694847));
#29991=CARTESIAN_POINT('Ctrl Pts',(-4.89443437256851,0.483420350336929,
30.8624390037789));
#29992=CARTESIAN_POINT('Ctrl Pts',(-4.90948242451799,0.331064946493519,
30.8711119733813));
#29993=CARTESIAN_POINT('Ctrl Pts',(-4.91741278380546,0.178001677768284,
30.8797849429838));
#29994=CARTESIAN_POINT('Ctrl Pts',(-4.91818712165292,0.0248696382643597,
30.8884579125863));
#29995=CARTESIAN_POINT('Ctrl Pts',(-4.91822883180395,0.0166210933719668,
30.8889250870544));
#29996=CARTESIAN_POINT('Ctrl Pts',(-4.91824979130361,0.00837234974432156,
30.8893922615226));
#29997=CARTESIAN_POINT('Ctrl Pts',(-4.91824999844923,0.000123507507276638,
30.8898594359908));
#29998=CARTESIAN_POINT('Ctrl Pts',(-4.91833690826082,0.000123432691201461,
30.8898594403516));
#29999=CARTESIAN_POINT('Ctrl Pts',(-4.91765989171386,-0.656721429210889,
30.9270592933315));
#30000=CARTESIAN_POINT('Ctrl Pts',(-4.62027241517956,-2.13239495771996,
31.0105991448156));
#30001=CARTESIAN_POINT('Ctrl Pts',(-3.18782294371806,-4.0156960603218,31.1404789948039));
#30002=CARTESIAN_POINT('Ctrl Pts',(-0.876714416284051,-5.05167316853129,
31.2794989903164));
#30003=CARTESIAN_POINT('Ctrl Pts',(1.64831882804362,-4.85500515040882,31.4185189858289));
#30004=CARTESIAN_POINT('Ctrl Pts',(3.77115024690762,-3.47368043789694,31.5575389813414));
#30005=CARTESIAN_POINT('Ctrl Pts',(4.97379347911828,-1.24475234342413,31.696558976854));
#30006=CARTESIAN_POINT('Ctrl Pts',(4.96279479767373,1.28790440854975,31.8355789723664));
#30007=CARTESIAN_POINT('Ctrl Pts',(3.7408379611281,3.50630308415606,31.974598967879));
#30008=CARTESIAN_POINT('Ctrl Pts',(1.60608935691497,4.86913821399472,32.1136189633915));
#30009=CARTESIAN_POINT('Ctrl Pts',(-0.920556773564781,5.04386807876885,
32.2526389589041));
#30010=CARTESIAN_POINT('Ctrl Pts',(-3.22258033195988,3.98785731608399,32.3916589544165));
#30011=CARTESIAN_POINT('Ctrl Pts',(-4.37570558480373,2.44415159686769,32.4974242635864));
#30012=CARTESIAN_POINT('Ctrl Pts',(-4.70671521754109,1.44580583700442,32.5568495742522));
#30013=CARTESIAN_POINT('Ctrl Pts',(-4.7639087307945,1.22191632179108,32.5699348864137));
#30014=CARTESIAN_POINT('Origin',(0.,0.,-3.23514056400928));
#30015=CARTESIAN_POINT('',(-4.76374291154778,1.22187309174177,34.6652037882801));
#30016=CARTESIAN_POINT('',(-4.76403458704967,1.22194824599671,34.3199237602016));
#30017=CARTESIAN_POINT('',(-4.76403458704967,1.22194824599672,-3.23514056400928));
#30018=CARTESIAN_POINT('',(-4.91786285480381,-3.23909219955966E-5,32.9851526239175));
#30019=CARTESIAN_POINT('Ctrl Pts',(-4.91784190852614,-3.30751234541968E-5,
32.9851405682246));
#30020=CARTESIAN_POINT('Ctrl Pts',(-4.91792932869888,-0.373298708305577,
33.006274043888));
#30021=CARTESIAN_POINT('Ctrl Pts',(-4.78405248732222,-1.56453986243927,
33.073722981313));
#30022=CARTESIAN_POINT('Ctrl Pts',(-3.83240713769111,-3.40563728872529,
33.1874873804997));
#30023=CARTESIAN_POINT('Ctrl Pts',(-1.73594721364791,-4.82412656164927,
33.3264337657849));
#30024=CARTESIAN_POINT('Ctrl Pts',(0.783657389885535,-5.06671401469037,
33.46538015107));
#30025=CARTESIAN_POINT('Ctrl Pts',(3.11224209807527,-4.07426790164198,33.6043265363551));
#30026=CARTESIAN_POINT('Ctrl Pts',(4.68220426594096,-2.08870127672345,33.7432729216403));
#30027=CARTESIAN_POINT('Ctrl Pts',(5.11085879043896,0.405995363982041,33.8822193069254));
#30028=CARTESIAN_POINT('Ctrl Pts',(4.29371926786136,2.80172886985484,34.0211656922105));
#30029=CARTESIAN_POINT('Ctrl Pts',(2.42996700894246,4.51452878458352,34.1601120774956));
#30030=CARTESIAN_POINT('Ctrl Pts',(-0.0261002714740853,5.12689268341077,
34.2990584627807));
#30031=CARTESIAN_POINT('Ctrl Pts',(-2.47580549726093,4.48955420405128,34.4380048480659));
#30032=CARTESIAN_POINT('Ctrl Pts',(-4.09749498730757,2.96846620137155,34.560053289899));
#30033=CARTESIAN_POINT('Ctrl Pts',(-4.6343106032874,1.72504109344374,34.6357862699704));
#30034=CARTESIAN_POINT('Ctrl Pts',(-4.76374291154778,1.22187309174177,34.6652037882801));
#30035=CARTESIAN_POINT('Ctrl Pts',(-4.91824999996037,-1.97449862875235E-5,
32.9853754464731));
#30036=CARTESIAN_POINT('Ctrl Pts',(-4.91825017361617,0.0432359271112932,
32.9829326257254));
#30037=CARTESIAN_POINT('Ctrl Pts',(-4.91767970138599,0.0864895187082102,
32.9804863497487));
#30038=CARTESIAN_POINT('Ctrl Pts',(-4.9153025743111,0.176578622886849,32.9753817507004));
#30039=CARTESIAN_POINT('Ctrl Pts',(-4.91339684882255,0.223407179894823,
32.972723027043));
#30040=CARTESIAN_POINT('Ctrl Pts',(-4.90485341734412,0.378681430613462,
32.9638865071782));
#30041=CARTESIAN_POINT('Ctrl Pts',(-4.89529185867349,0.486933085201178,
32.9576917406495));
#30042=CARTESIAN_POINT('Ctrl Pts',(-4.86028271416837,0.774300823744014,
32.9411447028977));
#30043=CARTESIAN_POINT('Ctrl Pts',(-4.82852675005391,0.952480656005482,
32.9307742699252));
#30044=CARTESIAN_POINT('Ctrl Pts',(-4.77966978282832,1.15972790237745,32.9186300745121));
#30045=CARTESIAN_POINT('Ctrl Pts',(-4.77200424158646,1.19087679106607,32.916802791448));
#30046=CARTESIAN_POINT('Ctrl Pts',(-4.76403458699526,1.22194824620887,32.9149784811847));
#30047=CARTESIAN_POINT('',(-4.91824999837229,-0.000126534489980439,32.6398594359908));
#30048=CARTESIAN_POINT('Ctrl Pts',(-4.7639087307945,1.22191632179108,32.5699348864137));
#30049=CARTESIAN_POINT('Ctrl Pts',(-4.86578454630458,0.823113631607463,
32.593243068965));
#30050=CARTESIAN_POINT('Ctrl Pts',(-4.91786568948866,0.411441406548216,
32.6165512515163));
#30051=CARTESIAN_POINT('Ctrl Pts',(-4.91829166267875,-0.000126501603607826,
32.6398594340676));
#30052=CARTESIAN_POINT('Ctrl Pts',(-4.91824999837229,-0.000126534489980439,
32.6398594359908));
#30053=CARTESIAN_POINT('Ctrl Pts',(-4.9182460739844,-0.152662975038819,
32.6484980527229));
#30054=CARTESIAN_POINT('Ctrl Pts',(-4.91114158002739,-0.305164623492694,
32.6571366694551));
#30055=CARTESIAN_POINT('Ctrl Pts',(-4.89697215839355,-0.456997529991619,
32.6657752861872));
#30056=CARTESIAN_POINT('Ctrl Pts',(-4.8948269082127,-0.479985029308245,
32.6670831726053));
#30057=CARTESIAN_POINT('Ctrl Pts',(-4.89251981310438,-0.502957206987885,
32.6683910590234));
#30058=CARTESIAN_POINT('Ctrl Pts',(-4.89005110050666,-0.525911871831763,
32.6696989454414));
#30059=CARTESIAN_POINT('Ctrl Pts',(-4.87465561600517,-0.669062673252445,
32.6778552391703));
#30060=CARTESIAN_POINT('Ctrl Pts',(-4.85296706059036,-0.811563777669985,
32.6860115328992));
#30061=CARTESIAN_POINT('Ctrl Pts',(-4.82506464173119,-0.952855847237913,
32.6941678266281));
#30062=CARTESIAN_POINT('Ctrl Pts',(-4.79716790981858,-1.09411911928639,
32.7023224579775));
#30063=CARTESIAN_POINT('Ctrl Pts',(-4.76305990581221,-1.23417351996479,
32.710477089327));
#30064=CARTESIAN_POINT('Ctrl Pts',(-4.72287104862409,-1.37246935141314,
32.7186317206764));
#30065=CARTESIAN_POINT('Ctrl Pts',(-4.68268076567248,-1.51077008912558,
32.7267866413244));
#30066=CARTESIAN_POINT('Ctrl Pts',(-4.63640928763732,-1.64731181037433,
32.7349415619723));
#30067=CARTESIAN_POINT('Ctrl Pts',(-4.58423720689594,-1.78155895030474,
32.7430964826203));
#30068=CARTESIAN_POINT('Ctrl Pts',(-4.53206819350884,-1.9157981974401,32.7512509238158));
#30069=CARTESIAN_POINT('Ctrl Pts',(-4.47399939357257,-2.04774282155977,
32.7594053650113));
#30070=CARTESIAN_POINT('Ctrl Pts',(-4.41025992885093,-2.17687629930407,
32.7675598062068));
#30071=CARTESIAN_POINT('Ctrl Pts',(-4.34650475302151,-2.30604160709268,
32.7757162573863));
#30072=CARTESIAN_POINT('Ctrl Pts',(-4.27707626735019,-2.43239408357324,
32.7838727085658));
#30073=CARTESIAN_POINT('Ctrl Pts',(-4.20225030301852,-2.55544036386701,
32.7920291597454));
#30074=CARTESIAN_POINT('Ctrl Pts',(-4.15121385158712,-2.63936638559112,
32.7975924201483));
#30075=CARTESIAN_POINT('Ctrl Pts',(-4.0976673651435,-2.72175479774588,32.8031556805512));
#30076=CARTESIAN_POINT('Ctrl Pts',(-4.04171019025238,-2.80245638690597,
32.8087189409541));
#30077=CARTESIAN_POINT('Ctrl Pts',(-3.95967139976016,-2.92077295271503,
32.8168752346829));
#30078=CARTESIAN_POINT('Ctrl Pts',(-3.8724183047003,-3.035506799502,32.8250315284118));
#30079=CARTESIAN_POINT('Ctrl Pts',(-3.78028818569261,-3.14620474470637,
32.8331878221406));
#30080=CARTESIAN_POINT('Ctrl Pts',(-3.6881768442351,-3.25688012794899,32.84134245349));
#30081=CARTESIAN_POINT('Ctrl Pts',(-3.59119067577382,-3.36352099353832,
32.8494970848394));
#30082=CARTESIAN_POINT('Ctrl Pts',(-3.48970731004212,-3.46570713603134,
32.8576517161888));
#30083=CARTESIAN_POINT('Ctrl Pts',(-3.38822034402671,-3.5678969037402,32.8658066368368));
#30084=CARTESIAN_POINT('Ctrl Pts',(-3.28223609462846,-3.66563139202599,
32.8739615574847));
#30085=CARTESIAN_POINT('Ctrl Pts',(-3.17216947869226,-3.75852682057123,
32.8821164781326));
#30086=CARTESIAN_POINT('Ctrl Pts',(-3.06210933390539,-3.8514167875132,32.8902709193281));
#30087=CARTESIAN_POINT('Ctrl Pts',(-2.94796755912266,-3.93946804877225,
32.8984253605235));
#30088=CARTESIAN_POINT('Ctrl Pts',(-2.83019256527175,-4.02233677182561,
32.906579801719));
#30089=CARTESIAN_POINT('Ctrl Pts',(-2.71238854112305,-4.10522592114799,
32.9147362528985));
#30090=CARTESIAN_POINT('Ctrl Pts',(-2.59094978207838,-4.18292978679778,
32.922892704078));
#30091=CARTESIAN_POINT('Ctrl Pts',(-2.46635462455556,-4.25514722758607,
32.9310491552575));
#30092=CARTESIAN_POINT('Ctrl Pts',(-2.38137216208393,-4.30440448664498,
32.9366124156605));
#30093=CARTESIAN_POINT('Ctrl Pts',(-2.29492190149264,-4.35111025836679,
32.9421756760636));
#30094=CARTESIAN_POINT('Ctrl Pts',(-2.2071624922942,-4.39518108786312,32.9477389364667));
#30095=CARTESIAN_POINT('Ctrl Pts',(-2.07849845950931,-4.45979331238655,
32.9558952301956));
#30096=CARTESIAN_POINT('Ctrl Pts',(-1.9469712168772,-4.5187640054613,32.9640515239244));
#30097=CARTESIAN_POINT('Ctrl Pts',(-1.81309381923539,-4.57185671966548,
32.9722078176532));
#30098=CARTESIAN_POINT('Ctrl Pts',(-1.67924370788772,-4.62493861274943,
32.9803624490027));
#30099=CARTESIAN_POINT('Ctrl Pts',(-1.54304470799748,-4.67214479365301,
32.9885170803521));
#30100=CARTESIAN_POINT('Ctrl Pts',(-1.40502951570803,-4.71328708254539,
32.9966717117016));
#30101=CARTESIAN_POINT('Ctrl Pts',(-1.2670094271106,-4.75443083102576,33.0048266323495));
#30102=CARTESIAN_POINT('Ctrl Pts',(-1.127173336803,-4.7895101578229,33.0129815529974));
#30103=CARTESIAN_POINT('Ctrl Pts',(-0.986069243359014,-4.81838671235522,
33.0211364736454));
#30104=CARTESIAN_POINT('Ctrl Pts',(-0.844973445851323,-4.8472615691476,
33.0292909148408));
#30105=CARTESIAN_POINT('Ctrl Pts',(-0.702610122412683,-4.86993431709509,
33.0374453560363));
#30106=CARTESIAN_POINT('Ctrl Pts',(-0.559537557595221,-4.88631771215712,
33.0455997972318));
#30107=CARTESIAN_POINT('Ctrl Pts',(-0.416429726894918,-4.90270514555376,
33.0537562484113));
#30108=CARTESIAN_POINT('Ctrl Pts',(-0.272612638089836,-4.9128000899778,
33.0619126995908));
#30109=CARTESIAN_POINT('Ctrl Pts',(-0.128650415256635,-4.91656710857833,
33.0700691507703));
#30110=CARTESIAN_POINT('Ctrl Pts',(-0.0304582828971516,-4.91913647421985,
33.0756324111732));
#30111=CARTESIAN_POINT('Ctrl Pts',(0.0678012572343151,-4.9187630562909,
33.0811956715761));
#30112=CARTESIAN_POINT('Ctrl Pts',(0.165948964316552,-4.91544952204193,
33.086758931979));
#30113=CARTESIAN_POINT('Ctrl Pts',(0.309843276247919,-4.91059155087796,
33.0949152257078));
#30114=CARTESIAN_POINT('Ctrl Pts',(0.453551059204196,-4.89940981069101,
33.1030715194366));
#30115=CARTESIAN_POINT('Ctrl Pts',(0.596508673255385,-4.88194228409463,
33.1112278131654));
#30116=CARTESIAN_POINT('Ctrl Pts',(0.739437150323049,-4.86447831765164,
33.1193824445148));
#30117=CARTESIAN_POINT('Ctrl Pts',(0.881615431522648,-4.84073116116138,
33.1275370758641));
#30118=CARTESIAN_POINT('Ctrl Pts',(1.02248573604808,-4.8107905776575,33.1356917072135));
#30119=CARTESIAN_POINT('Ctrl Pts',(1.16336103817132,-4.78084893196387,33.1438466278614));
#30120=CARTESIAN_POINT('Ctrl Pts',(1.30292794265939,-4.74471348548312,33.1520015485092));
#30121=CARTESIAN_POINT('Ctrl Pts',(1.44063908486165,-4.70252507592134,33.1601564691571));
#30122=CARTESIAN_POINT('Ctrl Pts',(1.57834213060943,-4.66033914674373,33.1683109103525));
#30123=CARTESIAN_POINT('Ctrl Pts',(1.71418931264419,-4.61210106538802,33.176465351548));
#30124=CARTESIAN_POINT('Ctrl Pts',(1.84764869829509,-4.55800146447853,33.1846197927434));
#30125=CARTESIAN_POINT('Ctrl Pts',(1.9811409802813,-4.50388852858625,33.1927762439228));
#30126=CARTESIAN_POINT('Ctrl Pts',(2.11224397942654,-4.44391131166096,33.2009326951023));
#30127=CARTESIAN_POINT('Ctrl Pts',(2.24044543438769,-4.37830872804001,33.2090891462817));
#30128=CARTESIAN_POINT('Ctrl Pts',(2.32788763962418,-4.33356325629193,33.214652406685));
#30129=CARTESIAN_POINT('Ctrl Pts',(2.41398041429648,-4.28620176541063,33.2202156670884));
#30130=CARTESIAN_POINT('Ctrl Pts',(2.49856766234332,-4.23631239395683,33.2257789274917));
#30131=CARTESIAN_POINT('Ctrl Pts',(2.62258099099763,-4.16316960752842,33.2339352212206));
#30132=CARTESIAN_POINT('Ctrl Pts',(2.74340356628593,-4.08456386030267,33.2420915149494));
#30133=CARTESIAN_POINT('Ctrl Pts',(2.86055869544279,-4.00079829689359,33.2502478086783));
#30134=CARTESIAN_POINT('Ctrl Pts',(2.97768994656362,-3.91704980620813,33.2584024400278));
#30135=CARTESIAN_POINT('Ctrl Pts',(3.09115497067334,-3.82814379184214,33.2665570713772));
#30136=CARTESIAN_POINT('Ctrl Pts',(3.20050700489114,-3.73442605685837,33.2747117027267));
#30137=CARTESIAN_POINT('Ctrl Pts',(3.309862918546,-3.64070499708913,33.2828666233746));
#30138=CARTESIAN_POINT('Ctrl Pts',(3.41510529379355,-3.54217209003059,33.2910215440226));
#30139=CARTESIAN_POINT('Ctrl Pts',(3.5158209608763,-3.43921299624824,33.2991764646705));
#30140=CARTESIAN_POINT('Ctrl Pts',(3.61653070658046,-3.33625995574233,33.3073309058661));
#30141=CARTESIAN_POINT('Ctrl Pts',(3.71271404321985,-3.2288814890323,33.3154853470616));
#30142=CARTESIAN_POINT('Ctrl Pts',(3.80399518545927,-3.11749958965558,33.3236397882571));
#30143=CARTESIAN_POINT('Ctrl Pts',(3.89529882754045,-3.00609023581182,33.3317962394366));
#30144=CARTESIAN_POINT('Ctrl Pts',(3.98169764828788,-2.89067573625114,33.3399526906161));
#30145=CARTESIAN_POINT('Ctrl Pts',(4.06285624459877,-2.77171105965698,33.3481091417956));
#30146=CARTESIAN_POINT('Ctrl Pts',(4.11821198636284,-2.69056897223881,33.3536724021985));
#30147=CARTESIAN_POINT('Ctrl Pts',(4.17113073013441,-2.6077759578888,33.3592356626013));
#30148=CARTESIAN_POINT('Ctrl Pts',(4.22151761319054,-2.52348412002573,33.3647989230041));
#30149=CARTESIAN_POINT('Ctrl Pts',(4.29538980117511,-2.39990389210712,33.3729552167329));
#30150=CARTESIAN_POINT('Ctrl Pts',(4.36384557851417,-2.27305451392679,33.3811115104617));
#30151=CARTESIAN_POINT('Ctrl Pts',(4.42661151612109,-2.1434303226007,33.3892678041905));
#30152=CARTESIAN_POINT('Ctrl Pts',(4.48936466105444,-2.01383255069937,33.3974224355399));
#30153=CARTESIAN_POINT('Ctrl Pts',(4.54643013398506,-1.8814613949083,33.4055770668892));
#30154=CARTESIAN_POINT('Ctrl Pts',(4.59758120336134,-1.7468343198479,33.4137316982386));
#30155=CARTESIAN_POINT('Ctrl Pts',(4.64873408740304,-1.61220246867823,33.4218866188865));
#30156=CARTESIAN_POINT('Ctrl Pts',(4.6939720256624,-1.47531484957851,33.4300415395344));
#30157=CARTESIAN_POINT('Ctrl Pts',(4.73311685971175,-1.33670784198058,33.4381964601822));
#30158=CARTESIAN_POINT('Ctrl Pts',(4.77225939231794,-1.19810898350777,33.4463509013777));
#30159=CARTESIAN_POINT('Ctrl Pts',(4.80530944735878,-1.05779126110086,33.4545053425731));
#30160=CARTESIAN_POINT('Ctrl Pts',(4.83213908119947,-0.916305059707026,
33.4626597837685));
#30161=CARTESIAN_POINT('Ctrl Pts',(4.85897532826281,-0.774783983452207,
33.4708162349479));
#30162=CARTESIAN_POINT('Ctrl Pts',(4.87958802770654,-0.63209418158598,33.4789726861274));
#30163=CARTESIAN_POINT('Ctrl Pts',(4.89390047547349,-0.488795661458185,
33.4871291373068));
#30164=CARTESIAN_POINT('Ctrl Pts',(4.90366254873117,-0.391056219960537,
33.4926923977102));
#30165=CARTESIAN_POINT('Ctrl Pts',(4.9104947018656,-0.2930337819537,33.4982556581135));
#30166=CARTESIAN_POINT('Ctrl Pts',(4.91438645268894,-0.194907301370204,
33.5038189185168));
#30167=CARTESIAN_POINT('Ctrl Pts',(4.92009214692821,-0.0510441096090894,
33.5119752122457));
#30168=CARTESIAN_POINT('Ctrl Pts',(4.91947741697528,0.0930967253521199,
33.5201315059745));
#30169=CARTESIAN_POINT('Ctrl Pts',(4.91253881611527,0.236950295760079,33.5282877997034));
#30170=CARTESIAN_POINT('Ctrl Pts',(4.90560162944995,0.380774546574776,33.5364424310529));
#30171=CARTESIAN_POINT('Ctrl Pts',(4.89234315927421,0.524311315575884,33.5445970624023));
#30172=CARTESIAN_POINT('Ctrl Pts',(4.87281202951924,0.666997741729757,33.5527516937518));
#30173=CARTESIAN_POINT('Ctrl Pts',(4.85328020686642,0.809689229911189,33.5609066143997));
#30174=CARTESIAN_POINT('Ctrl Pts',(4.82747532100132,0.951529982823226,33.5690615350477));
#30175=CARTESIAN_POINT('Ctrl Pts',(4.79549769678287,1.09196378266416,33.5772164556956));
#30176=CARTESIAN_POINT('Ctrl Pts',(4.76352195262564,1.23238932597733,33.5853708968911));
#30177=CARTESIAN_POINT('Ctrl Pts',(4.72537427139847,1.37140775560834,33.5935253380866));
#30178=CARTESIAN_POINT('Ctrl Pts',(4.68120577034772,1.50847459314474,33.6016797792821));
#30179=CARTESIAN_POINT('Ctrl Pts',(4.63702638222589,1.64557521621536,33.6098362304617));
#30180=CARTESIAN_POINT('Ctrl Pts',(4.58682331124454,1.78072296721192,33.6179926816412));
#30181=CARTESIAN_POINT('Ctrl Pts',(4.53079726874191,1.91338944599914,33.6261491328207));
#30182=CARTESIAN_POINT('Ctrl Pts',(4.49258365636061,2.00387710441492,33.6317123932235));
#30183=CARTESIAN_POINT('Ctrl Pts',(4.4516621236224,2.09321077570324,33.6372756536263));
#30184=CARTESIAN_POINT('Ctrl Pts',(4.40810912660491,2.18122832148368,33.6428389140291));
#30185=CARTESIAN_POINT('Ctrl Pts',(4.34425609605752,2.3102708082078,33.6509952077579));
#30186=CARTESIAN_POINT('Ctrl Pts',(4.27472085740843,2.43653168410303,33.6591515014867));
#30187=CARTESIAN_POINT('Ctrl Pts',(4.19977078733812,2.55951331239384,33.6673077952155));
#30188=CARTESIAN_POINT('Ctrl Pts',(4.12483599325682,2.68246987511768,33.6754624265649));
#30189=CARTESIAN_POINT('Ctrl Pts',(4.04448874347453,2.80214823798555,33.6836170579143));
#30190=CARTESIAN_POINT('Ctrl Pts',(3.95904115281108,2.91807748575124,33.6917716892636));
#30191=CARTESIAN_POINT('Ctrl Pts',(3.87359053075878,3.03401084629094,33.6999266099115));
#30192=CARTESIAN_POINT('Ctrl Pts',(3.78303940127665,3.1461945539773,33.7080815305594));
#30193=CARTESIAN_POINT('Ctrl Pts',(3.68774209251233,3.2541882738423,33.7162364512073));
#30194=CARTESIAN_POINT('Ctrl Pts',(3.59245038656494,3.36217564442998,33.7243908924027));
#30195=CARTESIAN_POINT('Ctrl Pts',(3.49241328173855,3.46597326972859,33.7325453335981));
#30196=CARTESIAN_POINT('Ctrl Pts',(3.38802408244951,3.5651754345673,33.7406997747935));
#30197=CARTESIAN_POINT('Ctrl Pts',(3.28360915232045,3.66440205169659,33.748856225973));
#30198=CARTESIAN_POINT('Ctrl Pts',(3.17484022667796,3.75903071410694,33.7570126771524));
#30199=CARTESIAN_POINT('Ctrl Pts',(3.06214645722417,3.84869356236755,33.7651691283319));
#30200=CARTESIAN_POINT('Ctrl Pts',(2.98528155954885,3.90984978857451,33.7707323887352));
#30201=CARTESIAN_POINT('Ctrl Pts',(2.90659149361485,3.96869662529929,33.7762956491385));
#30202=CARTESIAN_POINT('Ctrl Pts',(2.8262209979243,4.02512831266182,33.7818589095418));
#30203=CARTESIAN_POINT('Ctrl Pts',(2.70838984811907,4.1078627856826,33.7900152032706));
#30204=CARTESIAN_POINT('Ctrl Pts',(2.58690120655491,4.18543512719117,33.7981714969995));
#30205=CARTESIAN_POINT('Ctrl Pts',(2.46222803144597,4.2575363983954,33.8063277907284));
#30206=CARTESIAN_POINT('Ctrl Pts',(2.33758026666753,4.32962297424012,33.8144824220779));
#30207=CARTESIAN_POINT('Ctrl Pts',(2.20974955269506,4.39624053687945,33.8226370534273));
#30208=CARTESIAN_POINT('Ctrl Pts',(2.07923533694281,4.457125023612,33.8307916847768));
#30209=CARTESIAN_POINT('Ctrl Pts',(1.94871649099163,4.51801167031835,33.8389466054247));
#30210=CARTESIAN_POINT('Ctrl Pts',(1.81551425443547,4.57316468925295,33.8471015260727));
#30211=CARTESIAN_POINT('Ctrl Pts',(1.68015050005635,4.62236707322779,33.8552564467206));
#30212=CARTESIAN_POINT('Ctrl Pts',(1.54479470412168,4.67156656444568,33.8634108879161));
#30213=CARTESIAN_POINT('Ctrl Pts',(1.40727795946292,4.71481600719977,33.8715653291117));
#30214=CARTESIAN_POINT('Ctrl Pts',(1.26813978851806,4.75194744702394,33.8797197703072));
#30215=CARTESIAN_POINT('Ctrl Pts',(1.12896732147702,4.78908803935762,33.8878762214867));
#30216=CARTESIAN_POINT('Ctrl Pts',(0.988172952954542,4.82010752884014,33.8960326726662));
#30217=CARTESIAN_POINT('Ctrl Pts',(0.846309558868826,4.84488835713138,33.9041891238457));
#30218=CARTESIAN_POINT('Ctrl Pts',(0.749548971996745,4.8617905855328,33.9097523842485));
#30219=CARTESIAN_POINT('Ctrl Pts',(0.652291323342216,4.87579152998842,33.9153156446513));
#30220=CARTESIAN_POINT('Ctrl Pts',(0.55471431658077,4.88686761530127,33.9208789050541));
#30221=CARTESIAN_POINT('Ctrl Pts',(0.411656708146348,4.90310625930421,33.9290351987829));
#30222=CARTESIAN_POINT('Ctrl Pts',(0.267858778981811,4.91306184888029,33.9371914925117));
#30223=CARTESIAN_POINT('Ctrl Pts',(0.123883663578513,4.91668952654104,33.9453477862405));
#30224=CARTESIAN_POINT('Ctrl Pts',(-0.0200621074589962,4.92031646482472,
33.9535024175899));
#30225=CARTESIAN_POINT('Ctrl Pts',(-0.164184658347153,4.91761805569537,
33.9616570489393));
#30226=CARTESIAN_POINT('Ctrl Pts',(-0.307919077891934,4.90860152222302,
33.9698116802887));
#30227=CARTESIAN_POINT('Ctrl Pts',(-0.451658596643225,4.89958466887484,
33.9779666009366));
#30228=CARTESIAN_POINT('Ctrl Pts',(-0.595009622280352,4.88424925986398,
33.9861215215845));
#30229=CARTESIAN_POINT('Ctrl Pts',(-0.737410078155,4.86265456712025,33.9942764422323));
#30230=CARTESIAN_POINT('Ctrl Pts',(-0.87980216187628,4.84106114399381,34.0024308834278));
#30231=CARTESIAN_POINT('Ctrl Pts',(-1.0212434569048,4.81320922448485,34.0105853246232));
#30232=CARTESIAN_POINT('Ctrl Pts',(-1.16117987019393,4.77920959694764,34.0187397658186));
#30233=CARTESIAN_POINT('Ctrl Pts',(-1.30115077633757,4.74520158885973,34.0268962169981));
#30234=CARTESIAN_POINT('Ctrl Pts',(-1.4396157341306,4.70504292356356,34.0350526681775));
#30235=CARTESIAN_POINT('Ctrl Pts',(-1.57603304919831,4.65889502890274,34.043209119357));
#30236=CARTESIAN_POINT('Ctrl Pts',(-1.66907903580995,4.62741899239935,34.0487723797603));
#30237=CARTESIAN_POINT('Ctrl Pts',(-1.76117269102492,4.59315771194547,34.0543356401636));
#30238=CARTESIAN_POINT('Ctrl Pts',(-1.8521467069881,4.55617554954735,34.0598989005668));
#30239=CARTESIAN_POINT('Ctrl Pts',(-1.98552367338919,4.50195601686662,34.0680551942957));
#30240=CARTESIAN_POINT('Ctrl Pts',(-2.11654314582965,4.4418656179856,34.0762114880246));
#30241=CARTESIAN_POINT('Ctrl Pts',(-2.24468922246724,4.37613452227413,34.0843677817535));
#30242=CARTESIAN_POINT('Ctrl Pts',(-2.37280918094275,4.31041682358157,34.0925224131029));
#30243=CARTESIAN_POINT('Ctrl Pts',(-2.49805661435159,4.23906087420696,34.1006770444524));
#30244=CARTESIAN_POINT('Ctrl Pts',(-2.61993899017471,4.16234342050993,34.1088316758018));
#30245=CARTESIAN_POINT('Ctrl Pts',(-2.74182568996874,4.08562324513935,34.1169865964498));
#30246=CARTESIAN_POINT('Ctrl Pts',(-2.86034680808497,4.00354135991706,34.1251415170977));
#30247=CARTESIAN_POINT('Ctrl Pts',(-2.97503721481366,3.91641885310724,34.1332964377457));
#30248=CARTESIAN_POINT('Ctrl Pts',(-3.08972087854659,3.82930146849298,34.1414508789412));
#30249=CARTESIAN_POINT('Ctrl Pts',(-3.20057401555088,3.73714425837669,34.1496053201367));
#30250=CARTESIAN_POINT('Ctrl Pts',(-3.30716316491905,3.64030972076589,34.1577597613322));
#30251=CARTESIAN_POINT('Ctrl Pts',(-3.41377858739181,3.54345131445973,34.1659162125117));
#30252=CARTESIAN_POINT('Ctrl Pts',(-3.51612767407156,3.44191350184174,34.1740726636912));
#30253=CARTESIAN_POINT('Ctrl Pts',(-3.61381208950851,3.33609730736712,34.1822291148708));
#30254=CARTESIAN_POINT('Ctrl Pts',(-3.68043957594954,3.26392338862007,34.1877923752735));
#30255=CARTESIAN_POINT('Ctrl Pts',(-3.74489771362711,3.18975988577272,34.1933556356764));
#30256=CARTESIAN_POINT('Ctrl Pts',(-3.80707041484449,3.11374339323519,34.1989188960792));
#30257=CARTESIAN_POINT('Ctrl Pts',(-3.89822110671353,3.00229647597761,34.2070751290372));
#30258=CARTESIAN_POINT('Ctrl Pts',(-3.98449180843724,2.88682347498688,34.2152313619953));
#30259=CARTESIAN_POINT('Ctrl Pts',(-4.06553974214529,2.76777341333015,34.2233875949534));
#30260=CARTESIAN_POINT('Ctrl Pts',(-4.14658036526241,2.64873409008785,34.2315430922125));
#30261=CARTESIAN_POINT('Ctrl Pts',(-4.22239896825741,2.52611862391255,34.2396985894717));
#30262=CARTESIAN_POINT('Ctrl Pts',(-4.29269548527147,2.40040591009728,34.2478540867308));
#30263=CARTESIAN_POINT('Ctrl Pts',(-4.36298184084889,2.27471136818909,34.256008405104));
#30264=CARTESIAN_POINT('Ctrl Pts',(-4.42774754135432,2.14592076487399,34.2641627234773));
#30265=CARTESIAN_POINT('Ctrl Pts',(-4.4867379583526,2.01453854656048,34.2723170418506));
#30266=CARTESIAN_POINT('Ctrl Pts',(-4.54573832761712,1.88313416276849,34.2804727359379));
#30267=CARTESIAN_POINT('Ctrl Pts',(-4.59896132667297,1.74913759456132,34.2886284300253));
#30268=CARTESIAN_POINT('Ctrl Pts',(-4.64619980387587,1.61307484171189,34.2967841241126));
#30269=CARTESIAN_POINT('Ctrl Pts',(-4.69087538718258,1.48439408801705,34.3044973361423));
#30270=CARTESIAN_POINT('Ctrl Pts',(-4.73019850764378,1.35386565993627,34.312210548172));
#30271=CARTESIAN_POINT('Ctrl Pts',(-4.76403458704967,1.22194824599671,34.3199237602016));
#30272=CARTESIAN_POINT('Origin',(0.,0.,-3.23514056400928));
#30273=CARTESIAN_POINT('',(-4.76403458704968,1.22194824599668,36.4152130395234));
#30274=CARTESIAN_POINT('',(-4.76403458739297,1.22194824465831,36.0696927553338));
#30275=CARTESIAN_POINT('',(-4.76403458704967,1.22194824599672,-3.23514056400928));
#30276=CARTESIAN_POINT('',(-4.91824999894343,0.000101945896325419,34.7351405653851));
#30277=CARTESIAN_POINT('Ctrl Pts',(-4.91824999894343,0.000101945896325419,
34.7351405653851));
#30278=CARTESIAN_POINT('Ctrl Pts',(-4.91825297185789,-0.14332252814081,
34.7432643671499));
#30279=CARTESIAN_POINT('Ctrl Pts',(-4.91197785217775,-0.286773541245251,
34.7513881689147));
#30280=CARTESIAN_POINT('Ctrl Pts',(-4.89944373927689,-0.429690712211137,
34.7595119706796));
#30281=CARTESIAN_POINT('Ctrl Pts',(-4.88690997830694,-0.57260387037042,
34.7676355443455));
#30282=CARTESIAN_POINT('Ctrl Pts',(-4.86811759880276,-0.714982877260633,
34.7757591180115));
#30283=CARTESIAN_POINT('Ctrl Pts',(-4.84313767764064,-0.856271275891921,
34.7838826916774));
#30284=CARTESIAN_POINT('Ctrl Pts',(-4.81816023339163,-0.99754566490791,
34.792005459841));
#30285=CARTESIAN_POINT('Ctrl Pts',(-4.78699653311575,-1.13772932710976,
34.8001282280046));
#30286=CARTESIAN_POINT('Ctrl Pts',(-4.74976898696445,-1.27627490493652,
34.8082509961681));
#30287=CARTESIAN_POINT('Ctrl Pts',(-4.71253137452548,-1.41485794533563,
34.8163759607193));
#30288=CARTESIAN_POINT('Ctrl Pts',(-4.66922672622055,-1.55180168728186,
34.8245009252705));
#30289=CARTESIAN_POINT('Ctrl Pts',(-4.62002782714359,-1.6865722453897,34.8326258898216));
#30290=CARTESIAN_POINT('Ctrl Pts',(-4.57518222622321,-1.80941781263029,
34.8400319278548));
#30291=CARTESIAN_POINT('Ctrl Pts',(-4.52543997650175,-1.93045775236507,
34.847437965888));
#30292=CARTESIAN_POINT('Ctrl Pts',(-4.47096718960992,-2.04930121064024,
34.8548440039212));
#30293=CARTESIAN_POINT('Ctrl Pts',(-4.41097510319836,-2.18018614282575,
34.8630004376013));
#30294=CARTESIAN_POINT('Ctrl Pts',(-4.34522048768164,-2.30845937613391,
34.8711568712814));
#30295=CARTESIAN_POINT('Ctrl Pts',(-4.27395583508463,-2.43361553706539,
34.8793133049615));
#30296=CARTESIAN_POINT('Ctrl Pts',(-4.20270568685358,-2.55874622518958,
34.8874680785773));
#30297=CARTESIAN_POINT('Ctrl Pts',(-4.12594790424494,-2.68076081593636,
34.8956228521932));
#30298=CARTESIAN_POINT('Ctrl Pts',(-4.04398049103538,-2.79917931734022,
34.9037776258091));
#30299=CARTESIAN_POINT('Ctrl Pts',(-3.96201017100346,-2.9176020182367,34.911932688619));
#30300=CARTESIAN_POINT('Ctrl Pts',(-3.87483003804373,-3.03242809733651,
34.9200877514288));
#30301=CARTESIAN_POINT('Ctrl Pts',(-3.7827811984389,-3.14320687630279,34.9282428142386));
#30302=CARTESIAN_POINT('Ctrl Pts',(-3.69073775749174,-3.25397915810184,
34.9363973987546));
#30303=CARTESIAN_POINT('Ctrl Pts',(-3.59382639577598,-3.36070435789163,
34.9445519832706));
#30304=CARTESIAN_POINT('Ctrl Pts',(-3.49242820674477,-3.46296524430054,
34.9527065677866));
#30305=CARTESIAN_POINT('Ctrl Pts',(-3.39100508746049,-3.56525127306951,
34.9608631572285));
#30306=CARTESIAN_POINT('Ctrl Pts',(-3.28509317207918,-3.66307055729281,
34.9690197466704));
#30307=CARTESIAN_POINT('Ctrl Pts',(-3.17511050902387,-3.75604264059744,
34.9771763361123));
#30308=CARTESIAN_POINT('Ctrl Pts',(-3.10043641407023,-3.81916719117534,
34.9827143538103));
#30309=CARTESIAN_POINT('Ctrl Pts',(-3.02388650556722,-3.88005800371298,
34.9882523715084));
#30310=CARTESIAN_POINT('Ctrl Pts',(-2.94560038055085,-3.93860653792667,
34.9937903892065));
#30311=CARTESIAN_POINT('Ctrl Pts',(-2.83029999301516,-4.02483725483945,
35.0019468228866));
#30312=CARTESIAN_POINT('Ctrl Pts',(-2.71118892597505,-4.10601758221992,
35.0101032565667));
#30313=CARTESIAN_POINT('Ctrl Pts',(-2.58873068694449,-4.1818245411509,35.0182596902468));
#30314=CARTESIAN_POINT('Ctrl Pts',(-2.46629737161713,-4.25761607122907,
35.0264144638627));
#30315=CARTESIAN_POINT('Ctrl Pts',(-2.34051852769332,-4.3280362385645,35.0345692374786));
#30316=CARTESIAN_POINT('Ctrl Pts',(-2.21188548417436,-4.39280612677122,
35.0427240110946));
#30317=CARTESIAN_POINT('Ctrl Pts',(-2.0832478789233,-4.45757831192178,35.0508790739044));
#30318=CARTESIAN_POINT('Ctrl Pts',(-1.95175616871635,-4.51669966315225,
35.0590341367143));
#30319=CARTESIAN_POINT('Ctrl Pts',(-1.81792550717558,-4.56993762680197,
35.0671891995241));
#30320=CARTESIAN_POINT('Ctrl Pts',(-1.68410269479296,-4.62317246804915,
35.0753437840402));
#30321=CARTESIAN_POINT('Ctrl Pts',(-1.54794151681425,-4.67052448924647,
35.0834983685562));
#30322=CARTESIAN_POINT('Ctrl Pts',(-1.40997623830103,-4.71180963854934,
35.0916529530722));
#30323=CARTESIAN_POINT('Ctrl Pts',(-1.2719770389722,-4.75310493842018,35.0998095425142));
#30324=CARTESIAN_POINT('Ctrl Pts',(-1.13217317343178,-4.78833028960078,
35.1079661319561));
#30325=CARTESIAN_POINT('Ctrl Pts',(-0.99111376328778,-4.81735161377302,
35.116122721398));
#30326=CARTESIAN_POINT('Ctrl Pts',(-0.895339724961226,-4.83705600223404,
35.1216607390959));
#30327=CARTESIAN_POINT('Ctrl Pts',(-0.798987190987151,-4.85390143898352,
35.1271987567937));
#30328=CARTESIAN_POINT('Ctrl Pts',(-0.702230674208628,-4.86785940046552,
35.1327367744915));
#30329=CARTESIAN_POINT('Ctrl Pts',(-0.55972695622198,-4.88841679001326,
35.1408932081716));
#30330=CARTESIAN_POINT('Ctrl Pts',(-0.41629327802585,-4.90271615377631,
35.1490496418517));
#30331=CARTESIAN_POINT('Ctrl Pts',(-0.272491180651915,-4.91069563493472,
35.1572060755317));
#30332=CARTESIAN_POINT('Ctrl Pts',(-0.128718351058837,-4.91867349204376,
35.1653608491476));
#30333=CARTESIAN_POINT('Ctrl Pts',(0.0154224142110825,-4.92033401406274,
35.1735156227635));
#30334=CARTESIAN_POINT('Ctrl Pts',(0.159366224511822,-4.91566734726678,
35.1816703963793));
#30335=CARTESIAN_POINT('Ctrl Pts',(0.303315139513225,-4.91100051497613,
35.1898254591892));
#30336=CARTESIAN_POINT('Ctrl Pts',(0.447066751008784,-4.90000605197425,
35.197980521999));
#30337=CARTESIAN_POINT('Ctrl Pts',(0.590057428971841,-4.88272621524238,
35.2061355848088));
#30338=CARTESIAN_POINT('Ctrl Pts',(0.733039720541969,-4.86544739197168,
35.2142901693248));
#30339=CARTESIAN_POINT('Ctrl Pts',(0.87526083575672,-4.84188397357044,35.2224447538407));
#30340=CARTESIAN_POINT('Ctrl Pts',(1.01616356737732,-4.81212995115832,35.2305993383567));
#30341=CARTESIAN_POINT('Ctrl Pts',(1.15710094203062,-4.78236861327716,35.2387559277986));
#30342=CARTESIAN_POINT('Ctrl Pts',(1.29671895777609,-4.74641369894058,35.2469125172405));
#30343=CARTESIAN_POINT('Ctrl Pts',(1.43447127059977,-4.70441019005825,35.2550691066824));
#30344=CARTESIAN_POINT('Ctrl Pts',(1.52799991413489,-4.67589138606177,35.2606071243805));
#30345=CARTESIAN_POINT('Ctrl Pts',(1.62066872458696,-4.64458529858958,35.2661451420786));
#30346=CARTESIAN_POINT('Ctrl Pts',(1.7123108115699,-4.6105503735542,35.2716831597767));
#30347=CARTESIAN_POINT('Ctrl Pts',(1.84728195928515,-4.56042348267184,35.2798395934567));
#30348=CARTESIAN_POINT('Ctrl Pts',(1.98007566607134,-4.50435635074101,35.2879960271368));
#30349=CARTESIAN_POINT('Ctrl Pts',(2.11016923544657,-4.44256332090774,35.2961524608169));
#30350=CARTESIAN_POINT('Ctrl Pts',(2.24023632711345,-4.38078286769782,35.3043072344328));
#30351=CARTESIAN_POINT('Ctrl Pts',(2.36760407561693,-4.31327898494002,35.3124620080487));
#30352=CARTESIAN_POINT('Ctrl Pts',(2.49177172321678,-4.24031328345881,35.3206167816646));
#30353=CARTESIAN_POINT('Ctrl Pts',(2.61594377419179,-4.16734499438443,35.3287718444745));
#30354=CARTESIAN_POINT('Ctrl Pts',(2.73691520678645,-4.0889146652997,35.3369269072843));
#30355=CARTESIAN_POINT('Ctrl Pts',(2.85421130183859,-4.00532906350488,35.3450819700941));
#30356=CARTESIAN_POINT('Ctrl Pts',(2.9715005174835,-3.92174836399937,35.3532365546101));
#30357=CARTESIAN_POINT('Ctrl Pts',(3.08511455486701,-3.83301319166472,35.3613911391261));
#30358=CARTESIAN_POINT('Ctrl Pts',(3.19460908625978,-3.73947266984082,35.3695457236421));
#30359=CARTESIAN_POINT('Ctrl Pts',(3.3041305385117,-3.64590914968833,35.377702313084));
#30360=CARTESIAN_POINT('Ctrl Pts',(3.40953020620542,-3.54753813649967,35.3858589025259));
#30361=CARTESIAN_POINT('Ctrl Pts',(3.51039769664934,-3.44474833244158,35.3940154919678));
#30362=CARTESIAN_POINT('Ctrl Pts',(3.57888293195628,-3.37495791843314,35.3995535096658));
#30363=CARTESIAN_POINT('Ctrl Pts',(3.6452795935013,-3.30313130164868,35.4050915273638));
#30364=CARTESIAN_POINT('Ctrl Pts',(3.70946909361247,-3.229399651024,35.4106295450617));
#30365=CARTESIAN_POINT('Ctrl Pts',(3.80400786708083,-3.12080712726568,35.4187859787418));
#30366=CARTESIAN_POINT('Ctrl Pts',(3.8937925591734,-3.00804010677295,35.4269424124219));
#30367=CARTESIAN_POINT('Ctrl Pts',(3.97846672749768,-2.89153688558419,35.435098846102));
#30368=CARTESIAN_POINT('Ctrl Pts',(4.06312366224199,-2.77505737608482,35.4432536197179));
#30369=CARTESIAN_POINT('Ctrl Pts',(4.14267195161278,-2.65484345341187,35.4514083933338));
#30370=CARTESIAN_POINT('Ctrl Pts',(4.21679703265162,-2.53136442416348,35.4595631669497));
#30371=CARTESIAN_POINT('Ctrl Pts',(4.2909247423989,-2.40788101596046,35.4677182297596));
#30372=CARTESIAN_POINT('Ctrl Pts',(4.35962868353461,-2.281132554444,35.4758732925694));
#30373=CARTESIAN_POINT('Ctrl Pts',(4.42263876262049,-2.15161554137042,35.4840283553792));
#30374=CARTESIAN_POINT('Ctrl Pts',(4.48564514616972,-2.02210612446042,35.4921829398952));
#30375=CARTESIAN_POINT('Ctrl Pts',(4.5429581902288,-1.88982878218134,35.5003375244112));
#30376=CARTESIAN_POINT('Ctrl Pts',(4.59435475339333,-1.75530266976156,35.5084921089272));
#30377=CARTESIAN_POINT('Ctrl Pts',(4.64576395316754,-1.62074348209575,35.5166486983691));
#30378=CARTESIAN_POINT('Ctrl Pts',(4.69125364563663,-1.48393473213877,35.524805287811));
#30379=CARTESIAN_POINT('Ctrl Pts',(4.73064942443394,-1.34541409447159,35.5329618772529));
#30380=CARTESIAN_POINT('Ctrl Pts',(4.7573976777033,-1.25136378724406,35.5384998949509));
#30381=CARTESIAN_POINT('Ctrl Pts',(4.78133771546532,-1.15652469121814,35.5440379126489));
#30382=CARTESIAN_POINT('Ctrl Pts',(4.80242815902273,-1.06106872535455,35.5495759303469));
#30383=CARTESIAN_POINT('Ctrl Pts',(4.83349032125123,-0.920480468437998,
35.557732364027));
#30384=CARTESIAN_POINT('Ctrl Pts',(4.85838058965853,-0.778501010826628,
35.5658887977071));
#30385=CARTESIAN_POINT('Ctrl Pts',(4.87699566032415,-0.635685764886574,
35.5740452313871));
#30386=CARTESIAN_POINT('Ctrl Pts',(4.89560694229816,-0.492899585874827,
35.5822000050031));
#30387=CARTESIAN_POINT('Ctrl Pts',(4.90794553120562,-0.349278289508366,
35.590354778619));
#30388=CARTESIAN_POINT('Ctrl Pts',(4.91395973495841,-0.20538448263561,35.5985095522349));
#30389=CARTESIAN_POINT('Ctrl Pts',(4.91997415199377,-0.0614855728359807,
35.6066646150447));
#30390=CARTESIAN_POINT('Ctrl Pts',(4.91966371736256,0.0826855326418441,
35.6148196778545));
#30391=CARTESIAN_POINT('Ctrl Pts',(4.91302879980008,0.226563622046861,35.6229747406644));
#30392=CARTESIAN_POINT('Ctrl Pts',(4.906394271375,0.370433273012985,35.6311293251804));
#30393=CARTESIAN_POINT('Ctrl Pts',(4.8934360184806,0.514009608047258,35.6392839096964));
#30394=CARTESIAN_POINT('Ctrl Pts',(4.87420647772475,0.656729986376489,35.6474384942125));
#30395=CARTESIAN_POINT('Ctrl Pts',(4.85497220910031,0.799485454633476,35.6555950836544));
#30396=CARTESIAN_POINT('Ctrl Pts',(4.82946361606154,0.941384213849286,35.6637516730963));
#30397=CARTESIAN_POINT('Ctrl Pts',(4.79778479087673,1.08187067754511,35.6719082625382));
#30398=CARTESIAN_POINT('Ctrl Pts',(4.77627605909945,1.17725570676714,35.6774462802361));
#30399=CARTESIAN_POINT('Ctrl Pts',(4.75192398480672,1.27198984011147,35.6829842979341));
#30400=CARTESIAN_POINT('Ctrl Pts',(4.72477448451324,1.36590231458644,35.688522315632));
#30401=CARTESIAN_POINT('Ctrl Pts',(4.68478849843133,1.50421730590053,35.6966787493121));
#30402=CARTESIAN_POINT('Ctrl Pts',(4.63871723203097,1.64080109065291,35.7048351829922));
#30403=CARTESIAN_POINT('Ctrl Pts',(4.58673570064337,1.77511652432834,35.7129916166723));
#30404=CARTESIAN_POINT('Ctrl Pts',(4.53476474896289,1.90940462102638,35.7211463902882));
#30405=CARTESIAN_POINT('Ctrl Pts',(4.47688605272524,2.04142497577482,35.7293011639041));
#30406=CARTESIAN_POINT('Ctrl Pts',(4.41332339088377,2.17065881933991,35.73745593752));
#30407=CARTESIAN_POINT('Ctrl Pts',(4.34975847491045,2.29989724594348,35.7456110003298));
#30408=CARTESIAN_POINT('Ctrl Pts',(4.28050933430343,2.42634866171021,35.7537660631396));
#30409=CARTESIAN_POINT('Ctrl Pts',(4.20584671009077,2.54951691771572,35.7619211259494));
#30410=CARTESIAN_POINT('Ctrl Pts',(4.13118846483564,2.67267794991188,35.7700757104653));
#30411=CARTESIAN_POINT('Ctrl Pts',(4.05111754546079,2.79255592190872,35.7782302949813));
#30412=CARTESIAN_POINT('Ctrl Pts',(3.96594918493528,2.90868185352252,35.7863848794973));
#30413=CARTESIAN_POINT('Ctrl Pts',(3.88075988450122,3.02483633642429,35.7945414689391));
#30414=CARTESIAN_POINT('Ctrl Pts',(3.79047083639418,3.13723666550547,35.802698058381));
#30415=CARTESIAN_POINT('Ctrl Pts',(3.6954392585745,3.24544476900876,35.8108546478229));
#30416=CARTESIAN_POINT('Ctrl Pts',(3.63091638861855,3.31891400471662,35.816392665521));
#30417=CARTESIAN_POINT('Ctrl Pts',(3.56420812623701,3.39045131857025,35.8219306832191));
#30418=CARTESIAN_POINT('Ctrl Pts',(3.49543649080652,3.45992872776856,35.8274687009172));
#30419=CARTESIAN_POINT('Ctrl Pts',(3.39414911434074,3.56225557309202,35.8356251345972));
#30420=CARTESIAN_POINT('Ctrl Pts',(3.28834638458959,3.66015079372222,35.8437815682773));
#30421=CARTESIAN_POINT('Ctrl Pts',(3.17843897538824,3.75322644430534,35.8519380019574));
#30422=CARTESIAN_POINT('Ctrl Pts',(3.0685539354429,3.84628315136982,35.8600927755733));
#30423=CARTESIAN_POINT('Ctrl Pts',(2.95456613786648,3.93452202913846,35.8682475491892));
#30424=CARTESIAN_POINT('Ctrl Pts',(2.8369202855612,4.01759459824798,35.8764023228051));
#30425=CARTESIAN_POINT('Ctrl Pts',(2.71927026116367,4.10067011337229,35.884557385615));
#30426=CARTESIAN_POINT('Ctrl Pts',(2.59796219362905,4.1785787571513,35.8927124484248));
#30427=CARTESIAN_POINT('Ctrl Pts',(2.47347120197562,4.2510143819443,35.9008675112347));
#30428=CARTESIAN_POINT('Ctrl Pts',(2.3489875117094,4.3234457583934,35.9090220957507));
#30429=CARTESIAN_POINT('Ctrl Pts',(2.22132156051851,4.39040459057065,35.9171766802667));
#30430=CARTESIAN_POINT('Ctrl Pts',(2.0909745383266,4.45162987484021,35.9253312647828));
#30431=CARTESIAN_POINT('Ctrl Pts',(1.96059546838083,4.51287021225642,35.9334878542247));
#30432=CARTESIAN_POINT('Ctrl Pts',(1.82753431316723,4.56837404238567,35.9416444436666));
#30433=CARTESIAN_POINT('Ctrl Pts',(1.69231434290758,4.61792759008727,35.9498010331085));
#30434=CARTESIAN_POINT('Ctrl Pts',(1.60050506480937,4.65157258670245,35.9553390508064));
#30435=CARTESIAN_POINT('Ctrl Pts',(1.5077010432793,4.68247554983713,35.9608770685043));
#30436=CARTESIAN_POINT('Ctrl Pts',(1.41407065780245,4.71058247324491,35.9664150862022));
#30437=CARTESIAN_POINT('Ctrl Pts',(1.27617112926228,4.75197855921538,35.9745715198823));
#30438=CARTESIAN_POINT('Ctrl Pts',(1.13642681146136,4.78732283014429,35.9827279535624));
#30439=CARTESIAN_POINT('Ctrl Pts',(0.995383933206272,4.81647110320563,35.9908843872425));
#30440=CARTESIAN_POINT('Ctrl Pts',(0.854369761154215,4.84561344377144,35.9990391608584));
#30441=CARTESIAN_POINT('Ctrl Pts',(0.712057883404491,4.86856223452924,36.0071939344742));
#30442=CARTESIAN_POINT('Ctrl Pts',(0.569005528542592,4.88522422934587,36.0153487080901));
#30443=CARTESIAN_POINT('Ctrl Pts',(0.425948100593104,4.90188681504938,36.0235037708999));
#30444=CARTESIAN_POINT('Ctrl Pts',(0.282150474919354,4.91226211624998,36.0316588337098));
#30445=CARTESIAN_POINT('Ctrl Pts',(0.13817633620382,4.9163086114089,36.0398138965196));
#30446=CARTESIAN_POINT('Ctrl Pts',(-0.00578935843962983,4.92035486924119,
36.0479684810357));
#30447=CARTESIAN_POINT('Ctrl Pts',(-0.149931210878958,4.91807305518458,
36.0561230655517));
#30448=CARTESIAN_POINT('Ctrl Pts',(-0.29368424145842,4.90947376292195,36.0642776500678));
#30449=CARTESIAN_POINT('Ctrl Pts',(-0.437472615858507,4.90087235639542,
36.0724342395097));
#30450=CARTESIAN_POINT('Ctrl Pts',(-0.580871643178157,4.88595038770334,
36.0805908289516));
#30451=CARTESIAN_POINT('Ctrl Pts',(-0.723319550325413,4.8647704869415,36.0887474183935));
#30452=CARTESIAN_POINT('Ctrl Pts',(-0.820036325938714,4.85039013028679,
36.0942854360915));
#30453=CARTESIAN_POINT('Ctrl Pts',(-0.916314722954619,4.83312601110554,
36.0998234537895));
#30454=CARTESIAN_POINT('Ctrl Pts',(-1.01198104501103,4.81301126396338,36.1053614714875));
#30455=CARTESIAN_POINT('Ctrl Pts',(-1.15287911609435,4.78338611467638,36.1135179051677));
#30456=CARTESIAN_POINT('Ctrl Pts',(-1.29250173701214,4.74756411622313,36.1216743388478));
#30457=CARTESIAN_POINT('Ctrl Pts',(-1.43030026963249,4.70567999349607,36.1298307725279));
#30458=CARTESIAN_POINT('Ctrl Pts',(-1.5680707563656,4.6638043953691,36.1379855461437));
#30459=CARTESIAN_POINT('Ctrl Pts',(-1.70401757545809,4.61586923161095,36.1461403197596));
#30460=CARTESIAN_POINT('Ctrl Pts',(-1.83760679953115,4.56205921846888,36.1542950933754));
#30461=CARTESIAN_POINT('Ctrl Pts',(-1.97120076109933,4.50824729705406,36.1624501561853));
#30462=CARTESIAN_POINT('Ctrl Pts',(-2.10243664856603,4.44856023090712,36.1706052189951));
#30463=CARTESIAN_POINT('Ctrl Pts',(-2.23079961217624,4.38323124564679,36.1787602818049));
#30464=CARTESIAN_POINT('Ctrl Pts',(-2.35915504730866,4.31790609192635,36.186914866321));
#30465=CARTESIAN_POINT('Ctrl Pts',(-2.48463759787963,4.246939833731,36.195069450837));
#30466=CARTESIAN_POINT('Ctrl Pts',(-2.60675621074842,4.1706120798061,36.2032240353531));
#30467=CARTESIAN_POINT('Ctrl Pts',(-2.72890484829438,4.09426555956771,36.211380624795));
#30468=CARTESIAN_POINT('Ctrl Pts',(-2.847687611455,4.01255508678855,36.2195372142369));
#30469=CARTESIAN_POINT('Ctrl Pts',(-2.96264115890128,3.92580443044277,36.2276938036788));
#30470=CARTESIAN_POINT('Ctrl Pts',(-3.0406902975429,3.86690399496428,36.2332318213767));
#30471=CARTESIAN_POINT('Ctrl Pts',(-3.11697479224663,3.80568099756497,36.2387698390746));
#30472=CARTESIAN_POINT('Ctrl Pts',(-3.1913579690167,3.74224763692806,36.2443078567726));
#30473=CARTESIAN_POINT('Ctrl Pts',(-3.30091006533164,3.64882251130377,36.2524642904526));
#30474=CARTESIAN_POINT('Ctrl Pts',(-3.40637736857711,3.55056601131062,36.2606207241326));
#30475=CARTESIAN_POINT('Ctrl Pts',(-3.50734256422543,3.44785892978129,36.2687771578127));
#30476=CARTESIAN_POINT('Ctrl Pts',(-3.60828721061027,3.34517275203831,36.2769319314285));
#30477=CARTESIAN_POINT('Ctrl Pts',(-3.7047313429311,3.23803803830448,36.2850867050444));
#30478=CARTESIAN_POINT('Ctrl Pts',(-3.79629448213534,3.12687244181926,36.2932414786603));
#30479=CARTESIAN_POINT('Ctrl Pts',(-3.88786086845674,3.01570290305203,36.3013965414701));
#30480=CARTESIAN_POINT('Ctrl Pts',(-3.97454569966372,2.90050245139121,36.3095516042799));
#30481=CARTESIAN_POINT('Ctrl Pts',(-4.05600845779462,2.78172220985462,36.3177066670897));
#30482=CARTESIAN_POINT('Ctrl Pts',(-4.13746643814055,2.66294893477077,36.3258612516057));
#30483=CARTESIAN_POINT('Ctrl Pts',(-4.21370276966811,2.54059656636371,36.3340158361216));
#30484=CARTESIAN_POINT('Ctrl Pts',(-4.28442002208921,2.41514557259414,36.3421704206376));
#30485=CARTESIAN_POINT('Ctrl Pts',(-4.35515466139905,2.28966373483112,36.3503270100795));
#30486=CARTESIAN_POINT('Ctrl Pts',(-4.42036734553155,2.16108204090106,36.3584835995213));
#30487=CARTESIAN_POINT('Ctrl Pts',(-4.47980610638382,2.02990647856156,36.3666401889632));
#30488=CARTESIAN_POINT('Ctrl Pts',(-4.52016279123364,1.94084320144363,36.3721782066614));
#30489=CARTESIAN_POINT('Ctrl Pts',(-4.55785870643562,1.85058469757476,36.3777162243595));
#30490=CARTESIAN_POINT('Ctrl Pts',(-4.59282751524086,1.75929488083905,36.3832542420577));
#30491=CARTESIAN_POINT('Ctrl Pts',(-4.6441959739934,1.62519202330009,36.3913894758108));
#30492=CARTESIAN_POINT('Ctrl Pts',(-4.68969766571455,1.48880998238945,36.3995247095639));
#30493=CARTESIAN_POINT('Ctrl Pts',(-4.72914863910647,1.35067990720875,36.407659943317));
#30494=CARTESIAN_POINT('Ctrl Pts',(-4.74135795832662,1.30793129958807,36.4101776420524));
#30495=CARTESIAN_POINT('Ctrl Pts',(-4.75298810446264,1.26501539330207,36.4126953407879));
#30496=CARTESIAN_POINT('Ctrl Pts',(-4.76403458704968,1.22194824599668,36.4152130395234));
#30497=CARTESIAN_POINT('Ctrl Pts',(-4.76374291154778,1.22187309174177,34.6652037882801));
#30498=CARTESIAN_POINT('Ctrl Pts',(-4.83809112144176,0.932844481302283,
34.6821017317321));
#30499=CARTESIAN_POINT('Ctrl Pts',(-4.90466058528984,0.52491922363429,34.7054139903085));
#30500=CARTESIAN_POINT('Ctrl Pts',(-4.91858708601659,0.113351080789942,
34.7287262488849));
#30501=CARTESIAN_POINT('Ctrl Pts',(-4.918482524436,0.000101975006558605,
34.7351405640093));
#30502=CARTESIAN_POINT('',(-4.91824999921026,8.81380467261397E-5,34.3898594359908));
#30503=CARTESIAN_POINT('Ctrl Pts',(-4.76403458704967,1.22194824599671,34.3199237602016));
#30504=CARTESIAN_POINT('Ctrl Pts',(-4.79037732700833,1.11924526762439,34.3259288039984));
#30505=CARTESIAN_POINT('Ctrl Pts',(-4.81339501831344,1.0157006926628,34.3319338477951));
#30506=CARTESIAN_POINT('Ctrl Pts',(-4.83304115288514,0.9115351211109,34.3379388915919));
#30507=CARTESIAN_POINT('Ctrl Pts',(-4.86135174302733,0.761429827249134,
34.3465923156584));
#30508=CARTESIAN_POINT('Ctrl Pts',(-4.88266723294743,0.609990304203609,
34.3552457397249));
#30509=CARTESIAN_POINT('Ctrl Pts',(-4.89689112312491,0.457865035529576,
34.3638991637913));
#30510=CARTESIAN_POINT('Ctrl Pts',(-4.91111501330238,0.305739766855543,
34.3725525878578));
#30511=CARTESIAN_POINT('Ctrl Pts',(-4.91824726020695,0.152929090369015,
34.3812060119243));
#30512=CARTESIAN_POINT('Ctrl Pts',(-4.91824999921026,8.81380467261397E-5,
34.3898594359908));
#30513=CARTESIAN_POINT('Ctrl Pts',(-4.91824999938303,7.79028443291767E-5,
34.3896774359301));
#30514=CARTESIAN_POINT('Ctrl Pts',(-4.91825074414469,-0.0469412282994122,
34.3923216676047));
#30515=CARTESIAN_POINT('Ctrl Pts',(-4.91757722521463,-0.0939577480454042,
34.3949691675867));
#30516=CARTESIAN_POINT('Ctrl Pts',(-4.91500835274931,-0.183553522053632,
34.4000241138427));
#30517=CARTESIAN_POINT('Ctrl Pts',(-4.91323348613992,-0.226131998448165,
34.4024305931114));
#30518=CARTESIAN_POINT('Ctrl Pts',(-4.90719185527896,-0.336559556576164,
34.4086854898363));
#30519=CARTESIAN_POINT('Ctrl Pts',(-4.90207131642267,-0.404352457993183,
34.4125389499999));
#30520=CARTESIAN_POINT('Ctrl Pts',(-4.88447473963195,-0.58685625090398,
34.4229573023208));
#30521=CARTESIAN_POINT('Ctrl Pts',(-4.86936491820749,-0.701269199383594,
34.4295369919425));
#30522=CARTESIAN_POINT('Ctrl Pts',(-4.82106155443031,-0.988717887391323,
34.446201637765));
#30523=CARTESIAN_POINT('Ctrl Pts',(-4.78256986429135,-1.16069948524653,
34.4562994768585));
#30524=CARTESIAN_POINT('Ctrl Pts',(-4.72291365775679,-1.37304253060127,
34.4688779055031));
#30525=CARTESIAN_POINT('Ctrl Pts',(-4.71031039376294,-1.41567484180246,
34.4714086792694));
#30526=CARTESIAN_POINT('Ctrl Pts',(-4.68674507289465,-1.49158668918534,
34.4759223949944));
#30527=CARTESIAN_POINT('Ctrl Pts',(-4.67600215783279,-1.52493084691938,
34.4779073461427));
#30528=CARTESIAN_POINT('Ctrl Pts',(-4.64717933540673,-1.61122229437934,
34.4830508795125));
#30529=CARTESIAN_POINT('Ctrl Pts',(-4.62855058951403,-1.66398095118079,
34.4862030395873));
#30530=CARTESIAN_POINT('Ctrl Pts',(-4.55118306562789,-1.87173361758746,
34.4986689023063));
#30531=CARTESIAN_POINT('Ctrl Pts',(-4.4855256519364,-2.02403417003301,34.507929636316));
#30532=CARTESIAN_POINT('Ctrl Pts',(-4.37437913226233,-2.24974670939476,
34.5220370575558));
#30533=CARTESIAN_POINT('Ctrl Pts',(-4.33444412179511,-2.32575730145814,
34.5268564192795));
#30534=CARTESIAN_POINT('Ctrl Pts',(-4.26128310972199,-2.45657281426278,
34.5352939920868));
#30535=CARTESIAN_POINT('Ctrl Pts',(-4.22893745168335,-2.51184626432518,
34.538905397353));
#30536=CARTESIAN_POINT('Ctrl Pts',(-4.17932890940758,-2.59294347892429,
34.5442792923364));
#30537=CARTESIAN_POINT('Ctrl Pts',(-4.16288573415952,-2.61926103492093,
34.5460352463685));
#30538=CARTESIAN_POINT('Ctrl Pts',(-4.11530054319865,-2.6938417747727,34.5510468622103));
#30539=CARTESIAN_POINT('Ctrl Pts',(-4.08356079159473,-2.74171720776653,
34.554306867514));
#30540=CARTESIAN_POINT('Ctrl Pts',(-3.94365473255752,-2.94492727599082,
34.5683372832408));
#30541=CARTESIAN_POINT('Ctrl Pts',(-3.82741036747741,-3.0945011581524,34.5791655424194));
#30542=CARTESIAN_POINT('Ctrl Pts',(-3.64930129493728,-3.29824191828655,
34.59465592058));
#30543=CARTESIAN_POINT('Ctrl Pts',(-3.59425339245277,-3.35814567455288,
34.5993096786689));
#30544=CARTESIAN_POINT('Ctrl Pts',(-3.52101267723659,-3.43398207957179,
34.6053257622797));
#30545=CARTESIAN_POINT('Ctrl Pts',(-3.50415331489639,-3.45118425311468,
34.6066990137477));
#30546=CARTESIAN_POINT('Ctrl Pts',(-3.45647102549121,-3.49912646949745,
34.6105500535178));
#30547=CARTESIAN_POINT('Ctrl Pts',(-3.42536517517964,-3.52958233706649,
34.6130243872956));
#30548=CARTESIAN_POINT('Ctrl Pts',(-3.39134947615652,-3.56201401099534,
34.6156883959412));
#30549=CARTESIAN_POINT('Ctrl Pts',(-3.38883753453079,-3.56440391209304,
34.6158848812093));
#30550=CARTESIAN_POINT('Ctrl Pts',(-3.35599358006014,-3.59558606874761,
34.6184507766804));
#30551=CARTESIAN_POINT('Ctrl Pts',(-3.32529782845277,-3.62399316905981,
34.62081346202));
#30552=CARTESIAN_POINT('Ctrl Pts',(-3.22467620665868,-3.71475757311403,
34.6284535313758));
#30553=CARTESIAN_POINT('Ctrl Pts',(-3.15332959417629,-3.77550966987126,
34.6337105129599));
#30554=CARTESIAN_POINT('Ctrl Pts',(-2.9723991507809,-3.92086469062726,34.6467198304326));
#30555=CARTESIAN_POINT('Ctrl Pts',(-2.86089735463021,-4.00294926583454,
34.6544611036323));
#30556=CARTESIAN_POINT('Ctrl Pts',(-2.68483018214487,-4.12144650700363,
34.6663770741605));
#30557=CARTESIAN_POINT('Ctrl Pts',(-2.62265734073695,-4.16128618960683,
34.6705289536987));
#30558=CARTESIAN_POINT('Ctrl Pts',(-2.50428681509076,-4.23342986445814,
34.6783438937375));
#30559=CARTESIAN_POINT('Ctrl Pts',(-2.44830150448164,-4.26605209723561,
34.6820037504808));
#30560=CARTESIAN_POINT('Ctrl Pts',(-2.33804144834147,-4.32741431101967,
34.6891486301119));
#30561=CARTESIAN_POINT('Ctrl Pts',(-2.28384046379989,-4.35626274096333,
34.692632129344));
#30562=CARTESIAN_POINT('Ctrl Pts',(-2.03488902598885,-4.48284346803885,
34.7085119069185));
#30563=CARTESIAN_POINT('Ctrl Pts',(-1.83431814494171,-4.56858111255541,
34.7209879871812));
#30564=CARTESIAN_POINT('Ctrl Pts',(-1.56534041689761,-4.66298245892528,
34.7372974480912));
#30565=CARTESIAN_POINT('Ctrl Pts',(-1.50150283873288,-4.68392841090857,
34.741137197226));
#30566=CARTESIAN_POINT('Ctrl Pts',(-1.4293050322267,-4.70598972660754,34.7454413219094));
#30567=CARTESIAN_POINT('Ctrl Pts',(-1.42134796902732,-4.70839910514521,
34.745915165219));
#30568=CARTESIAN_POINT('Ctrl Pts',(-1.40829187019663,-4.71231634591387,
34.7466917867901));
#30569=CARTESIAN_POINT('Ctrl Pts',(-1.40319643566884,-4.71383613404634,
34.7469946639745));
#30570=CARTESIAN_POINT('Ctrl Pts',(-1.39474115994718,-4.71634311964407,
34.7474968902665));
#30571=CARTESIAN_POINT('Ctrl Pts',(-1.39138271322317,-4.7173349966728,34.7476962803704));
#30572=CARTESIAN_POINT('Ctrl Pts',(-1.38574834577608,-4.71899249920192,
34.748030631234));
#30573=CARTESIAN_POINT('Ctrl Pts',(-1.38347299877258,-4.71966006689258,
34.748165609608));
#30574=CARTESIAN_POINT('Ctrl Pts',(-1.37961899918934,-4.72078777148888,
34.7483941625807));
#30575=CARTESIAN_POINT('Ctrl Pts',(-1.37804059744594,-4.72124876257932,
34.7484877451053));
#30576=CARTESIAN_POINT('Ctrl Pts',(-1.34066744397065,-4.73214370012445,
34.7507030762123));
#30577=CARTESIAN_POINT('Ctrl Pts',(-1.30475517350021,-4.74217114508611,
34.7528209325033));
#30578=CARTESIAN_POINT('Ctrl Pts',(-1.23427474626808,-4.7609894840203,34.7569545438997));
#30579=CARTESIAN_POINT('Ctrl Pts',(-1.19971812253121,-4.76981461600973,
34.7589704975439));
#30580=CARTESIAN_POINT('Ctrl Pts',(-0.988413008190155,-4.82133645570441,
34.7712418842116));
#30581=CARTESIAN_POINT('Ctrl Pts',(-0.809502653869499,-4.85458058385838,
34.7814005214382));
#30582=CARTESIAN_POINT('Ctrl Pts',(-0.53503184515812,-4.8899827937999,34.7969097036767));
#30583=CARTESIAN_POINT('Ctrl Pts',(-0.440571400842349,-4.89939663984047,
34.802232847028));
#30584=CARTESIAN_POINT('Ctrl Pts',(-0.2805173499409,-4.91068111455807,34.8112586686447));
#30585=CARTESIAN_POINT('Ctrl Pts',(-0.215051137126121,-4.91398330175008,
34.8149521171336));
#30586=CARTESIAN_POINT('Ctrl Pts',(-0.0971283758486763,-4.91757039098498,
34.8216159470215));
#30587=CARTESIAN_POINT('Ctrl Pts',(-0.0446959804318531,-4.91832641024141,
34.8245827596083));
#30588=CARTESIAN_POINT('Ctrl Pts',(0.0888433687528893,-4.91811630500611,
34.8321529104713));
#30589=CARTESIAN_POINT('Ctrl Pts',(0.169932281921091,-4.91598249892155,
34.8367630425071));
#30590=CARTESIAN_POINT('Ctrl Pts',(0.444079372031434,-4.90197719218596,
34.8524062061807));
#30591=CARTESIAN_POINT('Ctrl Pts',(0.636476855251575,-4.88072565023785,
34.863487525507));
#30592=CARTESIAN_POINT('Ctrl Pts',(0.887380490528332,-4.8379206236326,34.8780445052179));
#30593=CARTESIAN_POINT('Ctrl Pts',(0.947444544338079,-4.8265172761627,34.8815366919209));
#30594=CARTESIAN_POINT('Ctrl Pts',(1.01056458987187,-4.81331003865799,34.8852115037291));
#30595=CARTESIAN_POINT('Ctrl Pts',(1.01384777450257,-4.81261955786096,34.8854026627514));
#30596=CARTESIAN_POINT('Ctrl Pts',(1.01970547135941,-4.81138137568049,34.8857437432547));
#30597=CARTESIAN_POINT('Ctrl Pts',(1.02228025473819,-4.81083496613095,34.8858936753608));
#30598=CARTESIAN_POINT('Ctrl Pts',(1.0268914922173,-4.80985251987779,34.8861622064881));
#30599=CARTESIAN_POINT('Ctrl Pts',(1.02892811000402,-4.80941725619766,34.8862808120459));
#30600=CARTESIAN_POINT('Ctrl Pts',(1.07387820941106,-4.79978071209952,34.8888986578261));
#30601=CARTESIAN_POINT('Ctrl Pts',(1.11666724303579,-4.79000664106514,34.8913928347294));
#30602=CARTESIAN_POINT('Ctrl Pts',(1.19917343997252,-4.76999453458668,34.8962038056025));
#30603=CARTESIAN_POINT('Ctrl Pts',(1.23890463824402,-4.75982984340485,34.8985211206678));
#30604=CARTESIAN_POINT('Ctrl Pts',(1.38187652545527,-4.72134097149887,34.9068707506923));
#30605=CARTESIAN_POINT('Ctrl Pts',(1.484313719197,-4.69014462031996,34.9128742179225));
#30606=CARTESIAN_POINT('Ctrl Pts',(1.68434726808814,-4.62201557986683,34.924716213517));
#30607=CARTESIAN_POINT('Ctrl Pts',(1.78194848922946,-4.5852713408477,34.9305519340014));
#30608=CARTESIAN_POINT('Ctrl Pts',(1.95334612389233,-4.51444506211634,34.9409550618655));
#30609=CARTESIAN_POINT('Ctrl Pts',(2.02760457068747,-4.48158396551061,34.9455156362989));
#30610=CARTESIAN_POINT('Ctrl Pts',(2.16788278557622,-4.41530709007382,34.95425362842));
#30611=CARTESIAN_POINT('Ctrl Pts',(2.23402892831928,-4.3822102927466,34.9584278156849));
#30612=CARTESIAN_POINT('Ctrl Pts',(2.35512967413449,-4.31816180740378,34.9661813093189));
#30613=CARTESIAN_POINT('Ctrl Pts',(2.41028406758654,-4.28762029343483,34.9697567446153));
#30614=CARTESIAN_POINT('Ctrl Pts',(2.56959412290019,-4.19535746381459,34.9802210705023));
#30615=CARTESIAN_POINT('Ctrl Pts',(2.67207566435028,-4.13084122715434,34.9871283272968));
#30616=CARTESIAN_POINT('Ctrl Pts',(2.88045431370102,-3.98865667594585,35.0015560980037));
#30617=CARTESIAN_POINT('Ctrl Pts',(2.98583455478219,-3.91039526977784,35.0090739592291));
#30618=CARTESIAN_POINT('Ctrl Pts',(3.14475690520836,-3.78219675358706,35.0207430164225));
#30619=CARTESIAN_POINT('Ctrl Pts',(3.20052847828905,-3.73512060430727,35.0249057257574));
#30620=CARTESIAN_POINT('Ctrl Pts',(3.28338290054233,-3.66196532314146,35.0311862835869));
#30621=CARTESIAN_POINT('Ctrl Pts',(3.31124806450737,-3.63678836472118,35.0333154705501));
#30622=CARTESIAN_POINT('Ctrl Pts',(3.37721092763697,-3.57580239473911,35.0383963404359));
#30623=CARTESIAN_POINT('Ctrl Pts',(3.41503130954039,-3.53970022218039,35.0413435921193));
#30624=CARTESIAN_POINT('Ctrl Pts',(3.56877194759443,-3.38818614303303,35.0534874992304));
#30625=CARTESIAN_POINT('Ctrl Pts',(3.67947516945032,-3.26762938574615,35.0626282366291));
#30626=CARTESIAN_POINT('Ctrl Pts',(3.84108437563824,-3.07298697472029,35.0768102810035));
#30627=CARTESIAN_POINT('Ctrl Pts',(3.89631578321361,-3.00264903960497,35.0818279271654));
#30628=CARTESIAN_POINT('Ctrl Pts',(3.99600755078186,-2.86830469104892,35.0912425446493));
#30629=CARTESIAN_POINT('Ctrl Pts',(4.04092399201479,-2.80467132565798,35.0956346738854));
#30630=CARTESIAN_POINT('Ctrl Pts',(4.1226044377536,-2.68291642884286,35.1039272487882));
#30631=CARTESIAN_POINT('Ctrl Pts',(4.15969752499579,-2.62503795634039,35.1078239510336));
#30632=CARTESIAN_POINT('Ctrl Pts',(4.25849930897197,-2.46351634486478,35.1185838220245));
#30633=CARTESIAN_POINT('Ctrl Pts',(4.31762708375117,-2.35835215793882,35.1254637639571));
#30634=CARTESIAN_POINT('Ctrl Pts',(4.37948025635084,-2.23820171788697,35.1331916014403));
#30635=CARTESIAN_POINT('Ctrl Pts',(4.3860744321992,-2.2252517431404,35.1340228158859));
#30636=CARTESIAN_POINT('Ctrl Pts',(4.46182235116031,-2.07484933382165,35.1436568720369));
#30637=CARTESIAN_POINT('Ctrl Pts',(4.52454670835785,-1.93425330871263,35.1524752345383));
#30638=CARTESIAN_POINT('Ctrl Pts',(4.59977867133716,-1.74183804071068,35.1642583112145));
#30639=CARTESIAN_POINT('Ctrl Pts',(4.61818931818931,-1.69242166698918,35.1672596324175));
#30640=CARTESIAN_POINT('Ctrl Pts',(4.64837931057808,-1.60722458043099,35.1723880856175));
#30641=CARTESIAN_POINT('Ctrl Pts',(4.66054863892969,-1.57158756684254,35.1745192133171));
#30642=CARTESIAN_POINT('Ctrl Pts',(4.69027507393914,-1.48115274608639,35.1798950581512));
#30643=CARTESIAN_POINT('Ctrl Pts',(4.70728203525076,-1.42618009876383,35.183133703897));
#30644=CARTESIAN_POINT('Ctrl Pts',(4.77022980523184,-1.20930222265085,35.1958222020602));
#30645=CARTESIAN_POINT('Ctrl Pts',(4.80881298324741,-1.04538147024358,35.2052239607812));
#30646=CARTESIAN_POINT('Ctrl Pts',(4.85335831839818,-0.800382789422243,
35.2191931890541));
#30647=CARTESIAN_POINT('Ctrl Pts',(4.86584119484062,-0.720617014055338,
35.223727776923));
#30648=CARTESIAN_POINT('Ctrl Pts',(4.88595833330758,-0.567477356665587,
35.2324272699616));
#30649=CARTESIAN_POINT('Ctrl Pts',(4.89391635714192,-0.494167893012595,
35.2365890323102));
#30650=CARTESIAN_POINT('Ctrl Pts',(4.90635657566737,-0.349269603322752,
35.2448203684671));
#30651=CARTESIAN_POINT('Ctrl Pts',(4.91092691024947,-0.277706364567444,
35.2488883312892));
#30652=CARTESIAN_POINT('Ctrl Pts',(4.92191132562743,-0.0157719820459993,
35.2637990267744));
#30653=CARTESIAN_POINT('Ctrl Pts',(4.91883053997718,0.174826206695605,35.2746965227519));
#30654=CARTESIAN_POINT('Ctrl Pts',(4.89879635409299,0.444212418833327,35.290158576961));
#30655=CARTESIAN_POINT('Ctrl Pts',(4.89095794756022,0.52350823523645,35.29471621915));
#30656=CARTESIAN_POINT('Ctrl Pts',(4.87788952290732,0.629369143233817,35.3008022574634));
#30657=CARTESIAN_POINT('Ctrl Pts',(4.87436178539507,0.656131779136851,35.3023409740495));
#30658=CARTESIAN_POINT('Ctrl Pts',(4.86465979669225,0.725332430524917,35.3063192485691));
#30659=CARTESIAN_POINT('Ctrl Pts',(4.85815046860718,0.767721403762226,35.3087557534089));
#30660=CARTESIAN_POINT('Ctrl Pts',(4.84419728172664,0.851284921245567,35.3135557108691));
#30661=CARTESIAN_POINT('Ctrl Pts',(4.83678072377878,0.892460420300843,35.3159192205619));
#30662=CARTESIAN_POINT('Ctrl Pts',(4.80816732466374,1.04046696157637,35.3244183385387));
#30663=CARTESIAN_POINT('Ctrl Pts',(4.78394864532835,1.14668232795667,35.3305246482754));
#30664=CARTESIAN_POINT('Ctrl Pts',(4.71531869157069,1.40739926996597,35.3456314857569));
#30665=CARTESIAN_POINT('Ctrl Pts',(4.66682342105925,1.56069270403046,35.3546208389073));
#30666=CARTESIAN_POINT('Ctrl Pts',(4.58293239882621,1.78672319446491,35.3681831994747));
#30667=CARTESIAN_POINT('Ctrl Pts',(4.55310816560508,1.86141209030977,35.3727162804049));
#30668=CARTESIAN_POINT('Ctrl Pts',(4.49438042703801,1.99861594648758,35.3811547706978));
#30669=CARTESIAN_POINT('Ctrl Pts',(4.46596909107252,2.06132022223891,35.3850556024099));
#30670=CARTESIAN_POINT('Ctrl Pts',(4.38678715884847,2.22674820904172,35.3954745487949));
#30671=CARTESIAN_POINT('Ctrl Pts',(4.3337277062924,2.32832832495043,35.4020069803053));
#30672=CARTESIAN_POINT('Ctrl Pts',(4.20695761677324,2.55165032044152,35.4166864261798));
#30673=CARTESIAN_POINT('Ctrl Pts',(4.13141289242162,2.67223486606339,35.4248364362686));
#30674=CARTESIAN_POINT('Ctrl Pts',(4.01967174683556,2.83450607149908,35.4360982966265));
#30675=CARTESIAN_POINT('Ctrl Pts',(3.98784228832422,2.87911437359183,35.4392263456227));
#30676=CARTESIAN_POINT('Ctrl Pts',(3.92899460527035,2.95873949708962,35.4448649364504));
#30677=CARTESIAN_POINT('Ctrl Pts',(3.90223678956224,2.99394156912474,35.4473778195897));
#30678=CARTESIAN_POINT('Ctrl Pts',(3.8532304820134,3.05664005760154,35.4518875807057));
#30679=CARTESIAN_POINT('Ctrl Pts',(3.83115332220221,3.08426617472947,35.4538867358657));
#30680=CARTESIAN_POINT('Ctrl Pts',(3.75985666853106,3.17153597972852,35.4602456957619));
#30681=CARTESIAN_POINT('Ctrl Pts',(3.70952741897562,3.23025837795004,35.4645908826303));
#30682=CARTESIAN_POINT('Ctrl Pts',(3.53329343628597,3.42632886065381,35.4793816893668));
#30683=CARTESIAN_POINT('Ctrl Pts',(3.40098078254064,3.55769891295114,35.4897881856924));
#30684=CARTESIAN_POINT('Ctrl Pts',(3.2311778263141,3.70814211254616,35.5025399427339));
#30685=CARTESIAN_POINT('Ctrl Pts',(3.20048872811925,3.73466195917086,35.5048220391819));
#30686=CARTESIAN_POINT('Ctrl Pts',(3.11397377532801,3.80757385763631,35.5111964149503));
#30687=CARTESIAN_POINT('Ctrl Pts',(3.05744411629576,3.85311389255301,35.5152945406126));
#30688=CARTESIAN_POINT('Ctrl Pts',(2.94934317972048,3.9363222325257,35.523017533691));
#30689=CARTESIAN_POINT('Ctrl Pts',(2.89800568544457,3.9742698503756,35.5266391511902));
#30690=CARTESIAN_POINT('Ctrl Pts',(2.68800168978644,4.12326731880424,35.5412799856154));
#30691=CARTESIAN_POINT('Ctrl Pts',(2.52357997662633,4.22589974555402,35.5523590464138));
#30692=CARTESIAN_POINT('Ctrl Pts',(2.28301200225218,4.35700477835287,35.5680412992763));
#30693=CARTESIAN_POINT('Ctrl Pts',(2.21155366352692,4.39370742774931,35.5726363150185));
#30694=CARTESIAN_POINT('Ctrl Pts',(2.08861779721544,4.45309081895141,35.5804265026641));
#30695=CARTESIAN_POINT('Ctrl Pts',(2.03759150475456,4.47666875156929,35.5836271366221));
#30696=CARTESIAN_POINT('Ctrl Pts',(1.95206899331457,4.5144212635825,35.5889331523417));
#30697=CARTESIAN_POINT('Ctrl Pts',(1.91779607910989,4.52908720742882,35.5910437831288));
#30698=CARTESIAN_POINT('Ctrl Pts',(1.82269681133135,4.56850869247828,35.5968595098942));
#30699=CARTESIAN_POINT('Ctrl Pts',(1.76153622343746,4.59243787452308,35.6005550265257));
#30700=CARTESIAN_POINT('Ctrl Pts',(1.54066140989137,4.67379372397906,35.6137762428182));
#30701=CARTESIAN_POINT('Ctrl Pts',(1.37847871486517,4.72416999752524,35.6232572068654));
#30702=CARTESIAN_POINT('Ctrl Pts',(1.13785854630853,4.78546104250795,35.6371897550111));
#30703=CARTESIAN_POINT('Ctrl Pts',(1.06124681526641,4.80303180326041,35.6416057346478));
#30704=CARTESIAN_POINT('Ctrl Pts',(0.913005491220411,4.83331058426471,35.6501297807318));
#30705=CARTESIAN_POINT('Ctrl Pts',(0.841450119119143,4.84628019884829,35.6542351000095));
#30706=CARTESIAN_POINT('Ctrl Pts',(0.706672533809823,4.86763399012172,35.6619602598687));
#30707=CARTESIAN_POINT('Ctrl Pts',(0.643523430792517,4.87638433808347,35.6655767889284));
#30708=CARTESIAN_POINT('Ctrl Pts',(0.42281232046767,4.90260548144071,35.6782141367267));
#30709=CARTESIAN_POINT('Ctrl Pts',(0.264591900243389,4.91368504302276,35.6872718082509));
#30710=CARTESIAN_POINT('Ctrl Pts',(0.00391130861140477,4.91931075411147,
35.7021969841897));
#30711=CARTESIAN_POINT('Ctrl Pts',(-0.0983369850662696,4.91832934726269,
35.7080507257407));
#30712=CARTESIAN_POINT('Ctrl Pts',(-0.264829880287277,4.91153702295192,
35.7175670470198));
#30713=CARTESIAN_POINT('Ctrl Pts',(-0.329122045356827,4.90764807403482,
35.7212379117332));
#30714=CARTESIAN_POINT('Ctrl Pts',(-0.430363191619516,4.89952565381932,
35.7270063843158));
#30715=CARTESIAN_POINT('Ctrl Pts',(-0.467371827186547,4.89613395752886,
35.7291121706339));
#30716=CARTESIAN_POINT('Ctrl Pts',(-0.56251269438262,4.8863260919902,35.7345190140703));
#30717=CARTESIAN_POINT('Ctrl Pts',(-0.620575357441604,4.8792919113134,35.737813252619));
#30718=CARTESIAN_POINT('Ctrl Pts',(-0.8520809972973,4.8470461346637,35.7509534417743));
#30719=CARTESIAN_POINT('Ctrl Pts',(-1.02424714000991,4.81360745164655,35.7607422030468));
#30720=CARTESIAN_POINT('Ctrl Pts',(-1.27291597077947,4.75136214304163,35.7751218579547));
#30721=CARTESIAN_POINT('Ctrl Pts',(-1.3510714039057,4.72973182974689,35.7796762632042));
#30722=CARTESIAN_POINT('Ctrl Pts',(-1.4993714977581,4.68471234091248,35.7884051144431));
#30723=CARTESIAN_POINT('Ctrl Pts',(-1.56959373461958,4.66165420689913,35.7925763508389));
#30724=CARTESIAN_POINT('Ctrl Pts',(-1.70674774442866,4.61316785025342,35.8008097182712));
#30725=CARTESIAN_POINT('Ctrl Pts',(-1.77369703218023,4.58784308318062,35.8048701489063));
#30726=CARTESIAN_POINT('Ctrl Pts',(-2.00817701243273,4.49324691822329,35.8192500710691));
#30727=CARTESIAN_POINT('Ctrl Pts',(-2.17240482237042,4.41618596522244,35.8296180705753));
#30728=CARTESIAN_POINT('Ctrl Pts',(-2.43382792269626,4.275399467294,35.8466151909248));
#30729=CARTESIAN_POINT('Ctrl Pts',(-2.53368969942039,4.21698658978817,35.8532324416303));
#30730=CARTESIAN_POINT('Ctrl Pts',(-2.66791069323429,4.1319853891978,35.8622780887086));
#30731=CARTESIAN_POINT('Ctrl Pts',(-2.70411538560231,4.10838298641798,35.864733687263));
#30732=CARTESIAN_POINT('Ctrl Pts',(-2.77450515324051,4.06116118919716,35.8695363196967));
#30733=CARTESIAN_POINT('Ctrl Pts',(-2.80871133408824,4.03757968823795,35.8718835670622));
#30734=CARTESIAN_POINT('Ctrl Pts',(-2.95943388126726,3.93083023077026,35.882297553027));
#30735=CARTESIAN_POINT('Ctrl Pts',(-3.07258632622914,3.84303127655233,35.890309712356));
#30736=CARTESIAN_POINT('Ctrl Pts',(-3.30008203783178,3.65003050180804,35.9070226926995));
#30737=CARTESIAN_POINT('Ctrl Pts',(-3.41359665507696,3.54409667055748,35.9157160760218));
#30738=CARTESIAN_POINT('Ctrl Pts',(-3.57230006490842,3.38128177480475,35.9285272479206));
#30739=CARTESIAN_POINT('Ctrl Pts',(-3.62154332756609,3.32848583616918,35.9326035210023));
#30740=CARTESIAN_POINT('Ctrl Pts',(-3.71229839944081,3.2267840166484,35.9403210647821));
#30741=CARTESIAN_POINT('Ctrl Pts',(-3.75405053938842,3.17811247902906,35.9439592773417));
#30742=CARTESIAN_POINT('Ctrl Pts',(-3.86796237286903,3.03994471280065,35.9541421979463));
#30743=CARTESIAN_POINT('Ctrl Pts',(-3.93795322476101,2.94871508723163,35.9607021659529));
#30744=CARTESIAN_POINT('Ctrl Pts',(-4.0806436240454,2.74857283843998,35.9747603210542));
#30745=CARTESIAN_POINT('Ctrl Pts',(-4.15232231793356,2.63903854233169,35.9822575754484));
#30746=CARTESIAN_POINT('Ctrl Pts',(-4.25699061142251,2.46424950146359,35.9939007057588));
#30747=CARTESIAN_POINT('Ctrl Pts',(-4.29303938975728,2.4008972618599,35.9980580617457));
#30748=CARTESIAN_POINT('Ctrl Pts',(-4.3455069459514,2.30372790713162,36.0043329788738));
#30749=CARTESIAN_POINT('Ctrl Pts',(-4.36296781754265,2.27048557921604,36.0064618431766));
#30750=CARTESIAN_POINT('Ctrl Pts',(-4.40384441819539,2.1904508355273,36.0115446006063));
#30751=CARTESIAN_POINT('Ctrl Pts',(-4.42689745977726,2.14347836363896,36.0144940474605));
#30752=CARTESIAN_POINT('Ctrl Pts',(-4.51892298387864,1.9481486768789,36.0266417500765));
#30753=CARTESIAN_POINT('Ctrl Pts',(-4.58122170532503,1.79676282753445,36.0357841157447));
#30754=CARTESIAN_POINT('Ctrl Pts',(-4.66570810398347,1.55831266185887,36.0499654484953));
#30755=CARTESIAN_POINT('Ctrl Pts',(-4.69325394094342,1.47327448889247,36.0549807112711));
#30756=CARTESIAN_POINT('Ctrl Pts',(-4.73461952527767,1.33260607176634,36.0632322216301));
#30757=CARTESIAN_POINT('Ctrl Pts',(-4.74981087387954,1.27740252714152,36.0664592637781));
#30758=CARTESIAN_POINT('Ctrl Pts',(-4.76403458739297,1.22194824465831,36.0696927553338));
#30759=CARTESIAN_POINT('Origin',(0.,0.,-3.23514056400928));
#30760=CARTESIAN_POINT('',(-4.76417305830272,1.22198379731345,38.1652023751175));
#30761=CARTESIAN_POINT('',(-4.76403458711433,1.22194824574464,37.8201594747841));
#30762=CARTESIAN_POINT('',(-4.76403458704967,1.22194824599672,-3.23514056400928));
#30763=CARTESIAN_POINT('',(-4.91815853856044,-0.000126264742759089,36.485140567961));
#30764=CARTESIAN_POINT('Ctrl Pts',(-4.91815853856044,-0.000126264742759089,
36.485140567961));
#30765=CARTESIAN_POINT('Ctrl Pts',(-4.9183727443974,-0.218274538310673,
36.4974939210882));
#30766=CARTESIAN_POINT('Ctrl Pts',(-4.85071591826797,-1.25417721681692,
36.5561627359772));
#30767=CARTESIAN_POINT('Ctrl Pts',(-4.13688039937621,-3.02851950177622,
36.6611470126279));
#30768=CARTESIAN_POINT('Ctrl Pts',(-2.18373858264853,-4.63864156990321,
36.800093397913));
#30769=CARTESIAN_POINT('Ctrl Pts',(0.301699006312604,-5.11807459118877,
36.9390397831982));
#30770=CARTESIAN_POINT('Ctrl Pts',(2.71359615099928,-4.34995468259888,37.0779861684833));
#30771=CARTESIAN_POINT('Ctrl Pts',(4.46404243787587,-2.52151441087003,37.2169325537684));
#30772=CARTESIAN_POINT('Ctrl Pts',(5.12635897532519,-0.0784440404670848,
37.3558789390535));
#30773=CARTESIAN_POINT('Ctrl Pts',(4.53910322825366,2.383747405796,37.4948253243387));
#30774=CARTESIAN_POINT('Ctrl Pts',(2.84542133781098,4.26489005974503,37.6337717096238));
#30775=CARTESIAN_POINT('Ctrl Pts',(0.458155627228689,5.1064472221517,37.7727180949089));
#30776=CARTESIAN_POINT('Ctrl Pts',(-2.04078750909336,4.70328567642987,37.911664480194));
#30777=CARTESIAN_POINT('Ctrl Pts',(-3.92533759866974,3.24421753779699,38.0424925735969));
#30778=CARTESIAN_POINT('Ctrl Pts',(-4.59593587221692,1.87509631612692,38.127005205238));
#30779=CARTESIAN_POINT('Ctrl Pts',(-4.76417305830272,1.22198379731345,38.1652023751175));
#30780=CARTESIAN_POINT('Ctrl Pts',(-4.76403458704968,1.22194824599668,36.4152130395234));
#30781=CARTESIAN_POINT('Ctrl Pts',(-4.79972046865974,1.0828189704184,36.4233465153422));
#30782=CARTESIAN_POINT('Ctrl Pts',(-4.82931125243571,0.942110445198123,
36.4314799911609));
#30783=CARTESIAN_POINT('Ctrl Pts',(-4.85268865924507,0.800372312698471,
36.4396134669797));
#30784=CARTESIAN_POINT('Ctrl Pts',(-4.87606781843622,0.658623555439367,
36.4477475524878));
#30785=CARTESIAN_POINT('Ctrl Pts',(-4.89323261137389,0.515845369784952,
36.4558816379958));
#30786=CARTESIAN_POINT('Ctrl Pts',(-4.90411614098923,0.372596213331416,
36.4640157235039));
#30787=CARTESIAN_POINT('Ctrl Pts',(-4.91353792651271,0.248586551371808,
36.4710573370057));
#30788=CARTESIAN_POINT('Ctrl Pts',(-4.91825318908601,0.124224198834564,
36.4780989505075));
#30789=CARTESIAN_POINT('Ctrl Pts',(-4.91824999838095,-0.000126197307044433,
36.4851405640093));
#30790=CARTESIAN_POINT('Ctrl Pts',(-4.76403458739297,1.22194824465831,36.0696927553338));
#30791=CARTESIAN_POINT('Ctrl Pts',(-4.76915365858994,1.20199041719359,36.070856479102));
#30792=CARTESIAN_POINT('Ctrl Pts',(-4.77414739613201,1.18200011230845,36.0720210311605));
#30793=CARTESIAN_POINT('Ctrl Pts',(-4.79525687143362,1.09518051212781,36.0770746475064));
#30794=CARTESIAN_POINT('Ctrl Pts',(-4.81009585453188,1.02804987461523,36.0809717342797));
#30795=CARTESIAN_POINT('Ctrl Pts',(-4.86834654471026,0.73556130694027,36.0979195148213));
#30796=CARTESIAN_POINT('Ctrl Pts',(-4.89736196884957,0.507633011785284,
36.1110600136259));
#30797=CARTESIAN_POINT('Ctrl Pts',(-4.91561843347707,0.185766226537681,
36.1295031537217));
#30798=CARTESIAN_POINT('Ctrl Pts',(-4.91825037702714,0.092882873750499,
36.1348100284067));
#30799=CARTESIAN_POINT('Ctrl Pts',(-4.91824985764764,-0.0350876821920873,
36.1420868305489));
#30800=CARTESIAN_POINT('Ctrl Pts',(-4.91787465981299,-0.0701546963813987,
36.1440771817146));
#30801=CARTESIAN_POINT('Ctrl Pts',(-4.91616350889335,-0.150123722229815,
36.1486062881711));
#30802=CARTESIAN_POINT('Ctrl Pts',(-4.91458736888693,-0.195017528460413,
36.1511421422222));
#30803=CARTESIAN_POINT('Ctrl Pts',(-4.90965832228768,-0.295955705186828,
36.1568357064839));
#30804=CARTESIAN_POINT('Ctrl Pts',(-4.90596034311486,-0.351977004863166,
36.1599901367399));
#30805=CARTESIAN_POINT('Ctrl Pts',(-4.8887269443645,-0.559040894279331,
36.1716502725919));
#30806=CARTESIAN_POINT('Ctrl Pts',(-4.86916758142504,-0.709496338106361,
36.1801267343971));
#30807=CARTESIAN_POINT('Ctrl Pts',(-4.82405283840344,-0.963891740085001,
36.1946230874154));
#30808=CARTESIAN_POINT('Ctrl Pts',(-4.80200176752851,-1.06834062535704,
36.2006223805234));
#30809=CARTESIAN_POINT('Ctrl Pts',(-4.76027223083158,-1.23841404828793,
36.2105051232522));
#30810=CARTESIAN_POINT('Ctrl Pts',(-4.74259017863045,-1.30449197949791,
36.2143734370645));
#30811=CARTESIAN_POINT('Ctrl Pts',(-4.70043830961648,-1.44980573098613,
36.2229523507716));
#30812=CARTESIAN_POINT('Ctrl Pts',(-4.67533109172692,-1.52883481968609,
36.2276662087741));
#30813=CARTESIAN_POINT('Ctrl Pts',(-4.57287602866743,-1.8251503429335,36.2455380171558));
#30814=CARTESIAN_POINT('Ctrl Pts',(-4.48227722362476,-2.03753736275619,
36.2587696446889));
#30815=CARTESIAN_POINT('Ctrl Pts',(-4.35116810217376,-2.29341583938602,
36.2751775824367));
#30816=CARTESIAN_POINT('Ctrl Pts',(-4.32434655824455,-2.34359702566997,
36.2784180459329));
#30817=CARTESIAN_POINT('Ctrl Pts',(-4.27857355765126,-2.42577262890232,
36.283757947967));
#30818=CARTESIAN_POINT('Ctrl Pts',(-4.26011942324112,-2.45803723976721,
36.2858628635063));
#30819=CARTESIAN_POINT('Ctrl Pts',(-4.20858540441802,-2.5458137013304,36.291614191006));
#30820=CARTESIAN_POINT('Ctrl Pts',(-4.17477442051568,-2.60088777153404,
36.2952513703655));
#30821=CARTESIAN_POINT('Ctrl Pts',(-4.08435117684644,-2.7418680341201,36.3046605879271));
#30822=CARTESIAN_POINT('Ctrl Pts',(-4.02611142905145,-2.82669273457415,
36.3104199277061));
#30823=CARTESIAN_POINT('Ctrl Pts',(-3.87217013280134,-3.03648457217969,
36.3249975394785));
#30824=CARTESIAN_POINT('Ctrl Pts',(-3.77305297749951,-3.15879889369088,
36.3338141331148));
#30825=CARTESIAN_POINT('Ctrl Pts',(-3.6257598569724,-3.32372026083363,36.3462787700566));
#30826=CARTESIAN_POINT('Ctrl Pts',(-3.58235384825361,-3.37045867916036,
36.3498810564949));
#30827=CARTESIAN_POINT('Ctrl Pts',(-3.48757739788449,-3.46861167924278,
36.3576054318407));
#30828=CARTESIAN_POINT('Ctrl Pts',(-3.43595150810933,-3.5197585364517,36.3617291118343));
#30829=CARTESIAN_POINT('Ctrl Pts',(-3.27792643239327,-3.66952629230834,
36.3741154567728));
#30830=CARTESIAN_POINT('Ctrl Pts',(-3.16827919646488,-3.76460236233875,
36.3824044328307));
#30831=CARTESIAN_POINT('Ctrl Pts',(-2.96279456250041,-3.92743552580013,
36.397411293512));
#30832=CARTESIAN_POINT('Ctrl Pts',(-2.86842759957285,-3.99687687535657,
36.4041190283989));
#30833=CARTESIAN_POINT('Ctrl Pts',(-2.72426787117915,-4.09522166724581,
36.4140786490599));
#30834=CARTESIAN_POINT('Ctrl Pts',(-2.67630152045202,-4.12672827072678,
36.4173471574357));
#30835=CARTESIAN_POINT('Ctrl Pts',(-2.59639012578395,-4.17723851743229,
36.422714119074));
#30836=CARTESIAN_POINT('Ctrl Pts',(-2.56476189492292,-4.19673203539651,
36.4248182203869));
#30837=CARTESIAN_POINT('Ctrl Pts',(-2.47809149356706,-4.24880409266185,
36.430531595401));
#30838=CARTESIAN_POINT('Ctrl Pts',(-2.42262977658445,-4.28067036623187,
36.434131900227));
#30839=CARTESIAN_POINT('Ctrl Pts',(-2.27809865825806,-4.36000380224147,
36.4433948881115));
#30840=CARTESIAN_POINT('Ctrl Pts',(-2.18816146882649,-4.40582753155394,
36.4490453437659));
#30841=CARTESIAN_POINT('Ctrl Pts',(-1.95126547375955,-4.51748374854374,
36.4637167856342));
#30842=CARTESIAN_POINT('Ctrl Pts',(-1.80237279492715,-4.57892430172765,
36.4727356618099));
#30843=CARTESIAN_POINT('Ctrl Pts',(-1.59075766756926,-4.65432351409807,
36.4853995559263));
#30844=CARTESIAN_POINT('Ctrl Pts',(-1.53036915096628,-4.6745275143435,36.4889959686534));
#30845=CARTESIAN_POINT('Ctrl Pts',(-1.4001071016717,-4.71531406958335,36.4967237688206));
#30846=CARTESIAN_POINT('Ctrl Pts',(-1.33013419623863,-4.73552843126685,
36.5008568208325));
#30847=CARTESIAN_POINT('Ctrl Pts',(-1.18354059721869,-4.77437205824853,
36.5094848613463));
#30848=CARTESIAN_POINT('Ctrl Pts',(-1.10686851233857,-4.79272770136382,
36.5139803912809));
#30849=CARTESIAN_POINT('Ctrl Pts',(-0.862099947135587,-4.84513938545707,
36.5282822763344));
#30850=CARTESIAN_POINT('Ctrl Pts',(-0.692648075571482,-4.87225106859554,
36.5381136708041));
#30851=CARTESIAN_POINT('Ctrl Pts',(-0.45771661135187,-4.89733341688776,
36.5516073274126));
#30852=CARTESIAN_POINT('Ctrl Pts',(-0.393175739072369,-4.9029370869517,
36.5552996437567));
#30853=CARTESIAN_POINT('Ctrl Pts',(-0.291453084146704,-4.9097474430385,
36.5610900653705));
#30854=CARTESIAN_POINT('Ctrl Pts',(-0.254336584095457,-4.91181003327085,
36.5631964839663));
#30855=CARTESIAN_POINT('Ctrl Pts',(-0.159061500614999,-4.91602168059029,
36.5685878054371));
#30856=CARTESIAN_POINT('Ctrl Pts',(-0.100881673223977,-4.91755963187683,
36.5718660010508));
#30857=CARTESIAN_POINT('Ctrl Pts',(0.108699118375107,-4.91937875025216,
36.5836488592819));
#30858=CARTESIAN_POINT('Ctrl Pts',(0.260066795118579,-4.91370212603069,
36.592112023372));
#30859=CARTESIAN_POINT('Ctrl Pts',(0.533586397255727,-4.89076870533044,
36.607497826894));
#30860=CARTESIAN_POINT('Ctrl Pts',(0.655810477627973,-4.8758840281008,36.6144066117279));
#30861=CARTESIAN_POINT('Ctrl Pts',(0.8397378360262,-4.84644363229078,36.6249090992425));
#30862=CARTESIAN_POINT('Ctrl Pts',(0.901930784488347,-4.83525555333189,
36.6284786899739));
#30863=CARTESIAN_POINT('Ctrl Pts',(1.03612870172869,-4.80843500302867,36.6362278924348));
#30864=CARTESIAN_POINT('Ctrl Pts',(1.10803284803315,-4.79237653984517,36.6404095328151));
#30865=CARTESIAN_POINT('Ctrl Pts',(1.25778653838397,-4.75538125074671,36.6491875557834));
#30866=CARTESIAN_POINT('Ctrl Pts',(1.3355370758514,-4.73413332663268,36.6537846962049));
#30867=CARTESIAN_POINT('Ctrl Pts',(1.61137584802014,-4.65141481377237,36.6702416063608));
#30868=CARTESIAN_POINT('Ctrl Pts',(1.80605539531741,-4.5793401484156,36.6821406405479));
#30869=CARTESIAN_POINT('Ctrl Pts',(2.03507818297181,-4.47766738938773,36.6964075302048));
#30870=CARTESIAN_POINT('Ctrl Pts',(2.07432106109065,-4.45962337584138,36.6988616261605));
#30871=CARTESIAN_POINT('Ctrl Pts',(2.15085572429808,-4.42320365267304,36.7036640114162));
#30872=CARTESIAN_POINT('Ctrl Pts',(2.18816231028214,-4.40486738176892,36.7060125019989));
#30873=CARTESIAN_POINT('Ctrl Pts',(2.24816515866717,-4.37442542191196,36.7098062108382));
#30874=CARTESIAN_POINT('Ctrl Pts',(2.27100659201765,-4.36261084914746,36.7112542875156));
#30875=CARTESIAN_POINT('Ctrl Pts',(2.42761967201566,-4.2800405177099,36.7212141084749));
#30876=CARTESIAN_POINT('Ctrl Pts',(2.55815713848632,-4.20332211675965,36.7296748834678));
#30877=CARTESIAN_POINT('Ctrl Pts',(2.79535887450648,-4.04876737336505,36.7455413947904));
#30878=CARTESIAN_POINT('Ctrl Pts',(2.90283066170729,-3.97242016958557,36.7529353450391));
#30879=CARTESIAN_POINT('Ctrl Pts',(3.05710596234772,-3.85321667938635,36.7639280127181));
#30880=CARTESIAN_POINT('Ctrl Pts',(3.1063567228369,-3.81362340112572,36.7674976596078));
#30881=CARTESIAN_POINT('Ctrl Pts',(3.21134346892449,-3.72583986514702,36.7752468058592));
#30882=CARTESIAN_POINT('Ctrl Pts',(3.26678710764764,-3.67732394500727,36.7794283330527));
#30883=CARTESIAN_POINT('Ctrl Pts',(3.38055788639135,-3.57316463836555,36.7882060072511));
#30884=CARTESIAN_POINT('Ctrl Pts',(3.43864926588164,-3.51729558064057,36.7928029115859));
#30885=CARTESIAN_POINT('Ctrl Pts',(3.63786059521919,-3.31605090794667,36.808985175974));
#30886=CARTESIAN_POINT('Ctrl Pts',(3.77134836138037,-3.16340879050152,36.8206074351496));
#30887=CARTESIAN_POINT('Ctrl Pts',(3.92265364090943,-2.96715630393549,36.834722765214));
#30888=CARTESIAN_POINT('Ctrl Pts',(3.94977029072956,-2.93096278269341,36.8372934393489));
#30889=CARTESIAN_POINT('Ctrl Pts',(3.99999551027771,-2.86196238409177,36.8421307986737));
#30890=CARTESIAN_POINT('Ctrl Pts',(4.02320910019249,-2.82923688308017,36.8443985764278));
#30891=CARTESIAN_POINT('Ctrl Pts',(4.12006346219044,-2.68909298197594,36.8540080299212));
#30892=CARTESIAN_POINT('Ctrl Pts',(4.18982321592747,-2.57905529323885,36.8613035060759));
#30893=CARTESIAN_POINT('Ctrl Pts',(4.34510123776315,-2.31116089382878,36.8786506666839));
#30894=CARTESIAN_POINT('Ctrl Pts',(4.42650742263402,-2.15113932963113,36.8886929152544));
#30895=CARTESIAN_POINT('Ctrl Pts',(4.52473862876919,-1.92872647022129,36.902398987217));
#30896=CARTESIAN_POINT('Ctrl Pts',(4.54935310344817,-1.86992825671265,36.9059989145167));
#30897=CARTESIAN_POINT('Ctrl Pts',(4.59959277319203,-1.74304869485935,36.9137246176184));
#30898=CARTESIAN_POINT('Ctrl Pts',(4.62486442537564,-1.67484366784924,36.9178520137867));
#30899=CARTESIAN_POINT('Ctrl Pts',(4.6962248560521,-1.46830217097573,36.930284139322));
#30900=CARTESIAN_POINT('Ctrl Pts',(4.73768411650814,-1.32845303780736,36.9386155180457));
#30901=CARTESIAN_POINT('Ctrl Pts',(4.79837909957649,-1.08439547331938,36.9530107281173));
#30902=CARTESIAN_POINT('Ctrl Pts',(4.82057543841378,-0.981024011397351,
36.9590637111313));
#30903=CARTESIAN_POINT('Ctrl Pts',(4.85088758435772,-0.813760173383621,
36.9687716407984));
#30904=CARTESIAN_POINT('Ctrl Pts',(4.86111003255971,-0.750283528148921,
36.972435899526));
#30905=CARTESIAN_POINT('Ctrl Pts',(4.87527298311822,-0.649828618438256,
36.9781976231457));
#30906=CARTESIAN_POINT('Ctrl Pts',(4.88004356932441,-0.612975285299537,
36.9803032249921));
#30907=CARTESIAN_POINT('Ctrl Pts',(4.89125660588522,-0.517902075131387,
36.9857149504015));
#30908=CARTESIAN_POINT('Ctrl Pts',(4.8970775079715,-0.45961478095763,36.9890142204667));
#30909=CARTESIAN_POINT('Ctrl Pts',(4.90888722511114,-0.315337114742292,
36.9971521125751));
#30910=CARTESIAN_POINT('Ctrl Pts',(4.91365934784131,-0.229266796234206,
37.0019818681607));
#30911=CARTESIAN_POINT('Ctrl Pts',(4.92137141890658,0.0356514832284077,
37.0168303411873));
#30912=CARTESIAN_POINT('Ctrl Pts',(4.91682088426007,0.214567202374961,37.0268388529457));
#30913=CARTESIAN_POINT('Ctrl Pts',(4.89680124701929,0.464409699242177,37.0409631330739));
#30914=CARTESIAN_POINT('Ctrl Pts',(4.88949939728122,0.535849146955819,37.0450181385255));
#30915=CARTESIAN_POINT('Ctrl Pts',(4.87155096025943,0.680140738863191,37.0532514739268));
#30916=CARTESIAN_POINT('Ctrl Pts',(4.86082744378178,0.752965186673622,37.0574293176773));
#30917=CARTESIAN_POINT('Ctrl Pts',(4.83496994747732,0.904832194723154,37.0661956407366));
#30918=CARTESIAN_POINT('Ctrl Pts',(4.81952216143642,0.98379959792492,37.0707848609837));
#30919=CARTESIAN_POINT('Ctrl Pts',(4.76503426862988,1.23010096849234,37.0852003531169));
#30920=CARTESIAN_POINT('Ctrl Pts',(4.7191599004821,1.39579000797142,37.0950502339182));
#30921=CARTESIAN_POINT('Ctrl Pts',(4.64518331278746,1.61717379493152,37.1083770337312));
#30922=CARTESIAN_POINT('Ctrl Pts',(4.6245601732874,1.67523802130459,37.1118877803724));
#30923=CARTESIAN_POINT('Ctrl Pts',(4.58977248063143,1.76763953902369,37.1174942274581));
#30924=CARTESIAN_POINT('Ctrl Pts',(4.57630067287657,1.80223005114025,37.1195971051009));
#30925=CARTESIAN_POINT('Ctrl Pts',(4.5396929749308,1.89316680174464,37.1251375950794));
#30926=CARTESIAN_POINT('Ctrl Pts',(4.51589974070905,1.94924152212843,37.12856744341));
#30927=CARTESIAN_POINT('Ctrl Pts',(4.45343689537089,2.08916402458212,37.1371792107406));
#30928=CARTESIAN_POINT('Ctrl Pts',(4.41343635217545,2.17239182678577,37.1423509056104));
#30929=CARTESIAN_POINT('Ctrl Pts',(4.30838920675485,2.37606652267735,37.1551892608679));
#30930=CARTESIAN_POINT('Ctrl Pts',(4.24061337211479,2.49501653053431,37.1628518148848));
#30931=CARTESIAN_POINT('Ctrl Pts',(4.12484860677061,2.67981411048286,37.1751170017326));
#30932=CARTESIAN_POINT('Ctrl Pts',(4.08003299963365,2.74756441308388,37.1796950442693));
#30933=CARTESIAN_POINT('Ctrl Pts',(3.99426859348585,2.87049072220417,37.1881691233165));
#30934=CARTESIAN_POINT('Ctrl Pts',(3.9538016592187,2.92597861923693,37.1920602613161));
#30935=CARTESIAN_POINT('Ctrl Pts',(3.84450798527856,3.06943200279022,37.2023044399441));
#30936=CARTESIAN_POINT('Ctrl Pts',(3.77382427321572,3.15593160804204,37.2086706925013));
#30937=CARTESIAN_POINT('Ctrl Pts',(3.5724346226182,3.38593328248438,37.2261434429111));
#30938=CARTESIAN_POINT('Ctrl Pts',(3.4360836985779,3.52422507944231,37.2372732668762));
#30939=CARTESIAN_POINT('Ctrl Pts',(3.25659611627805,3.68592258255789,37.251040096925));
#30940=CARTESIAN_POINT('Ctrl Pts',(3.22081216307909,3.71723185069398,37.2537439762873));
#30941=CARTESIAN_POINT('Ctrl Pts',(3.15486294948704,3.77326694559638,37.2586509126666));
#30942=CARTESIAN_POINT('Ctrl Pts',(3.12484712788844,3.79816194076146,37.2608560090299));
#30943=CARTESIAN_POINT('Ctrl Pts',(3.01979070371403,3.88320688457817,37.2684835395084));
#30944=CARTESIAN_POINT('Ctrl Pts',(2.94328382915175,3.94151142288682,37.2738820112885));
#30945=CARTESIAN_POINT('Ctrl Pts',(2.68280056517236,4.12820513036423,37.2918494349101));
#30946=CARTESIAN_POINT('Ctrl Pts',(2.49176121249271,4.24624790575298,37.3043788073436));
#30947=CARTESIAN_POINT('Ctrl Pts',(2.23237591464222,4.38297037470432,37.3209148486011));
#30948=CARTESIAN_POINT('Ctrl Pts',(2.17074865777022,4.41381712957403,37.3248093750886));
#30949=CARTESIAN_POINT('Ctrl Pts',(2.03859081144828,4.47652961057704,37.333097849338));
#30950=CARTESIAN_POINT('Ctrl Pts',(1.96791507519602,4.50804613002256,37.3374932572073));
#30951=CARTESIAN_POINT('Ctrl Pts',(1.79802663513586,4.57904793868868,37.3479795050177));
#30952=CARTESIAN_POINT('Ctrl Pts',(1.69821397042713,4.61699564189424,37.354077925755));
#30953=CARTESIAN_POINT('Ctrl Pts',(1.43473985138644,4.70746499598242,37.3700171980796));
#30954=CARTESIAN_POINT('Ctrl Pts',(1.26941980741697,4.75471126598224,37.3798657421152));
#30955=CARTESIAN_POINT('Ctrl Pts',(1.06121854151851,4.802577057846,37.3920251590479));
#30956=CARTESIAN_POINT('Ctrl Pts',(1.02035277231022,4.81142509740532,37.3944000812988));
#30957=CARTESIAN_POINT('Ctrl Pts',(0.94697174834649,4.82633620394941,37.3986416046695));
#30958=CARTESIAN_POINT('Ctrl Pts',(0.914498867274258,4.83259438552585,37.4005106020057));
#30959=CARTESIAN_POINT('Ctrl Pts',(0.878210596228608,4.83920900315252,37.4025917516664));
#30960=CARTESIAN_POINT('Ctrl Pts',(0.874455248824459,4.83988901167726,37.4028070338407));
#30961=CARTESIAN_POINT('Ctrl Pts',(0.869586956238884,4.84076469836626,37.4030860050825));
#30962=CARTESIAN_POINT('Ctrl Pts',(0.868474731580764,4.8409643646712,37.4031497320734));
#30963=CARTESIAN_POINT('Ctrl Pts',(0.865544675632951,4.84148932533259,37.4033175951875));
#30964=CARTESIAN_POINT('Ctrl Pts',(0.863726729452476,4.84181397924985,37.4034217252602));
#30965=CARTESIAN_POINT('Ctrl Pts',(0.858922939870501,4.84266906183712,37.403696828573));
#30966=CARTESIAN_POINT('Ctrl Pts',(0.85593678711114,4.84319775309633,37.4038677856434));
#30967=CARTESIAN_POINT('Ctrl Pts',(0.848022984751394,4.84459132533947,37.4043207102209));
#30968=CARTESIAN_POINT('Ctrl Pts',(0.843094498914097,4.8454514504014,37.4046026345484));
#30969=CARTESIAN_POINT('Ctrl Pts',(0.830025694823135,4.84771169041316,37.4053498396787));
#30970=CARTESIAN_POINT('Ctrl Pts',(0.821883141434145,4.84909882241837,37.4058150074393));
#30971=CARTESIAN_POINT('Ctrl Pts',(0.750782145772908,4.86102706320264,37.4098737126302));
#30972=CARTESIAN_POINT('Ctrl Pts',(0.687627111697836,4.87036210111441,37.4134573467778));
#30973=CARTESIAN_POINT('Ctrl Pts',(0.410350552395102,4.90584579308773,37.4291335294651));
#30974=CARTESIAN_POINT('Ctrl Pts',(0.194825184235147,4.91912114573091,37.4411798229461));
#30975=CARTESIAN_POINT('Ctrl Pts',(-0.0863308533219903,4.91792789965569,
37.4570199485428));
#30976=CARTESIAN_POINT('Ctrl Pts',(-0.151775949126505,4.91634333481699,
37.4607149545633));
#30977=CARTESIAN_POINT('Ctrl Pts',(-0.28141185302162,4.91061356473325,37.4680574544334));
#30978=CARTESIAN_POINT('Ctrl Pts',(-0.345591927526374,4.90651447731638,
37.4717039275781));
#30979=CARTESIAN_POINT('Ctrl Pts',(-0.481291363410916,4.89517178017584,
37.4794431028436));
#30980=CARTESIAN_POINT('Ctrl Pts',(-0.552769702195023,4.88761635646434,
37.4835369425077));
#30981=CARTESIAN_POINT('Ctrl Pts',(-0.750362476975425,4.86234033424924,
37.4949063055543));
#30982=CARTESIAN_POINT('Ctrl Pts',(-0.875992938351217,4.84128427121603,
37.5021956352467));
#30983=CARTESIAN_POINT('Ctrl Pts',(-1.02269996240819,4.81079769069408,37.5107726807931));
#30984=CARTESIAN_POINT('Ctrl Pts',(-1.0447046516616,4.80606718908558,37.5120608451116));
#30985=CARTESIAN_POINT('Ctrl Pts',(-1.16125003399877,4.78017438267656,37.5188919378874));
#30986=CARTESIAN_POINT('Ctrl Pts',(-1.25518340029912,4.75637296168653,37.5244277682988));
#30987=CARTESIAN_POINT('Ctrl Pts',(-1.38256588247471,4.72005935126867,37.5319613306906));
#30988=CARTESIAN_POINT('Ctrl Pts',(-1.4166720689071,4.70993513645557,37.5339809810342));
#30989=CARTESIAN_POINT('Ctrl Pts',(-1.4824835311819,4.68961986585549,37.5378817238552));
#30990=CARTESIAN_POINT('Ctrl Pts',(-1.51420101865333,4.67947509977371,37.5397634152908));
#30991=CARTESIAN_POINT('Ctrl Pts',(-1.55376046307042,4.66637777806139,37.5421141832611));
#30992=CARTESIAN_POINT('Ctrl Pts',(-1.56170098350097,4.66372631944484,37.5425862325198));
#30993=CARTESIAN_POINT('Ctrl Pts',(-1.58063143798559,4.65735138910722,37.5437121253483));
#30994=CARTESIAN_POINT('Ctrl Pts',(-1.59161504915292,4.65360927029664,37.5443657908606));
#30995=CARTESIAN_POINT('Ctrl Pts',(-1.62331845714446,4.64268254069482,37.5462538979492));
#30996=CARTESIAN_POINT('Ctrl Pts',(-1.64400361325797,4.63539816108357,37.5474874786266));
#30997=CARTESIAN_POINT('Ctrl Pts',(-1.7485712537359,4.59778616217263,37.5537337284135));
#30998=CARTESIAN_POINT('Ctrl Pts',(-1.83166676742684,4.56531883323016,37.5587311911084));
#30999=CARTESIAN_POINT('Ctrl Pts',(-2.07849843915366,4.4610514586551,37.5737426081891));
#31000=CARTESIAN_POINT('Ctrl Pts',(-2.23924689646878,4.38256867160318,37.5837484506122));
#31001=CARTESIAN_POINT('Ctrl Pts',(-2.4314788493592,4.27537173817518,37.5961554127492));
#31002=CARTESIAN_POINT('Ctrl Pts',(-2.46733771663527,4.25477819125951,37.5984892666716));
#31003=CARTESIAN_POINT('Ctrl Pts',(-2.56055473744722,4.19966942606904,37.6046101837079));
#31004=CARTESIAN_POINT('Ctrl Pts',(-2.61747508770703,4.16443127988252,37.6084022023059));
#31005=CARTESIAN_POINT('Ctrl Pts',(-2.73070012924449,4.0910974825056,37.6160624784095));
#31006=CARTESIAN_POINT('Ctrl Pts',(-2.78696992643701,4.05297425481835,37.6199301963578));
#31007=CARTESIAN_POINT('Ctrl Pts',(-2.99993253720415,3.90215781347006,37.6348112009915));
#31008=CARTESIAN_POINT('Ctrl Pts',(-3.15073130341971,3.78144444881562,37.6458733125078));
#31009=CARTESIAN_POINT('Ctrl Pts',(-3.34868432918662,3.60290306530415,37.6611123192323));
#31010=CARTESIAN_POINT('Ctrl Pts',(-3.40221167507765,3.55240103849283,37.6653114850938));
#31011=CARTESIAN_POINT('Ctrl Pts',(-3.48185718223459,3.47380505642974,37.6716735291493));
#31012=CARTESIAN_POINT('Ctrl Pts',(-3.50881304296983,3.4465754161021,37.6738473756669));
#31013=CARTESIAN_POINT('Ctrl Pts',(-3.55954048976114,3.3941207449958,37.6779768906759));
#31014=CARTESIAN_POINT('Ctrl Pts',(-3.58336884734312,3.36895412013561,37.6799337687668));
#31015=CARTESIAN_POINT('Ctrl Pts',(-3.64081556853383,3.30698195472023,37.6846972754829));
#31016=CARTESIAN_POINT('Ctrl Pts',(-3.67414430623344,3.26991304636743,37.6875001847029));
#31017=CARTESIAN_POINT('Ctrl Pts',(-3.7844066043997,3.14346246168126,37.6969213208271));
#31018=CARTESIAN_POINT('Ctrl Pts',(-3.85868775066657,3.05182218593411,37.7035196519911));
#31019=CARTESIAN_POINT('Ctrl Pts',(-4.00908140001213,2.85200230180349,37.7175338517272));
#31020=CARTESIAN_POINT('Ctrl Pts',(-4.0842698593523,2.74324441503253,37.7249469077476));
#31021=CARTESIAN_POINT('Ctrl Pts',(-4.19132552979462,2.5742155938858,37.736223374973));
#31022=CARTESIAN_POINT('Ctrl Pts',(-4.22647239041994,2.51609352374469,37.7400589774292));
#31023=CARTESIAN_POINT('Ctrl Pts',(-4.29218162557632,2.40216679832502,37.7475052072134));
#31024=CARTESIAN_POINT('Ctrl Pts',(-4.32288718079736,2.34646004520824,37.7511139419817));
#31025=CARTESIAN_POINT('Ctrl Pts',(-4.38738524844168,2.22388067773893,37.7589901106813));
#31026=CARTESIAN_POINT('Ctrl Pts',(-4.4207476225241,2.15679968694377,37.7632596135832));
#31027=CARTESIAN_POINT('Ctrl Pts',(-4.51409155944719,1.95784171071394,37.775809157908));
#31028=CARTESIAN_POINT('Ctrl Pts',(-4.56979450790952,1.82404621302096,37.7841072297769));
#31029=CARTESIAN_POINT('Ctrl Pts',(-4.63625768489655,1.6421567416116,37.7951858567299));
#31030=CARTESIAN_POINT('Ctrl Pts',(-4.65232188913736,1.59607805567092,37.7979753020625));
#31031=CARTESIAN_POINT('Ctrl Pts',(-4.68623118588717,1.49394769216465,37.8041175372925));
#31032=CARTESIAN_POINT('Ctrl Pts',(-4.70376192678936,1.4377991129602,37.8074679208683));
#31033=CARTESIAN_POINT('Ctrl Pts',(-4.73026274992449,1.34724174591711,37.8128246000106));
#31034=CARTESIAN_POINT('Ctrl Pts',(-4.73987403156545,1.31302711503208,37.814837534469));
#31035=CARTESIAN_POINT('Ctrl Pts',(-4.75420028048348,1.25981963272418,37.817951762854));
#31036=CARTESIAN_POINT('Ctrl Pts',(-4.75917397327971,1.24089842019217,37.8190561662389));
#31037=CARTESIAN_POINT('Ctrl Pts',(-4.76403458711433,1.22194824574464,37.8201594747841));
#31038=CARTESIAN_POINT('Origin',(0.,0.,-3.23514056400928));
#31039=CARTESIAN_POINT('',(-4.76403458699542,1.22194824620825,39.9154303604093));
#31040=CARTESIAN_POINT('',(-4.76374161084644,1.22187275725133,39.5699226582762));
#31041=CARTESIAN_POINT('',(-4.76403458704967,1.22194824599672,-3.23514056400928));
#31042=CARTESIAN_POINT('',(-4.91801823864715,0.000109808377098883,38.2351405640093));
#31043=CARTESIAN_POINT('Ctrl Pts',(-4.76403458699542,1.22194824620825,39.9154303604093));
#31044=CARTESIAN_POINT('Ctrl Pts',(-4.76226888768041,1.22883221419384,39.9150262275596));
#31045=CARTESIAN_POINT('Ctrl Pts',(-4.76048825187975,1.23571241595701,39.9146219985247));
#31046=CARTESIAN_POINT('Ctrl Pts',(-4.72218457861485,1.38240246304848,39.9059967734601));
#31047=CARTESIAN_POINT('Ctrl Pts',(-4.67953286590494,1.52053774692604,39.897739744708));
#31048=CARTESIAN_POINT('Ctrl Pts',(-4.59002992174783,1.77073549763694,39.8825303168297));
#31049=CARTESIAN_POINT('Ctrl Pts',(-4.54499144113064,1.88333001439706,39.8755876860244));
#31050=CARTESIAN_POINT('Ctrl Pts',(-4.4735792175259,2.04433021541214,39.8655386112798));
#31051=CARTESIAN_POINT('Ctrl Pts',(-4.4504807492959,2.09413902234831,39.8624124595704));
#31052=CARTESIAN_POINT('Ctrl Pts',(-4.41049122053387,2.17671964077631,39.8572044089465));
#31053=CARTESIAN_POINT('Ctrl Pts',(-4.39405710892769,2.20970662269982,39.8551176305458));
#31054=CARTESIAN_POINT('Ctrl Pts',(-4.34746112244599,2.30065952462245,39.8493437879833));
#31055=CARTESIAN_POINT('Ctrl Pts',(-4.31651246047074,2.35821389944226,39.8456663074602));
#31056=CARTESIAN_POINT('Ctrl Pts',(-4.23263617040839,2.50700962124998,39.8360713127913));
#31057=CARTESIAN_POINT('Ctrl Pts',(-4.17790430488023,2.59719502856669,39.8301671141549));
#31058=CARTESIAN_POINT('Ctrl Pts',(-4.03730539533373,2.81290933102471,39.8157414122895));
#31059=CARTESIAN_POINT('Ctrl Pts',(-3.94843619728096,2.93634884622942,39.8072212314393));
#31060=CARTESIAN_POINT('Ctrl Pts',(-3.81458497318871,3.10518091172412,39.7950767132423));
#31061=CARTESIAN_POINT('Ctrl Pts',(-3.77421837457664,3.15412152027172,39.7914941862384));
#31062=CARTESIAN_POINT('Ctrl Pts',(-3.68633375761085,3.25656954447343,39.7838533751558));
#31063=CARTESIAN_POINT('Ctrl Pts',(-3.6385718268744,3.30984843640951,39.7797937123147));
#31064=CARTESIAN_POINT('Ctrl Pts',(-3.47989020820409,3.47927219468329,39.7665897396737));
#31065=CARTESIAN_POINT('Ctrl Pts',(-3.36444212654279,3.59103033630064,39.7574101680859));
#31066=CARTESIAN_POINT('Ctrl Pts',(-3.14084163402903,3.78721992620003,39.7403818984161));
#31067=CARTESIAN_POINT('Ctrl Pts',(-3.03422213400287,3.87316635127496,39.7325448809477));
#31068=CARTESIAN_POINT('Ctrl Pts',(-2.89067646817213,3.97930978356815,39.7223833712935));
#31069=CARTESIAN_POINT('Ctrl Pts',(-2.8568837251367,4.00363987308693,39.7200181516101));
#31070=CARTESIAN_POINT('Ctrl Pts',(-2.78829291408903,4.05171320388529,39.7152733676541));
#31071=CARTESIAN_POINT('Ctrl Pts',(-2.75349056108777,4.07544439865203,39.7128941178801));
#31072=CARTESIAN_POINT('Ctrl Pts',(-2.67583738742511,4.12694611427883,39.7076413839367));
#31073=CARTESIAN_POINT('Ctrl Pts',(-2.63285023185272,4.15450233792234,39.7047704438202));
#31074=CARTESIAN_POINT('Ctrl Pts',(-2.48728661874389,4.24464675796873,39.6951564440135));
#31075=CARTESIAN_POINT('Ctrl Pts',(-2.38284728595317,4.30414449687835,39.6884336974947));
#31076=CARTESIAN_POINT('Ctrl Pts',(-2.22069780329699,4.3888066168109,39.6781827033342));
#31077=CARTESIAN_POINT('Ctrl Pts',(-2.16451112073421,4.41678772543179,39.6746636013246));
#31078=CARTESIAN_POINT('Ctrl Pts',(-2.02207063641701,4.48435251633549,39.6658103974578));
#31079=CARTESIAN_POINT('Ctrl Pts',(-1.93517859377164,4.52252923160447,39.6604709322254));
#31080=CARTESIAN_POINT('Ctrl Pts',(-1.78486454346354,4.58344531307038,39.651312632398));
#31081=CARTESIAN_POINT('Ctrl Pts',(-1.72197986770229,4.60743937323632,39.6475041255071));
#31082=CARTESIAN_POINT('Ctrl Pts',(-1.57623715913091,4.65964783215472,39.6387218457337));
#31083=CARTESIAN_POINT('Ctrl Pts',(-1.49307895660277,4.68695599071738,39.6337430714126));
#31084=CARTESIAN_POINT('Ctrl Pts',(-1.30191896994236,4.74412662427354,39.6223622313465));
#31085=CARTESIAN_POINT('Ctrl Pts',(-1.19353615377101,4.77254665449531,39.6159549300532));
#31086=CARTESIAN_POINT('Ctrl Pts',(-0.948977861495143,4.82782202743262,
39.6016024346359));
#31087=CARTESIAN_POINT('Ctrl Pts',(-0.812442962099693,4.85266540797225,
39.5936603580244));
#31088=CARTESIAN_POINT('Ctrl Pts',(-0.63388901456503,4.87740645159984,39.5834004383169));
#31089=CARTESIAN_POINT('Ctrl Pts',(-0.592667121670689,4.88258688764306,
39.5810406143829));
#31090=CARTESIAN_POINT('Ctrl Pts',(-0.50942959525157,4.89197783583892,39.5762956120336));
#31091=CARTESIAN_POINT('Ctrl Pts',(-0.46741541310621,4.89617080441049,39.5739107961787));
#31092=CARTESIAN_POINT('Ctrl Pts',(-0.399000421103954,4.90210988992745,
39.5700396873988));
#31093=CARTESIAN_POINT('Ctrl Pts',(-0.372630573636632,4.90418486342901,
39.5685505700832));
#31094=CARTESIAN_POINT('Ctrl Pts',(-0.193692573615001,4.91681344604834,
39.5584617011572));
#31095=CARTESIAN_POINT('Ctrl Pts',(-0.0407198531436483,4.92045869720686,
39.5499122295538));
#31096=CARTESIAN_POINT('Ctrl Pts',(0.237675233164923,4.91410746627151,39.5343040191604));
#31097=CARTESIAN_POINT('Ctrl Pts',(0.363019134542659,4.90644048785214,39.5272589346098));
#31098=CARTESIAN_POINT('Ctrl Pts',(0.550478308213643,4.88775078511209,39.516637712046));
#31099=CARTESIAN_POINT('Ctrl Pts',(0.612899795705358,4.88031636673526,39.5130870131365));
#31100=CARTESIAN_POINT('Ctrl Pts',(0.746886235170257,4.86174735103065,39.5054283840337));
#31101=CARTESIAN_POINT('Ctrl Pts',(0.81838241311975,4.85022436748832,39.5013186849675));
#31102=CARTESIAN_POINT('Ctrl Pts',(1.03455307575027,4.81046835603453,39.4888133427834));
#31103=CARTESIAN_POINT('Ctrl Pts',(1.17823548646428,4.77730741010397,39.4803902503027));
#31104=CARTESIAN_POINT('Ctrl Pts',(1.46288214905752,4.69798838529512,39.463476323209));
#31105=CARTESIAN_POINT('Ctrl Pts',(1.60368691055606,4.65180696472423,39.4549939643085));
#31106=CARTESIAN_POINT('Ctrl Pts',(1.78052716017062,4.58482130568957,39.4442323166427));
#31107=CARTESIAN_POINT('Ctrl Pts',(1.81867809098722,4.56982203514822,39.4419042139383));
#31108=CARTESIAN_POINT('Ctrl Pts',(1.89631494019438,4.53817239126163,39.4371555767541));
#31109=CARTESIAN_POINT('Ctrl Pts',(1.93577976217076,4.52147937903724,39.4347357018761));
#31110=CARTESIAN_POINT('Ctrl Pts',(1.99980215401641,4.49340700816309,39.4307956115768));
#31111=CARTESIAN_POINT('Ctrl Pts',(2.02449261170527,4.48233698777984,39.4292725625656));
#31112=CARTESIAN_POINT('Ctrl Pts',(2.18948049865964,4.40672296422198,39.4190668725454));
#31113=CARTESIAN_POINT('Ctrl Pts',(2.3267629568682,4.33580521688991,39.410434324733));
#31114=CARTESIAN_POINT('Ctrl Pts',(2.5668034932147,4.19711578312782,39.3948943487093));
#31115=CARTESIAN_POINT('Ctrl Pts',(2.67078647829326,4.13172604706275,39.3880019430391));
#31116=CARTESIAN_POINT('Ctrl Pts',(2.82401233012307,4.02716651299461,39.3775428649606));
#31117=CARTESIAN_POINT('Ctrl Pts',(2.87513116626288,3.99083154684322,39.37400020615));
#31118=CARTESIAN_POINT('Ctrl Pts',(2.98395227579363,3.9103058748551,39.3663350455311));
#31119=CARTESIAN_POINT('Ctrl Pts',(3.04139813112048,3.86579363923212,39.3622106663965));
#31120=CARTESIAN_POINT('Ctrl Pts',(3.15927050713853,3.7702054484251,39.3535757049503));
#31121=CARTESIAN_POINT('Ctrl Pts',(3.21949360144223,3.71891113607392,39.3490644714927));
#31122=CARTESIAN_POINT('Ctrl Pts',(3.409650195705,3.54886541152646,39.334488457462));
#31123=CARTESIAN_POINT('Ctrl Pts',(3.53445486657579,3.42458594224403,39.3243973802742));
#31124=CARTESIAN_POINT('Ctrl Pts',(3.692810595625,3.24899778386449,39.3108989219688));
#31125=CARTESIAN_POINT('Ctrl Pts',(3.73246186029148,3.20336780308052,39.3074550002844));
#31126=CARTESIAN_POINT('Ctrl Pts',(3.79485061794772,3.12884039994491,39.3019361833758));
#31127=CARTESIAN_POINT('Ctrl Pts',(3.81812244439937,3.10039908733556,39.2998544459276));
#31128=CARTESIAN_POINT('Ctrl Pts',(3.87869025885567,3.0246607362004,39.2943733011372));
#31129=CARTESIAN_POINT('Ctrl Pts',(3.91543997479883,2.97693477030682,39.2909814714282));
#31130=CARTESIAN_POINT('Ctrl Pts',(4.03333006413394,2.81787301114302,39.2798537812124));
#31131=CARTESIAN_POINT('Ctrl Pts',(4.11067045099002,2.70380261278462,39.2721493847202));
#31132=CARTESIAN_POINT('Ctrl Pts',(4.21707090008802,2.53173127072188,39.2608112220651));
#31133=CARTESIAN_POINT('Ctrl Pts',(4.2499368429498,2.47616376228464,39.2571913528747));
#31134=CARTESIAN_POINT('Ctrl Pts',(4.32729968765962,2.33928395105995,39.2483601270319));
#31135=CARTESIAN_POINT('Ctrl Pts',(4.37061002448932,2.25733021780282,39.2431440427045));
#31136=CARTESIAN_POINT('Ctrl Pts',(4.44131058089824,2.11387483281484,39.2341118950906));
#31137=CARTESIAN_POINT('Ctrl Pts',(4.46980168289862,2.05294404864993,39.23030529415));
#31138=CARTESIAN_POINT('Ctrl Pts',(4.53318897893135,1.90980461493238,39.2214233167043));
#31139=CARTESIAN_POINT('Ctrl Pts',(4.5671134619615,1.82719192339286,39.216342355559));
#31140=CARTESIAN_POINT('Ctrl Pts',(4.64008957660375,1.63472767797632,39.2045992667209));
#31141=CARTESIAN_POINT('Ctrl Pts',(4.67752242416655,1.52431935826938,39.1979311506441));
#31142=CARTESIAN_POINT('Ctrl Pts',(4.7480649890382,1.28907548577166,39.1838721818453));
#31143=CARTESIAN_POINT('Ctrl Pts',(4.78025306883592,1.16405235565174,39.1764856726978));
#31144=CARTESIAN_POINT('Ctrl Pts',(4.81635666307974,0.996823995008947,39.1667470189971));
#31145=CARTESIAN_POINT('Ctrl Pts',(4.82469940481146,0.955628217649391,39.1643593134903));
#31146=CARTESIAN_POINT('Ctrl Pts',(4.84027022024472,0.873331729859529,39.159614335306));
#31147=CARTESIAN_POINT('Ctrl Pts',(4.84750530856395,0.832235814823772,39.1572571841265));
#31148=CARTESIAN_POINT('Ctrl Pts',(4.8583943874849,0.765416044221063,39.1534403453621));
#31149=CARTESIAN_POINT('Ctrl Pts',(4.86236901657948,0.739746781968841,39.151977840823));
#31150=CARTESIAN_POINT('Ctrl Pts',(4.87177178080422,0.675668144782082,39.1483348516107));
#31151=CARTESIAN_POINT('Ctrl Pts',(4.87694922006158,0.637223707954985,39.1461562542479));
#31152=CARTESIAN_POINT('Ctrl Pts',(4.90074261961795,0.443224534146613,39.1351885635246));
#31153=CARTESIAN_POINT('Ctrl Pts',(4.91237335646857,0.286904716768253,39.1264321642819));
#31154=CARTESIAN_POINT('Ctrl Pts',(4.91923444692432,0.0280134831669276,
39.1118971280989));
#31155=CARTESIAN_POINT('Ctrl Pts',(4.91875260533546,-0.0743285839474307,
39.1061435218152));
#31156=CARTESIAN_POINT('Ctrl Pts',(4.91265210273125,-0.244135101471975,
39.0965527967804));
#31157=CARTESIAN_POINT('Ctrl Pts',(4.9088326281508,-0.31163235419062,39.0927290265234));
#31158=CARTESIAN_POINT('Ctrl Pts',(4.89721435249451,-0.461941857409463,
39.0841801486178));
#31159=CARTESIAN_POINT('Ctrl Pts',(4.88870372793514,-0.544678176938047,
39.0794514827065));
#31160=CARTESIAN_POINT('Ctrl Pts',(4.86514312858313,-0.727934904613118,
39.0689184545321));
#31161=CARTESIAN_POINT('Ctrl Pts',(4.8490669333082,-0.82828527111731,39.0631104686996));
#31162=CARTESIAN_POINT('Ctrl Pts',(4.79892384203584,-1.08924314946118,39.0479025562572));
#31163=CARTESIAN_POINT('Ctrl Pts',(4.75990457932159,-1.2487713559981,39.0384984560371));
#31164=CARTESIAN_POINT('Ctrl Pts',(4.70267666919145,-1.44059527716543,39.027110160454));
#31165=CARTESIAN_POINT('Ctrl Pts',(4.69199120515729,-1.47502582123768,39.0250630311218));
#31166=CARTESIAN_POINT('Ctrl Pts',(4.66811043924559,-1.54908762644346,39.0206545955774));
#31167=CARTESIAN_POINT('Ctrl Pts',(4.65478682240799,-1.58867467987585,39.0182951466843));
#31168=CARTESIAN_POINT('Ctrl Pts',(4.59841808967512,-1.7493571131665,39.0086950858514));
#31169=CARTESIAN_POINT('Ctrl Pts',(4.55113836542247,-1.86891399582052,39.0014969630169));
#31170=CARTESIAN_POINT('Ctrl Pts',(4.43706318923243,-2.12728546348757,38.985674225092));
#31171=CARTESIAN_POINT('Ctrl Pts',(4.36832167212134,-2.26509123902372,38.9770565349013));
#31172=CARTESIAN_POINT('Ctrl Pts',(4.25645034538123,-2.46525814720661,38.9641471208801));
#31173=CARTESIAN_POINT('Ctrl Pts',(4.2181602050814,-2.53021571861341,38.959893604808));
#31174=CARTESIAN_POINT('Ctrl Pts',(4.14171529562556,-2.65333983704687,38.9516944358007));
#31175=CARTESIAN_POINT('Ctrl Pts',(4.10378995201621,-2.7116278807087,38.9477514987004));
#31176=CARTESIAN_POINT('Ctrl Pts',(3.98594082008995,-2.88461402753731,38.9358531950217));
#31177=CARTESIAN_POINT('Ctrl Pts',(3.9023515181653,-2.99672722423762,38.9278724879442));
#31178=CARTESIAN_POINT('Ctrl Pts',(3.70845354506083,-3.23489680078571,38.9102989927824));
#31179=CARTESIAN_POINT('Ctrl Pts',(3.59625046210315,-3.35919161974612,38.9007086726743));
#31180=CARTESIAN_POINT('Ctrl Pts',(3.44831532434259,-3.50714396096354,38.8887991921053));
#31181=CARTESIAN_POINT('Ctrl Pts',(3.41832315609936,-3.5363829251366,38.8864198591102));
#31182=CARTESIAN_POINT('Ctrl Pts',(3.35760974500172,-3.59407747865262,38.8816751540646));
#31183=CARTESIAN_POINT('Ctrl Pts',(3.32689123134357,-3.62253100904149,38.8793099738672));
#31184=CARTESIAN_POINT('Ctrl Pts',(3.19706760101372,-3.73973795681526,38.8694496077892));
#31185=CARTESIAN_POINT('Ctrl Pts',(3.09474474986734,-3.82484469333287,38.8620001711711));
#31186=CARTESIAN_POINT('Ctrl Pts',(2.86161190001133,-4.0032651575686,38.8455537110574));
#31187=CARTESIAN_POINT('Ctrl Pts',(2.72942788170617,-4.09453015973498,38.8365636761315));
#31188=CARTESIAN_POINT('Ctrl Pts',(2.53157276894922,-4.21729196914811,38.8234460624785));
#31189=CARTESIAN_POINT('Ctrl Pts',(2.46929361425007,-4.25405701947805,38.8193635337122));
#31190=CARTESIAN_POINT('Ctrl Pts',(2.34381648906955,-4.32444541097243,38.8112193017649));
#31191=CARTESIAN_POINT('Ctrl Pts',(2.28064983350614,-4.35808903357751,38.8071587994209));
#31192=CARTESIAN_POINT('Ctrl Pts',(2.18127633109587,-4.40826471524024,38.8008265465051));
#31193=CARTESIAN_POINT('Ctrl Pts',(2.14556461847156,-4.42575605697535,38.7985619023984));
#31194=CARTESIAN_POINT('Ctrl Pts',(1.9957484613591,-4.49689543053981,38.789105664532));
#31195=CARTESIAN_POINT('Ctrl Pts',(1.8798152508781,-4.54657834076028,38.7818928878107));
#31196=CARTESIAN_POINT('Ctrl Pts',(1.63997090369856,-4.63861953808499,38.7671867562889));
#31197=CARTESIAN_POINT('Ctrl Pts',(1.51601722892208,-4.68059698128877,38.7596987394821));
#31198=CARTESIAN_POINT('Ctrl Pts',(1.3503280354426,-4.72943490070241,38.749866099238));
#31199=CARTESIAN_POINT('Ctrl Pts',(1.30996894616915,-4.74077226801363,38.7474847502543));
#31200=CARTESIAN_POINT('Ctrl Pts',(1.22905255661804,-4.76239047212999,38.7427400005994));
#31201=CARTESIAN_POINT('Ctrl Pts',(1.18849910264559,-4.77267253568953,38.7403767747798));
#31202=CARTESIAN_POINT('Ctrl Pts',(1.14580002865878,-4.7829206211638,38.7379012040744));
#31203=CARTESIAN_POINT('Ctrl Pts',(1.14378063822835,-4.78340393711924,38.7377841552889));
#31204=CARTESIAN_POINT('Ctrl Pts',(1.13955837206968,-4.78441165733066,38.737539483943));
#31205=CARTESIAN_POINT('Ctrl Pts',(1.13735543891617,-4.78493581939512,38.7374118636207));
#31206=CARTESIAN_POINT('Ctrl Pts',(1.13273759460993,-4.78603121201167,38.7371444151133));
#31207=CARTESIAN_POINT('Ctrl Pts',(1.13032261139427,-4.78660213666986,38.7370045896998));
#31208=CARTESIAN_POINT('Ctrl Pts',(1.12715956771992,-4.78734738256734,38.7368215059007));
#31209=CARTESIAN_POINT('Ctrl Pts',(1.12641189787147,-4.78752335647679,38.7367782330802));
#31210=CARTESIAN_POINT('Ctrl Pts',(1.12470692845255,-4.78792422189296,38.7366795636331));
#31211=CARTESIAN_POINT('Ctrl Pts',(1.12374960255776,-4.78814900146709,38.7366241679812));
#31212=CARTESIAN_POINT('Ctrl Pts',(1.12156137598197,-4.78866210341169,38.7364975608455));
#31213=CARTESIAN_POINT('Ctrl Pts',(1.12033043132739,-4.78895023834961,38.7364263509783));
#31214=CARTESIAN_POINT('Ctrl Pts',(1.06223654430143,-4.80252501455946,38.7330661267533));
#31215=CARTESIAN_POINT('Ctrl Pts',(1.00514122116211,-4.81479845911944,38.7297859349637));
#31216=CARTESIAN_POINT('Ctrl Pts',(0.78050394419513,-4.85891740162198,38.7169419842515));
#31217=CARTESIAN_POINT('Ctrl Pts',(0.611571474909233,-4.88305693549449,
38.7074128759114));
#31218=CARTESIAN_POINT('Ctrl Pts',(0.349264561199292,-4.90671134325719,
38.6926201216086));
#31219=CARTESIAN_POINT('Ctrl Pts',(0.256585154504632,-4.91242971500897,
38.6873950383847));
#31220=CARTESIAN_POINT('Ctrl Pts',(0.098595075308817,-4.91769443130679,
38.6784676655964));
#31221=CARTESIAN_POINT('Ctrl Pts',(0.0333535360516099,-4.91856960186443,
38.6747753858831));
#31222=CARTESIAN_POINT('Ctrl Pts',(-0.109510367245702,-4.91764337860662,
38.666670761035));
#31223=CARTESIAN_POINT('Ctrl Pts',(-0.18711168213534,-4.91530242668106,
38.6622558641897));
#31224=CARTESIAN_POINT('Ctrl Pts',(-0.366305919494645,-4.90564696914728,
38.652025460237));
#31225=CARTESIAN_POINT('Ctrl Pts',(-0.467792071977703,-4.89701159036208,
38.6462046449401));
#31226=CARTESIAN_POINT('Ctrl Pts',(-0.731590117253801,-4.8662895621965,
38.6310052437245));
#31227=CARTESIAN_POINT('Ctrl Pts',(-0.89319775116091,-4.83923514659879,
38.6216226876822));
#31228=CARTESIAN_POINT('Ctrl Pts',(-1.08834251606943,-4.79645611658005,
38.6102572419994));
#31229=CARTESIAN_POINT('Ctrl Pts',(-1.12344427202847,-4.78835605539061,
38.6082116258924));
#31230=CARTESIAN_POINT('Ctrl Pts',(-1.19347508286451,-4.77138332144673,
38.6041294523743));
#31231=CARTESIAN_POINT('Ctrl Pts',(-1.22840197390703,-4.76251091327946,
38.6020930300535));
#31232=CARTESIAN_POINT('Ctrl Pts',(-1.26658014263471,-4.75236465690808,
38.5998646704706));
#31233=CARTESIAN_POINT('Ctrl Pts',(-1.26993091771608,-4.75147035707909,
38.5996690744923));
#31234=CARTESIAN_POINT('Ctrl Pts',(-1.27712730916522,-4.74954153131194,
38.5992489508562));
#31235=CARTESIAN_POINT('Ctrl Pts',(-1.28097262117994,-4.74850587714698,
38.5990244341232));
#31236=CARTESIAN_POINT('Ctrl Pts',(-1.28932319287547,-4.74624594421492,
38.5985368019319));
#31237=CARTESIAN_POINT('Ctrl Pts',(-1.29382797660832,-4.74501991836387,
38.5982737028405));
#31238=CARTESIAN_POINT('Ctrl Pts',(-1.3004400014129,-4.74321026797663,38.5978874649188));
#31239=CARTESIAN_POINT('Ctrl Pts',(-1.30254860740403,-4.74263165013583,
38.5977642818467));
#31240=CARTESIAN_POINT('Ctrl Pts',(-1.30800436124589,-4.74113063600515,
38.5974455343492));
#31241=CARTESIAN_POINT('Ctrl Pts',(-1.31135092042317,-4.74020610102918,
38.5972499885996));
#31242=CARTESIAN_POINT('Ctrl Pts',(-1.32012002824678,-4.73777351207704,
38.5967375211165));
#31243=CARTESIAN_POINT('Ctrl Pts',(-1.32554097458688,-4.73625969151886,
38.5964206482785));
#31244=CARTESIAN_POINT('Ctrl Pts',(-1.39434857854842,-4.71691751268915,
38.5923976148445));
#31245=CARTESIAN_POINT('Ctrl Pts',(-1.45737400449448,-4.6978271463955,38.5887018504978));
#31246=CARTESIAN_POINT('Ctrl Pts',(-1.73102000633406,-4.60890287719874,
38.5725684115556));
#31247=CARTESIAN_POINT('Ctrl Pts',(-1.93715838440445,-4.52612773716528,
38.5601753831499));
#31248=CARTESIAN_POINT('Ctrl Pts',(-2.18812955254942,-4.40505330480025,
38.544465955373));
#31249=CARTESIAN_POINT('Ctrl Pts',(-2.23882669251638,-4.37950459753855,
38.5412600158807));
#31250=CARTESIAN_POINT('Ctrl Pts',(-2.34420031919172,-4.32409386226783,
38.534522467246));
#31251=CARTESIAN_POINT('Ctrl Pts',(-2.39877464489883,-4.29405903118504,
38.5309901082451));
#31252=CARTESIAN_POINT('Ctrl Pts',(-2.51457123515964,-4.2274341413938,38.5233974296439));
#31253=CARTESIAN_POINT('Ctrl Pts',(-2.57559792278348,-4.19053255777091,
38.5193355979906));
#31254=CARTESIAN_POINT('Ctrl Pts',(-2.74226922564166,-4.0847332619287,38.5080686675776));
#31255=CARTESIAN_POINT('Ctrl Pts',(-2.84609889261695,-4.01307950018809,
38.5008500254866));
#31256=CARTESIAN_POINT('Ctrl Pts',(-2.97302490791104,-3.91808089209701,
38.4917750617003));
#31257=CARTESIAN_POINT('Ctrl Pts',(-2.99879790881972,-3.89839019167147,
38.4899188755996));
#31258=CARTESIAN_POINT('Ctrl Pts',(-3.0502715924491,-3.85825151621077,38.4861849763177));
#31259=CARTESIAN_POINT('Ctrl Pts',(-3.07596605150839,-3.83779811999458,
38.4843073764962));
#31260=CARTESIAN_POINT('Ctrl Pts',(-3.14869659537006,-3.77870323698239,
38.4789542433377));
#31261=CARTESIAN_POINT('Ctrl Pts',(-3.1952230868871,-3.73944353396493,38.4754831124882));
#31262=CARTESIAN_POINT('Ctrl Pts',(-3.26922617887872,-3.67460890286862,
38.4698904078534));
#31263=CARTESIAN_POINT('Ctrl Pts',(-3.29715967091668,-3.64956553033259,
38.4677623973218));
#31264=CARTESIAN_POINT('Ctrl Pts',(-3.35992050289029,-3.59198945593125,
38.4629432954941));
#31265=CARTESIAN_POINT('Ctrl Pts',(-3.39456698019871,-3.55926525103117,
38.4602550965803));
#31266=CARTESIAN_POINT('Ctrl Pts',(-3.45282208457417,-3.50261783925194,
38.4556805321384));
#31267=CARTESIAN_POINT('Ctrl Pts',(-3.47667092006059,-3.4789468818189,38.4537916343882));
#31268=CARTESIAN_POINT('Ctrl Pts',(-3.57977881714836,-3.37448883369365,
38.4455485711046));
#31269=CARTESIAN_POINT('Ctrl Pts',(-3.65647876685172,-3.29122386186867,
38.4392149358211));
#31270=CARTESIAN_POINT('Ctrl Pts',(-3.82294254343825,-3.09750324837499,
38.4249035794577));
#31271=CARTESIAN_POINT('Ctrl Pts',(-3.91092205507343,-2.98564968185524,
38.416927298866));
#31272=CARTESIAN_POINT('Ctrl Pts',(-4.03410624633866,-2.81423342762668,
38.405027667454));
#31273=CARTESIAN_POINT('Ctrl Pts',(-4.07310468205173,-2.75748818700039,
38.4011383913222));
#31274=CARTESIAN_POINT('Ctrl Pts',(-4.11685570183872,-2.69087345347245,
38.3966247162756));
#31275=CARTESIAN_POINT('Ctrl Pts',(-4.12278261567562,-2.68178379361217,
38.3960099246217));
#31276=CARTESIAN_POINT('Ctrl Pts',(-4.17064502236606,-2.60784717153851,
38.3910179608201));
#31277=CARTESIAN_POINT('Ctrl Pts',(-4.21107761584773,-2.54204089098516,
38.3866297731041));
#31278=CARTESIAN_POINT('Ctrl Pts',(-4.29562213547851,-2.39688356770791,
38.3770606821016));
#31279=CARTESIAN_POINT('Ctrl Pts',(-4.33912064763474,-2.31720783433195,
38.3718773626993));
#31280=CARTESIAN_POINT('Ctrl Pts',(-4.45407414201297,-2.09204832402128,
38.357416983894));
#31281=CARTESIAN_POINT('Ctrl Pts',(-4.52058115066674,-1.94416795913786,
38.3481284516612));
#31282=CARTESIAN_POINT('Ctrl Pts',(-4.59832478621222,-1.74562616652423,
38.3359701872842));
#31283=CARTESIAN_POINT('Ctrl Pts',(-4.61623803360097,-1.69768903375906,
38.3330581733992));
#31284=CARTESIAN_POINT('Ctrl Pts',(-4.6456379223541,-1.61510459136912,38.3280849867555));
#31285=CARTESIAN_POINT('Ctrl Pts',(-4.65749278056879,-1.58059342382598,
38.3260199867548));
#31286=CARTESIAN_POINT('Ctrl Pts',(-4.69033268897614,-1.48141298564855,
38.3201198589345));
#31287=CARTESIAN_POINT('Ctrl Pts',(-4.71036241766494,-1.41643610183184,
38.3162953629141));
#31288=CARTESIAN_POINT('Ctrl Pts',(-4.78146111828876,-1.16757414712526,
38.3017621176116));
#31289=CARTESIAN_POINT('Ctrl Pts',(-4.82315968132596,-0.981188428389662,
38.2911070746136));
#31290=CARTESIAN_POINT('Ctrl Pts',(-4.8686028279121,-0.702980734757526,
38.2752712097921));
#31291=CARTESIAN_POINT('Ctrl Pts',(-4.88078369307783,-0.612719895725724,
38.2701450987969));
#31292=CARTESIAN_POINT('Ctrl Pts',(-4.89708474214341,-0.46005138977395,
38.2614731311142));
#31293=CARTESIAN_POINT('Ctrl Pts',(-4.90253346691393,-0.397808687289228,
38.2579372395336));
#31294=CARTESIAN_POINT('Ctrl Pts',(-4.91024137641091,-0.285071165663136,
38.2515272870964));
#31295=CARTESIAN_POINT('Ctrl Pts',(-4.91291081207015,-0.234612962061103,
38.248656387333));
#31296=CARTESIAN_POINT('Ctrl Pts',(-4.91710205017738,-0.12273600534833,
38.2422845533916));
#31297=CARTESIAN_POINT('Ctrl Pts',(-4.91825146531259,-0.0613118016263361,
38.2387818971424));
#31298=CARTESIAN_POINT('Ctrl Pts',(-4.91824999859808,0.000117430551467993,
38.2352739421131));
#31299=CARTESIAN_POINT('Ctrl Pts',(-4.76417305830272,1.22198379731345,38.1652023751175));
#31300=CARTESIAN_POINT('Ctrl Pts',(-4.79992959697842,1.08317356408338,38.1733206669997));
#31301=CARTESIAN_POINT('Ctrl Pts',(-4.88511646459839,0.68011126137427,38.1966333966303));
#31302=CARTESIAN_POINT('Ctrl Pts',(-4.91823750901205,0.268450859973121,
38.2199461262609));
#31303=CARTESIAN_POINT('Ctrl Pts',(-4.91801823864715,0.000109808377098883,
38.2351405640093));
#31304=CARTESIAN_POINT('',(-4.91786390629002,-3.8137431901149E-5,37.8898484442262));
#31305=CARTESIAN_POINT('Ctrl Pts',(-4.76403458711433,1.22194824574464,37.8201594747841));
#31306=CARTESIAN_POINT('Ctrl Pts',(-4.77168918472963,1.19210510965708,37.8218969884493));
#31307=CARTESIAN_POINT('Ctrl Pts',(-4.77906333949699,1.16219014635735,37.8236317891998));
#31308=CARTESIAN_POINT('Ctrl Pts',(-4.82722030109097,0.958617240570028,
37.835397210521));
#31309=CARTESIAN_POINT('Ctrl Pts',(-4.85881042990668,0.782920717595789,
37.8453594523882));
#31310=CARTESIAN_POINT('Ctrl Pts',(-4.89436812730833,0.496486354594997,
37.861548849846));
#31311=CARTESIAN_POINT('Ctrl Pts',(-4.90426733166406,0.386651749871982,
37.8677434591192));
#31312=CARTESIAN_POINT('Ctrl Pts',(-4.91315075192891,0.228932496530562,
37.8766552215315));
#31313=CARTESIAN_POINT('Ctrl Pts',(-4.91514075959246,0.181250284693678,
37.8793514780635));
#31314=CARTESIAN_POINT('Ctrl Pts',(-4.91764592424943,0.0890244001506232,
37.8845731483227));
#31315=CARTESIAN_POINT('Ctrl Pts',(-4.91825045937924,0.0444877371853263,
37.8870977200385));
#31316=CARTESIAN_POINT('Ctrl Pts',(-4.91824999973809,-5.07567696672655E-5,
37.8896262308883));
#31317=CARTESIAN_POINT('Ctrl Pts',(-4.91784480820938,-3.75132173967632E-5,
37.8898594359907));
#31318=CARTESIAN_POINT('Ctrl Pts',(-4.91794292181926,-0.368586153414599,
37.9107258822996));
#31319=CARTESIAN_POINT('Ctrl Pts',(-4.78626629645783,-1.55553496917534,
37.9779323271126));
#31320=CARTESIAN_POINT('Ctrl Pts',(-3.84145891917051,-3.39576550157761,
38.0914787704297));
#31321=CARTESIAN_POINT('Ctrl Pts',(-1.74734491989153,-4.82025058480454,
38.2304987659423));
#31322=CARTESIAN_POINT('Ctrl Pts',(0.773133994074016,-5.06855934133029,
38.3695187614548));
#31323=CARTESIAN_POINT('Ctrl Pts',(3.10496257022011,-4.08010262210541,38.5085387569673));
#31324=CARTESIAN_POINT('Ctrl Pts',(4.67915761546661,-2.09607108157144,38.6475587524798));
#31325=CARTESIAN_POINT('Ctrl Pts',(5.11160404839724,0.399417102523584,38.7865787479924));
#31326=CARTESIAN_POINT('Ctrl Pts',(4.29678178286066,2.79744459817457,38.9255987435048));
#31327=CARTESIAN_POINT('Ctrl Pts',(2.43351339920456,4.51287519274255,39.0646187390174));
#31328=CARTESIAN_POINT('Ctrl Pts',(-0.0235500165765371,5.12713129986921,
39.2036387345299));
#31329=CARTESIAN_POINT('Ctrl Pts',(-2.47486705641651,4.49032994583289,39.3426587300424));
#31330=CARTESIAN_POINT('Ctrl Pts',(-4.09737808320941,2.96877998133387,39.4647533712912));
#31331=CARTESIAN_POINT('Ctrl Pts',(-4.63432213820682,1.72499203924927,39.5405080140358));
#31332=CARTESIAN_POINT('Ctrl Pts',(-4.76374161084644,1.22187275725133,39.5699226582762));
#31333=CARTESIAN_POINT('Origin',(0.,0.,-3.23514056400928));
#31334=CARTESIAN_POINT('',(-4.76403458703735,1.22194824604475,41.6649672278726));
#31335=CARTESIAN_POINT('',(-4.76403458753695,1.22194824409695,41.3199466556564));
#31336=CARTESIAN_POINT('',(-4.76403458704967,1.22194824599672,-3.23514056400928));
#31337=CARTESIAN_POINT('Ctrl Pts',(-4.76403458703735,1.22194824604475,41.6649672278726));
#31338=CARTESIAN_POINT('Ctrl Pts',(-4.76127012557744,1.23272610840693,41.6643359433539));
#31339=CARTESIAN_POINT('Ctrl Pts',(-4.75846907609556,1.2434946412027,41.6637050875201));
#31340=CARTESIAN_POINT('Ctrl Pts',(-4.74504793833352,1.29438226263213,41.6607234763439));
#31341=CARTESIAN_POINT('Ctrl Pts',(-4.73395682140785,1.33437560005354,41.658378907746));
#31342=CARTESIAN_POINT('Ctrl Pts',(-4.67508088305431,1.53669590136459,41.6464987161115));
#31343=CARTESIAN_POINT('Ctrl Pts',(-4.61944724187694,1.69662136101325,41.6370405664665));
#31344=CARTESIAN_POINT('Ctrl Pts',(-4.51357840235773,1.95685364602639,41.6212973888434));
#31345=CARTESIAN_POINT('Ctrl Pts',(-4.4679615957932,2.05887955640786,41.6150315473424));
#31346=CARTESIAN_POINT('Ctrl Pts',(-4.39098051602284,2.21642060072307,41.6051614540538));
#31347=CARTESIAN_POINT('Ctrl Pts',(-4.36194457291228,2.27303093021728,41.6015740438707));
#31348=CARTESIAN_POINT('Ctrl Pts',(-4.30107521832979,2.38624176509895,41.5943090217789));
#31349=CARTESIAN_POINT('Ctrl Pts',(-4.26920264831027,2.44280707843993,41.5906317800841));
#31350=CARTESIAN_POINT('Ctrl Pts',(-4.18718885180447,2.58184941225385,41.5814668750217));
#31351=CARTESIAN_POINT('Ctrl Pts',(-4.13572222172027,2.66351238507201,41.5759705967678));
#31352=CARTESIAN_POINT('Ctrl Pts',(-3.99093908488945,2.87891797954815,41.5611512126468));
#31353=CARTESIAN_POINT('Ctrl Pts',(-3.8933195210266,3.00962227236982,41.5518084117889));
#31354=CARTESIAN_POINT('Ctrl Pts',(-3.74360396144366,3.19057538634981,41.5383803318057));
#31355=CARTESIAN_POINT('Ctrl Pts',(-3.69661045832224,3.24490573029522,41.5342800811727));
#31356=CARTESIAN_POINT('Ctrl Pts',(-3.6261955408353,3.32279846319194,41.5283064202999));
#31357=CARTESIAN_POINT('Ctrl Pts',(-3.60369888278384,3.34718360963317,41.5264221623577));
#31358=CARTESIAN_POINT('Ctrl Pts',(-3.5534321376645,3.40057575898001,41.5222662582524));
#31359=CARTESIAN_POINT('Ctrl Pts',(-3.52555012892606,3.42947397930547,41.5199968785908));
#31360=CARTESIAN_POINT('Ctrl Pts',(-3.43486186490294,3.52119262246206,41.5127219175477));
#31361=CARTESIAN_POINT('Ctrl Pts',(-3.3707062478194,3.58265449201192,41.5077350954234));
#31362=CARTESIAN_POINT('Ctrl Pts',(-3.19853901279424,3.73887225268478,41.4947001992828));
#31363=CARTESIAN_POINT('Ctrl Pts',(-3.08797963509335,3.83069174281939,41.4866669955951));
#31364=CARTESIAN_POINT('Ctrl Pts',(-2.914308013696,3.96251504192322,41.4744266560372));
#31365=CARTESIAN_POINT('Ctrl Pts',(-2.85404320278021,4.00613952749576,41.4702442694101));
#31366=CARTESIAN_POINT('Ctrl Pts',(-2.74097827088411,4.08413842010144,41.462501859737));
#31367=CARTESIAN_POINT('Ctrl Pts',(-2.68846237352837,4.11889772584592,41.4589455778651));
#31368=CARTESIAN_POINT('Ctrl Pts',(-2.57813592491649,4.18891166886341,41.4515492150936));
#31369=CARTESIAN_POINT('Ctrl Pts',(-2.52023558181634,4.22400027151912,41.4477086358015));
#31370=CARTESIAN_POINT('Ctrl Pts',(-2.27203187227084,4.36749547096227,41.4314054757767));
#31371=CARTESIAN_POINT('Ctrl Pts',(-2.07532605824382,4.4643213175208,41.4188642024773));
#31372=CARTESIAN_POINT('Ctrl Pts',(-1.80154390889707,4.57706955416008,41.4019256048073));
#31373=CARTESIAN_POINT('Ctrl Pts',(-1.72957954469765,4.60474547902596,41.3975207409046));
#31374=CARTESIAN_POINT('Ctrl Pts',(-1.64205675192484,4.63606345670309,41.3922268003096));
#31375=CARTESIAN_POINT('Ctrl Pts',(-1.62709372730172,4.64133609601798,41.3913239502535));
#31376=CARTESIAN_POINT('Ctrl Pts',(-1.58083908428008,4.65738404150837,41.3885399932151));
#31377=CARTESIAN_POINT('Ctrl Pts',(-1.5494638195863,4.66791604738023,41.3866614306249));
#31378=CARTESIAN_POINT('Ctrl Pts',(-1.47705507728195,4.69141161654292,41.382349908059));
#31379=CARTESIAN_POINT('Ctrl Pts',(-1.4359528809273,4.70415497607896,41.379919843149));
#31380=CARTESIAN_POINT('Ctrl Pts',(-1.19522586104527,4.77534109809547,41.3657717301727));
#31381=CARTESIAN_POINT('Ctrl Pts',(-0.992220497007273,4.82161256708251,
41.3541679785016));
#31382=CARTESIAN_POINT('Ctrl Pts',(-0.708083399112774,4.86766631645762,
41.3380193845171));
#31383=CARTESIAN_POINT('Ctrl Pts',(-0.628973195036945,4.87851924570152,
41.333534174749));
#31384=CARTESIAN_POINT('Ctrl Pts',(-0.48712049490661,4.89447178982773,41.3254937797367));
#31385=CARTESIAN_POINT('Ctrl Pts',(-0.424477867849351,4.90030192070997,
41.3219438746532));
#31386=CARTESIAN_POINT('Ctrl Pts',(-0.294555258300993,4.90988378166817,
41.3145755311625));
#31387=CARTESIAN_POINT('Ctrl Pts',(-0.22727524051386,4.91345778250953,41.3107566670574));
#31388=CARTESIAN_POINT('Ctrl Pts',(-0.0477222785081193,4.91930001104523,
41.3005488390981));
#31389=CARTESIAN_POINT('Ctrl Pts',(0.0645899568266395,4.91910740345627,
41.294146191484));
#31390=CARTESIAN_POINT('Ctrl Pts',(0.318021825071502,4.90999142257998,41.2796492933961));
#31391=CARTESIAN_POINT('Ctrl Pts',(0.458963024904282,4.89882705562738,41.2715516604399));
#31392=CARTESIAN_POINT('Ctrl Pts',(0.646351159819651,4.87582478765226,41.260760374117));
#31393=CARTESIAN_POINT('Ctrl Pts',(0.693389027364387,4.86935815922265,41.2580496634431));
#31394=CARTESIAN_POINT('Ctrl Pts',(0.75509310129909,4.85996302360793,41.254492996489));
#31395=CARTESIAN_POINT('Ctrl Pts',(0.769849820403595,4.8576473151558,41.2536423531267));
#31396=CARTESIAN_POINT('Ctrl Pts',(0.790498206432284,4.85431059949587,41.2524520767375));
#31397=CARTESIAN_POINT('Ctrl Pts',(0.796398882350495,4.85334602424806,41.2521119310035));
#31398=CARTESIAN_POINT('Ctrl Pts',(0.834542189679698,4.84703935620124,41.2499131646396));
#31399=CARTESIAN_POINT('Ctrl Pts',(0.866732850906196,4.8413867206099,41.2480575914216));
#31400=CARTESIAN_POINT('Ctrl Pts',(0.939772114062169,4.82780930199566,41.2438487777712));
#31401=CARTESIAN_POINT('Ctrl Pts',(0.980581426389653,4.81968613089237,41.241498221529));
#31402=CARTESIAN_POINT('Ctrl Pts',(1.15576708138316,4.78249793214748,41.2314012733404));
#31403=CARTESIAN_POINT('Ctrl Pts',(1.28899648590461,4.74832316799393,41.2237043983724));
#31404=CARTESIAN_POINT('Ctrl Pts',(1.57361139306861,4.66245291709921,41.207049933443));
#31405=CARTESIAN_POINT('Ctrl Pts',(1.72426065722136,4.60886584550659,41.1980993591963));
#31406=CARTESIAN_POINT('Ctrl Pts',(1.93824741008034,4.5207861376355,41.1850604484116));
#31407=CARTESIAN_POINT('Ctrl Pts',(2.00385879921705,4.49208861025668,41.181017136032));
#31408=CARTESIAN_POINT('Ctrl Pts',(2.13437915203234,4.43157203681371,41.1728718296125));
#31409=CARTESIAN_POINT('Ctrl Pts',(2.19926015001516,4.39973405004222,41.1687706267095));
#31410=CARTESIAN_POINT('Ctrl Pts',(2.40670357795528,4.29220330295604,41.1554771674057));
#31411=CARTESIAN_POINT('Ctrl Pts',(2.54624714685475,4.21092099440199,41.1462496963559));
#31412=CARTESIAN_POINT('Ctrl Pts',(2.76021925332452,4.07175414611854,41.1316381030135));
#31413=CARTESIAN_POINT('Ctrl Pts',(2.83741793384337,4.01833942818293,41.1262653315481));
#31414=CARTESIAN_POINT('Ctrl Pts',(2.9624680785184,3.9264142851043,41.1174042451881));
#31415=CARTESIAN_POINT('Ctrl Pts',(3.01121138725378,3.88915831070677,41.1139087209731));
#31416=CARTESIAN_POINT('Ctrl Pts',(3.08802281659371,3.82813909206122,41.108338165352));
#31417=CARTESIAN_POINT('Ctrl Pts',(3.11654315697061,3.80495632252344,41.1062559742967));
#31418=CARTESIAN_POINT('Ctrl Pts',(3.19044983606742,3.74349273800337,41.1008226890684));
#31419=CARTESIAN_POINT('Ctrl Pts',(3.23540757819331,3.70470592141908,41.0974788414106));
#31420=CARTESIAN_POINT('Ctrl Pts',(3.4037301011422,3.55408596325554,41.0847825342693));
#31421=CARTESIAN_POINT('Ctrl Pts',(3.52209022323534,3.43682799440656,41.0754798461348));
#31422=CARTESIAN_POINT('Ctrl Pts',(3.71128779954039,3.22933280322472,41.059731337927));
#31423=CARTESIAN_POINT('Ctrl Pts',(3.7853316133196,3.1422144405286,41.0533100279584));
#31424=CARTESIAN_POINT('Ctrl Pts',(3.89864898287532,2.99906331369223,41.0430098556726));
#31425=CARTESIAN_POINT('Ctrl Pts',(3.9399058912837,2.94465381343115,41.0391496909832));
#31426=CARTESIAN_POINT('Ctrl Pts',(4.02648296510146,2.82539799668982,41.0307968407793));
#31427=CARTESIAN_POINT('Ctrl Pts',(4.07139838603363,2.76028148596165,41.0263020120701));
#31428=CARTESIAN_POINT('Ctrl Pts',(4.19225613370118,2.57569507955791,41.0137319866517));
#31429=CARTESIAN_POINT('Ctrl Pts',(4.26464014440258,2.45398866927749,41.0056361057063));
#31430=CARTESIAN_POINT('Ctrl Pts',(4.39300520140962,2.21527832575622,40.9901206837461));
#31431=CARTESIAN_POINT('Ctrl Pts',(4.44980870248769,2.09884630724671,40.9827085399044));
#31432=CARTESIAN_POINT('Ctrl Pts',(4.51877714079427,1.94205625501779,40.9729586557662));
#31433=CARTESIAN_POINT('Ctrl Pts',(4.535115022309,1.90359164067747,40.9705848043272));
#31434=CARTESIAN_POINT('Ctrl Pts',(4.56462476294707,1.83157919888971,40.9661761248724));
#31435=CARTESIAN_POINT('Ctrl Pts',(4.57792191807458,1.79808579765527,40.9641397503168));
#31436=CARTESIAN_POINT('Ctrl Pts',(4.64967272521397,1.61140022607851,40.9528582216726));
#31437=CARTESIAN_POINT('Ctrl Pts',(4.70080603863717,1.45550370805503,40.9436896444015));
#31438=CARTESIAN_POINT('Ctrl Pts',(4.77088618060545,1.19923829566586,40.9288041962419));
#31439=CARTESIAN_POINT('Ctrl Pts',(4.79466491796991,1.10032519941727,40.9231030361316));
#31440=CARTESIAN_POINT('Ctrl Pts',(4.83228980989685,0.919282989847636,40.9127060638676));
#31441=CARTESIAN_POINT('Ctrl Pts',(4.84714979631333,0.837403516293261,40.9080178496487));
#31442=CARTESIAN_POINT('Ctrl Pts',(4.87030432989658,0.688395029301021,40.8994949259284));
#31443=CARTESIAN_POINT('Ctrl Pts',(4.87930509953652,0.621396485327472,40.8956660709592));
#31444=CARTESIAN_POINT('Ctrl Pts',(4.89844165093083,0.452661270867243,40.8860234273353));
#31445=CARTESIAN_POINT('Ctrl Pts',(4.90679156300431,0.35075487925224,40.8801997175755));
#31446=CARTESIAN_POINT('Ctrl Pts',(4.91988711428797,0.0920726518648833,
40.8654051299495));
#31447=CARTESIAN_POINT('Ctrl Pts',(4.92032176764996,-0.0648074796190918,
40.8564201614287));
#31448=CARTESIAN_POINT('Ctrl Pts',(4.91151532301408,-0.260203900777127,
40.8452378296772));
#31449=CARTESIAN_POINT('Ctrl Pts',(4.9093094790622,-0.298946982803085,40.8430212267564));
#31450=CARTESIAN_POINT('Ctrl Pts',(4.90486167097758,-0.363579498427921,
40.8393255995916));
#31451=CARTESIAN_POINT('Ctrl Pts',(4.90287261503604,-0.389484522573766,
40.837844964514));
#31452=CARTESIAN_POINT('Ctrl Pts',(4.89715386951535,-0.456955821325617,
40.8339907258432));
#31453=CARTESIAN_POINT('Ctrl Pts',(4.89310020846959,-0.498492777046296,
40.8316201046153));
#31454=CARTESIAN_POINT('Ctrl Pts',(4.88455800569197,-0.575827538727203,
40.8272125631839));
#31455=CARTESIAN_POINT('Ctrl Pts',(4.88020329122169,-0.611637259458739,
40.8251741172176));
#31456=CARTESIAN_POINT('Ctrl Pts',(4.85382436935202,-0.810293466766594,
40.8138701301806));
#31457=CARTESIAN_POINT('Ctrl Pts',(4.82404304726574,-0.972006434915165,
40.8046814331215));
#31458=CARTESIAN_POINT('Ctrl Pts',(4.76286889319268,-1.23067442687123,40.7897887058167));
#31459=CARTESIAN_POINT('Ctrl Pts',(4.73646500303619,-1.32867554207821,40.7841006304361));
#31460=CARTESIAN_POINT('Ctrl Pts',(4.68295779333109,-1.50532231612577,40.7737225104314));
#31461=CARTESIAN_POINT('Ctrl Pts',(4.65685509938529,-1.58423146298085,40.7690400081237));
#31462=CARTESIAN_POINT('Ctrl Pts',(4.60591444700487,-1.7260665128362,40.7605221570072));
#31463=CARTESIAN_POINT('Ctrl Pts',(4.58175369392048,-1.78921392019121,40.7566926237168));
#31464=CARTESIAN_POINT('Ctrl Pts',(4.51772548402142,-1.94674980259616,40.7470366110536));
#31465=CARTESIAN_POINT('Ctrl Pts',(4.47619631815472,-2.04042751803428,40.7412001331203));
#31466=CARTESIAN_POINT('Ctrl Pts',(4.3639116619959,-2.27375192740842,40.726409692148));
#31467=CARTESIAN_POINT('Ctrl Pts',(4.28935928111048,-2.41144552078567,40.7174418803514));
#31468=CARTESIAN_POINT('Ctrl Pts',(4.18830501496816,-2.5785242576005,40.7062786111037));
#31469=CARTESIAN_POINT('Ctrl Pts',(4.16784819878627,-2.61146082850883,40.7040639264697));
#31470=CARTESIAN_POINT('Ctrl Pts',(4.13304389542213,-2.66604678875744,40.7003710345483));
#31471=CARTESIAN_POINT('Ctrl Pts',(4.11891055103188,-2.687830575652,40.6988912189603));
#31472=CARTESIAN_POINT('Ctrl Pts',(4.08162285119034,-2.74431745765307,40.6950386506098));
#31473=CARTESIAN_POINT('Ctrl Pts',(4.05819816463289,-2.77883988724328,40.6926688797651));
#31474=CARTESIAN_POINT('Ctrl Pts',(4.01029230312024,-2.84754384696619,40.6879241974873));
#31475=CARTESIAN_POINT('Ctrl Pts',(3.98580635563148,-2.88171790208906,40.6855495605213));
#31476=CARTESIAN_POINT('Ctrl Pts',(3.88445472840469,-3.01940678943945,40.6759114796982));
#31477=CARTESIAN_POINT('Ctrl Pts',(3.80397018577044,-3.12019509478082,40.6686905226161));
#31478=CARTESIAN_POINT('Ctrl Pts',(3.64333477628409,-3.30588716271997,40.6549352870396));
#31479=CARTESIAN_POINT('Ctrl Pts',(3.56394043146482,-3.39132814704771,40.6484059320886));
#31480=CARTESIAN_POINT('Ctrl Pts',(3.41850245671627,-3.53708928199259,40.6368366085084));
#31481=CARTESIAN_POINT('Ctrl Pts',(3.35370985647061,-3.59858160481833,40.6318080748863));
#31482=CARTESIAN_POINT('Ctrl Pts',(3.23725330713151,-3.70322797967979,40.6229638174593));
#31483=CARTESIAN_POINT('Ctrl Pts',(3.18631069491693,-3.74714964550685,40.6191562630126));
#31484=CARTESIAN_POINT('Ctrl Pts',(3.063085191658,-3.84906180221732,40.6100813325401));
#31485=CARTESIAN_POINT('Ctrl Pts',(2.99003293003017,-3.90608120891154,40.6048072677707));
#31486=CARTESIAN_POINT('Ctrl Pts',(2.86339029042916,-3.99929391888486,40.5958329208454));
#31487=CARTESIAN_POINT('Ctrl Pts',(2.81061698608563,-4.03655644016261,40.5921406362612));
#31488=CARTESIAN_POINT('Ctrl Pts',(2.64304214184509,-4.14999889126037,40.5805631747692));
#31489=CARTESIAN_POINT('Ctrl Pts',(2.52576417070549,-4.22240193500484,40.5726694856033));
#31490=CARTESIAN_POINT('Ctrl Pts',(2.35307115826591,-4.31924372768505,40.5613666374717));
#31491=CARTESIAN_POINT('Ctrl Pts',(2.30000368458892,-4.34773428701329,40.5579352840458));
#31492=CARTESIAN_POINT('Ctrl Pts',(2.21373536687171,-4.39202791280347,40.552429001109));
#31493=CARTESIAN_POINT('Ctrl Pts',(2.18085766640212,-4.40844568303518,40.5503473066003));
#31494=CARTESIAN_POINT('Ctrl Pts',(2.09341828856982,-4.45089170928469,40.5448538701359));
#31495=CARTESIAN_POINT('Ctrl Pts',(2.03855540942028,-4.47628519111695,40.5414497905662));
#31496=CARTESIAN_POINT('Ctrl Pts',(1.82218346700338,-4.57163052739899,40.5281607523585));
#31497=CARTESIAN_POINT('Ctrl Pts',(1.6574350816683,-4.63390416202332,40.5183307120094));
#31498=CARTESIAN_POINT('Ctrl Pts',(1.41432341579592,-4.71117060158908,40.5040183218915));
#31499=CARTESIAN_POINT('Ctrl Pts',(1.33837699845439,-4.73330603453515,40.4995744753822));
#31500=CARTESIAN_POINT('Ctrl Pts',(1.19169855837149,-4.77224451623979,40.4910257248124));
#31501=CARTESIAN_POINT('Ctrl Pts',(1.12106277791577,-4.78932993890191,40.48692372207));
#31502=CARTESIAN_POINT('Ctrl Pts',(0.988809572068376,-4.81823322542175,
40.4792610537538));
#31503=CARTESIAN_POINT('Ctrl Pts',(0.927294127842371,-4.830449386652,40.4757039259542));
#31504=CARTESIAN_POINT('Ctrl Pts',(0.744683672134529,-4.86309654144218,
40.4651587298516));
#31505=CARTESIAN_POINT('Ctrl Pts',(0.623039361243161,-4.88017244297477,
40.4581515322236));
#31506=CARTESIAN_POINT('Ctrl Pts',(0.347257412911509,-4.90840546064777,
40.4422951712435));
#31507=CARTESIAN_POINT('Ctrl Pts',(0.192973982276927,-4.91688856340486,
40.4334441485654));
#31508=CARTESIAN_POINT('Ctrl Pts',(0.0114908346716353,-4.91831100326869,
40.423088420495));
#31509=CARTESIAN_POINT('Ctrl Pts',(-0.0155670981207993,-4.91829979159156,
40.4215459996912));
#31510=CARTESIAN_POINT('Ctrl Pts',(-0.0854693359728234,-4.91769396625693,
40.4175659650834));
#31511=CARTESIAN_POINT('Ctrl Pts',(-0.128308678464229,-4.9167627452191,
40.4151313662233));
#31512=CARTESIAN_POINT('Ctrl Pts',(-0.21209805116757,-4.91384552448128,
40.410380877063));
#31513=CARTESIAN_POINT('Ctrl Pts',(-0.253046257479163,-4.91190706934958,
40.4080647256208));
#31514=CARTESIAN_POINT('Ctrl Pts',(-0.441802045227604,-4.90060485653567,
40.3974019782434));
#31515=CARTESIAN_POINT('Ctrl Pts',(-0.589164823893292,-4.8850796126689,
40.3891145210953));
#31516=CARTESIAN_POINT('Ctrl Pts',(-0.881335476444615,-4.84088366236685,
40.3725600806903));
#31517=CARTESIAN_POINT('Ctrl Pts',(-1.02600154734095,-4.81229955324352,
40.3643014367101));
#31518=CARTESIAN_POINT('Ctrl Pts',(-1.23949923693228,-4.76004916349649,
40.3519191590435));
#31519=CARTESIAN_POINT('Ctrl Pts',(-1.30944507470617,-4.74128461852585,
40.3478312085033));
#31520=CARTESIAN_POINT('Ctrl Pts',(-1.43928653541154,-4.70335926244195,
40.3401742294546));
#31521=CARTESIAN_POINT('Ctrl Pts',(-1.49927869188953,-4.6845808113581,40.3366086255711));
#31522=CARTESIAN_POINT('Ctrl Pts',(-1.68223966891118,-4.62343661130429,
40.3256420127992));
#31523=CARTESIAN_POINT('Ctrl Pts',(-1.80390042499715,-4.57733972253791,
40.3182186702065));
#31524=CARTESIAN_POINT('Ctrl Pts',(-2.03670624979136,-4.47840561511,40.3037471662076));
#31525=CARTESIAN_POINT('Ctrl Pts',(-2.14798127852132,-4.4261118041256,40.2967060105874));
#31526=CARTESIAN_POINT('Ctrl Pts',(-2.3198982158494,-4.33730773823601,40.2856495087172));
#31527=CARTESIAN_POINT('Ctrl Pts',(-2.38191182290566,-4.30356391780155,
40.28162349304));
#31528=CARTESIAN_POINT('Ctrl Pts',(-2.47538609803914,-4.25006163907513,
40.2755040224618));
#31529=CARTESIAN_POINT('Ctrl Pts',(-2.50738462099791,-4.23126254031497,
40.2734000766671));
#31530=CARTESIAN_POINT('Ctrl Pts',(-2.58375524397054,-4.18522429557003,
40.2683567975792));
#31531=CARTESIAN_POINT('Ctrl Pts',(-2.62791354361724,-4.15763924155213,
40.2654219260389));
#31532=CARTESIAN_POINT('Ctrl Pts',(-2.80866745312201,-4.04069447324324,
40.2533099295796));
#31533=CARTESIAN_POINT('Ctrl Pts',(-2.94121125220358,-3.94526321342507,
40.244188384022));
#31534=CARTESIAN_POINT('Ctrl Pts',(-3.13841208648988,-3.78780883130564,
40.2300419995351));
#31535=CARTESIAN_POINT('Ctrl Pts',(-3.20653417846862,-3.73031694925138,
40.2250406554286));
#31536=CARTESIAN_POINT('Ctrl Pts',(-3.33088507147023,-3.61944613791084,
40.2156651433138));
#31537=CARTESIAN_POINT('Ctrl Pts',(-3.38748718848314,-3.56652717127812,
40.2112958065381));
#31538=CARTESIAN_POINT('Ctrl Pts',(-3.49133606069609,-3.46473258874863,
40.2030712723929));
#31539=CARTESIAN_POINT('Ctrl Pts',(-3.5388658321118,-3.41617152450963,40.1992198807745));
#31540=CARTESIAN_POINT('Ctrl Pts',(-3.66769395098982,-3.27897338735749,
40.1885260062558));
#31541=CARTESIAN_POINT('Ctrl Pts',(-3.74676990167051,-3.18831618374307,
40.1816666469326));
#31542=CARTESIAN_POINT('Ctrl Pts',(-3.90763839537789,-2.9896280456453,40.1670484457888));
#31543=CARTESIAN_POINT('Ctrl Pts',(-3.98845277301097,-2.88093008319467,
40.1592908320748));
#31544=CARTESIAN_POINT('Ctrl Pts',(-4.09485606079001,-2.72474030229458,
40.1484894546837));
#31545=CARTESIAN_POINT('Ctrl Pts',(-4.12430681336699,-2.67995321797789,
40.1454301402173));
#31546=CARTESIAN_POINT('Ctrl Pts',(-4.17631587965217,-2.59797226531116,
40.1399017194316));
#31547=CARTESIAN_POINT('Ctrl Pts',(-4.19912409790724,-2.56094339783189,
40.1374303969522));
#31548=CARTESIAN_POINT('Ctrl Pts',(-4.24221522708388,-2.48886171012647,
40.1326714156966));
#31549=CARTESIAN_POINT('Ctrl Pts',(-4.26256219317296,-2.45385130643173,
40.1303832079428));
#31550=CARTESIAN_POINT('Ctrl Pts',(-4.34292643774065,-2.31155461747833,
40.1211667494932));
#31551=CARTESIAN_POINT('Ctrl Pts',(-4.39934459991836,-2.20228575645318,
40.114278357886));
#31552=CARTESIAN_POINT('Ctrl Pts',(-4.49040945495615,-2.00841587798372,
40.1022778635949));
#31553=CARTESIAN_POINT('Ctrl Pts',(-4.52690234577645,-1.92475102358778,
40.0971679709301));
#31554=CARTESIAN_POINT('Ctrl Pts',(-4.59096954896794,-1.76594967120052,
40.0875613691223));
#31555=CARTESIAN_POINT('Ctrl Pts',(-4.61907900418149,-1.69106139324119,
40.0830684497223));
#31556=CARTESIAN_POINT('Ctrl Pts',(-4.66935764089449,-1.54648773988445,
40.074446902422));
#31557=CARTESIAN_POINT('Ctrl Pts',(-4.69182361231053,-1.47692793855491,
40.0703213378629));
#31558=CARTESIAN_POINT('Ctrl Pts',(-4.73060568485256,-1.34701801958561,
40.06264798708));
#31559=CARTESIAN_POINT('Ctrl Pts',(-4.74733761229574,-1.28680735883147,
40.0591039239372));
#31560=CARTESIAN_POINT('Ctrl Pts',(-4.79278337010759,-1.11029643957127,
40.0487438184267));
#31561=CARTESIAN_POINT('Ctrl Pts',(-4.81840120607102,-0.993247122121397,
40.0419098369365));
#31562=CARTESIAN_POINT('Ctrl Pts',(-4.86322047056684,-0.745454737457813,
40.0275087980453));
#31563=CARTESIAN_POINT('Ctrl Pts',(-4.88147926804105,-0.614635079622523,
40.019943777298));
#31564=CARTESIAN_POINT('Ctrl Pts',(-4.90162769916389,-0.410563376290089,
40.0082243532188));
#31565=CARTESIAN_POINT('Ctrl Pts',(-4.90718363383326,-0.337735641736515,
40.0040583875519));
#31566=CARTESIAN_POINT('Ctrl Pts',(-4.91312187312776,-0.227606454765455,
39.9977912084183));
#31567=CARTESIAN_POINT('Ctrl Pts',(-4.9147051369929,-0.190380433108299,
39.9956785946174));
#31568=CARTESIAN_POINT('Ctrl Pts',(-4.91745419764362,-0.102134038920577,
39.9906847619314));
#31569=CARTESIAN_POINT('Ctrl Pts',(-4.91824921726208,-0.0511064683498441,
39.9878076141425));
#31570=CARTESIAN_POINT('Ctrl Pts',(-4.91825229998802,0.150019757647768,
39.9764904476838));
#31571=CARTESIAN_POINT('Ctrl Pts',(-4.91138369861575,0.300037440534878,
39.9680977432507));
#31572=CARTESIAN_POINT('Ctrl Pts',(-4.88625459014518,0.573835310482956,
39.9526896390735));
#31573=CARTESIAN_POINT('Ctrl Pts',(-4.87011380743797,0.697683223990364,
39.9456861149759));
#31574=CARTESIAN_POINT('Ctrl Pts',(-4.83731210447299,0.891479717866304,
39.9346113163893));
#31575=CARTESIAN_POINT('Ctrl Pts',(-4.82380129474772,0.961907166196714,
39.9305625354046));
#31576=CARTESIAN_POINT('Ctrl Pts',(-4.79510592311643,1.0956157219789,39.9228201984772));
#31577=CARTESIAN_POINT('Ctrl Pts',(-4.78019591494569,1.15893974681738,39.9191293614024));
#31578=CARTESIAN_POINT('Ctrl Pts',(-4.76403458699542,1.22194824620825,39.9154303604093));
#31579=CARTESIAN_POINT('',(-4.91848456985419,0.000101914598987455,39.6398594359908));
#31580=CARTESIAN_POINT('Ctrl Pts',(-4.76374161084644,1.22187275725133,39.5699226582762));
#31581=CARTESIAN_POINT('Ctrl Pts',(-4.83821031443323,0.932375049404611,
39.58684801254));
#31582=CARTESIAN_POINT('Ctrl Pts',(-4.90472206789031,0.524434703871696,
39.6101602717781));
#31583=CARTESIAN_POINT('Ctrl Pts',(-4.91858862069526,0.112866935379977,
39.6334725310163));
#31584=CARTESIAN_POINT('Ctrl Pts',(-4.91848456985419,0.000101914598987455,
39.6398594359908));
#31585=CARTESIAN_POINT('Ctrl Pts',(-4.91824999878197,0.000109458262579736,
39.6399944356597));
#31586=CARTESIAN_POINT('Ctrl Pts',(-4.91825380405249,-0.170871437005476,
39.6495859678532));
#31587=CARTESIAN_POINT('Ctrl Pts',(-4.90934150834709,-0.341736064180338,
39.6591402713725));
#31588=CARTESIAN_POINT('Ctrl Pts',(-4.88416414869687,-0.582374933733232,
39.6727317641722));
#31589=CARTESIAN_POINT('Ctrl Pts',(-4.87525199054741,-0.652792382767571,
39.6767249503495));
#31590=CARTESIAN_POINT('Ctrl Pts',(-4.85531216028108,-0.78696218483098,
39.6843757529689));
#31591=CARTESIAN_POINT('Ctrl Pts',(-4.84454433577162,-0.850738335762799,
39.688030934994));
#31592=CARTESIAN_POINT('Ctrl Pts',(-4.81831674870789,-0.989366502816203,
39.6960238846444));
#31593=CARTESIAN_POINT('Ctrl Pts',(-4.80236362562827,-1.06410797581266,
39.7003640493471));
#31594=CARTESIAN_POINT('Ctrl Pts',(-4.72062103491384,-1.40765657936257,
39.720471850089));
#31595=CARTESIAN_POINT('Ctrl Pts',(-4.63396087787739,-1.67097701880662,
39.7363671056722));
#31596=CARTESIAN_POINT('Ctrl Pts',(-4.50888362915507,-1.96493725022399,
39.7545587172262));
#31597=CARTESIAN_POINT('Ctrl Pts',(-4.49163686654724,-2.00404797674673,
39.7569878356097));
#31598=CARTESIAN_POINT('Ctrl Pts',(-4.45720878502796,-2.07944324109466,
39.7616852607083));
#31599=CARTESIAN_POINT('Ctrl Pts',(-4.44008879425048,-2.11575184783079,
39.7639539235128));
#31600=CARTESIAN_POINT('Ctrl Pts',(-4.34996130050543,-2.30098395932659,
39.7755727541387));
#31601=CARTESIAN_POINT('Ctrl Pts',(-4.26989828670354,-2.4463565675653,39.7848457459926));
#31602=CARTESIAN_POINT('Ctrl Pts',(-4.129598375601,-2.67315675435193,39.799788144739));
#31603=CARTESIAN_POINT('Ctrl Pts',(-4.07392928326103,-2.75725402415036,
39.8054405691831));
#31604=CARTESIAN_POINT('Ctrl Pts',(-3.96871867005731,-2.90604215939763,
39.8156874692169));
#31605=CARTESIAN_POINT('Ctrl Pts',(-3.92007997359551,-2.97132658977595,
39.8202741984091));
#31606=CARTESIAN_POINT('Ctrl Pts',(-3.86502005635664,-3.04152332213673,
39.8253164067597));
#31607=CARTESIAN_POINT('Ctrl Pts',(-3.86018153268147,-3.04766183978437,
39.8257582784446));
#31608=CARTESIAN_POINT('Ctrl Pts',(-3.84697764023086,-3.064331408321,39.8269608007248));
#31609=CARTESIAN_POINT('Ctrl Pts',(-3.83858368339721,-3.07483971109781,
39.8277216799806));
#31610=CARTESIAN_POINT('Ctrl Pts',(-3.79048970413415,-3.13454417932209,
39.8320610348507));
#31611=CARTESIAN_POINT('Ctrl Pts',(-3.74988746088526,-3.18300539260527,
39.835646728471));
#31612=CARTESIAN_POINT('Ctrl Pts',(-3.62716353657138,-3.32387549084481,
39.8462671682976));
#31613=CARTESIAN_POINT('Ctrl Pts',(-3.54248025997216,-3.41398543796978,
39.8533213071857));
#31614=CARTESIAN_POINT('Ctrl Pts',(-3.37474670909175,-3.57949991103548,
39.8668000842906));
#31615=CARTESIAN_POINT('Ctrl Pts',(-3.29233455531089,-3.65544362948992,
39.8732176907365));
#31616=CARTESIAN_POINT('Ctrl Pts',(-3.16181580181251,-3.76772075223153,
39.8830634686469));
#31617=CARTESIAN_POINT('Ctrl Pts',(-3.11551492340916,-3.80609585759247,
39.8864981807686));
#31618=CARTESIAN_POINT('Ctrl Pts',(-3.03219316867195,-3.87261521154067,
39.8925732721704));
#31619=CARTESIAN_POINT('Ctrl Pts',(-2.99545488666384,-3.90110164939895,
39.8952167120479));
#31620=CARTESIAN_POINT('Ctrl Pts',(-2.92735731573845,-3.95237450034852,
39.9000499073559));
#31621=CARTESIAN_POINT('Ctrl Pts',(-2.89612222976877,-3.97531899386409,
39.9022414377925));
#31622=CARTESIAN_POINT('Ctrl Pts',(-2.80255975533688,-4.04235952871821,
39.9087368107064));
#31623=CARTESIAN_POINT('Ctrl Pts',(-2.73947306651016,-4.08537627094839,
39.9130272283708));
#31624=CARTESIAN_POINT('Ctrl Pts',(-2.54493574657071,-4.21149180140599,
39.9260352763269));
#31625=CARTESIAN_POINT('Ctrl Pts',(-2.41052357468821,-4.28984117615114,
39.9347265769696));
#31626=CARTESIAN_POINT('Ctrl Pts',(-2.20472033538892,-4.39707338898737,
39.9477511439824));
#31627=CARTESIAN_POINT('Ctrl Pts',(-2.13599790362256,-4.43086435736537,
39.9520549745192));
#31628=CARTESIAN_POINT('Ctrl Pts',(-2.00570345418328,-4.4911944533872,39.9601463359329));
#31629=CARTESIAN_POINT('Ctrl Pts',(-1.94432313575945,-4.51810595055532,
39.9639303844588));
#31630=CARTESIAN_POINT('Ctrl Pts',(-1.83193200935231,-4.5646679868378,39.9708167495842));
#31631=CARTESIAN_POINT('Ctrl Pts',(-1.78110676819378,-4.58473852314179,
39.9739154421669));
#31632=CARTESIAN_POINT('Ctrl Pts',(-1.61818168800316,-4.64595835812933,
39.983804487152));
#31633=CARTESIAN_POINT('Ctrl Pts',(-1.50491416145742,-4.68387380341578,
39.9906147339127));
#31634=CARTESIAN_POINT('Ctrl Pts',(-1.25906589890843,-4.75633024829885,
40.005269774266));
#31635=CARTESIAN_POINT('Ctrl Pts',(-1.12619279710575,-4.78953172313279,
40.0131140799779));
#31636=CARTESIAN_POINT('Ctrl Pts',(-0.939228885663524,-4.82803759207858,
40.0240243409718));
#31637=CARTESIAN_POINT('Ctrl Pts',(-0.88617351712668,-4.83805688855832,
40.0271060380122));
#31638=CARTESIAN_POINT('Ctrl Pts',(-0.794217816583256,-4.85385894891157,
40.0324190957173));
#31639=CARTESIAN_POINT('Ctrl Pts',(-0.755393247203296,-4.86005244012726,
40.0346536961606));
#31640=CARTESIAN_POINT('Ctrl Pts',(-0.687365714579173,-4.87006966581824,
40.0385524034825));
#31641=CARTESIAN_POINT('Ctrl Pts',(-0.658195217830814,-4.87409778761951,
40.0402186475269));
#31642=CARTESIAN_POINT('Ctrl Pts',(-0.560804454528446,-4.88665611686589,
40.0457657363222));
#31643=CARTESIAN_POINT('Ctrl Pts',(-0.492441355987468,-4.89401791274671,
40.049633815286));
#31644=CARTESIAN_POINT('Ctrl Pts',(-0.25742644258563,-4.91435153091155,
40.0628808816306));
#31645=CARTESIAN_POINT('Ctrl Pts',(-0.0902805606894244,-4.92026107802224,
40.072219110002));
#31646=CARTESIAN_POINT('Ctrl Pts',(0.181084879859672,-4.9160208166942,40.0874481640124));
#31647=CARTESIAN_POINT('Ctrl Pts',(0.285249127677867,-4.9110777795041,40.0933093068804));
#31648=CARTESIAN_POINT('Ctrl Pts',(0.433520850873622,-4.89930827197351,
40.1017032653211));
#31649=CARTESIAN_POINT('Ctrl Pts',(0.477815160072979,-4.89518687147136,
40.104217272108));
#31650=CARTESIAN_POINT('Ctrl Pts',(0.53113761744237,-4.88949480727931,40.1072527800906));
#31651=CARTESIAN_POINT('Ctrl Pts',(0.540225261002683,-4.88849908521108,
40.1077704339065));
#31652=CARTESIAN_POINT('Ctrl Pts',(0.624104688839324,-4.87907176630438,
40.1125514192457));
#31653=CARTESIAN_POINT('Ctrl Pts',(0.698695851383743,-4.86894977252967,
40.1168253081762));
#31654=CARTESIAN_POINT('Ctrl Pts',(0.882107812899771,-4.83975922914403,
40.1273977247081));
#31655=CARTESIAN_POINT('Ctrl Pts',(0.990574165129971,-4.81872867058308,
40.1337060305085));
#31656=CARTESIAN_POINT('Ctrl Pts',(1.21703565956611,-4.766850159978,40.1469982071036));
#31657=CARTESIAN_POINT('Ctrl Pts',(1.33477950833735,-4.73522966597282,40.1539801603826));
#31658=CARTESIAN_POINT('Ctrl Pts',(1.50044562213065,-4.68406868950492,40.1638872846454));
#31659=CARTESIAN_POINT('Ctrl Pts',(1.54942259776311,-4.6680966388798,40.1668266074534));
#31660=CARTESIAN_POINT('Ctrl Pts',(1.63829550845636,-4.63756118208562,40.1721761248854));
#31661=CARTESIAN_POINT('Ctrl Pts',(1.6782710987365,-4.62324475510122,40.1745883022877));
#31662=CARTESIAN_POINT('Ctrl Pts',(1.75763041877068,-4.59365890410072,40.1793864014169));
#31663=CARTESIAN_POINT('Ctrl Pts',(1.79701288812756,-4.57839617672405,40.1817721764296));
#31664=CARTESIAN_POINT('Ctrl Pts',(1.97952007660285,-4.50494757728266,40.1928628089835));
#31665=CARTESIAN_POINT('Ctrl Pts',(2.12005011548457,-4.44054512171268,40.2015044643823));
#31666=CARTESIAN_POINT('Ctrl Pts',(2.38290784497685,-4.30475501852256,40.2180801838806));
#31667=CARTESIAN_POINT('Ctrl Pts',(2.50564239405402,-4.23449183527942,40.226003933801));
#31668=CARTESIAN_POINT('Ctrl Pts',(2.68634879532864,-4.12043028504605,40.2380441945136));
#31669=CARTESIAN_POINT('Ctrl Pts',(2.74665899280869,-4.08047543812533,40.2421286570757));
#31670=CARTESIAN_POINT('Ctrl Pts',(2.85863465239956,-4.00268512649904,40.2498480334147));
#31671=CARTESIAN_POINT('Ctrl Pts',(2.91048543662297,-3.96514245728844,40.2534798163193));
#31672=CARTESIAN_POINT('Ctrl Pts',(3.11636713309874,-3.80985874636241,40.2681434893905));
#31673=CARTESIAN_POINT('Ctrl Pts',(3.26410627944244,-3.68407058501565,40.2792351899149));
#31674=CARTESIAN_POINT('Ctrl Pts',(3.46150416980243,-3.49478354881989,40.2948894113038));
#31675=CARTESIAN_POINT('Ctrl Pts',(3.51762923628789,-3.43828559777132,40.2994444483396));
#31676=CARTESIAN_POINT('Ctrl Pts',(3.59090501574226,-3.36084994769392,40.3055273431877));
#31677=CARTESIAN_POINT('Ctrl Pts',(3.60929037297623,-3.34109775626211,40.3070655141585));
#31678=CARTESIAN_POINT('Ctrl Pts',(3.65646417692722,-3.28957306578256,40.311042680713));
#31679=CARTESIAN_POINT('Ctrl Pts',(3.6850015495682,-3.2575734633346,40.3134786234767));
#31680=CARTESIAN_POINT('Ctrl Pts',(3.7405574267787,-3.19361303210002,40.3182785178885));
#31681=CARTESIAN_POINT('Ctrl Pts',(3.76759368551343,-3.16167233171011,40.3206425219592));
#31682=CARTESIAN_POINT('Ctrl Pts',(3.88168774424247,-3.02333935585963,40.3307522163886));
#31683=CARTESIAN_POINT('Ctrl Pts',(3.96467250334307,-2.91366665555636,40.3384483356752));
#31684=CARTESIAN_POINT('Ctrl Pts',(4.13446596625642,-2.66855763522293,40.3551522609846));
#31685=CARTESIAN_POINT('Ctrl Pts',(4.21944680064033,-2.53204986832389,40.3641530158703));
#31686=CARTESIAN_POINT('Ctrl Pts',(4.33262594742223,-2.32867473918436,40.3772678647632));
#31687=CARTESIAN_POINT('Ctrl Pts',(4.36627225693209,-2.26495917423766,40.3813362550234));
#31688=CARTESIAN_POINT('Ctrl Pts',(4.43130602307156,-2.13496699029808,40.3895661997115));
#31689=CARTESIAN_POINT('Ctrl Pts',(4.46263535629884,-2.06868137368618,40.3937271117874));
#31690=CARTESIAN_POINT('Ctrl Pts',(4.55383461287824,-1.86400246975567,40.4064772546395));
#31691=CARTESIAN_POINT('Ctrl Pts',(4.6088322883087,-1.723536731297,40.4150953682651));
#31692=CARTESIAN_POINT('Ctrl Pts',(4.68929700832626,-1.48647008250853,40.4294262331924));
#31693=CARTESIAN_POINT('Ctrl Pts',(4.71843245351833,-1.3912207082221,40.4351280122482));
#31694=CARTESIAN_POINT('Ctrl Pts',(4.76137847641793,-1.23389241068017,40.4444409781371));
#31695=CARTESIAN_POINT('Ctrl Pts',(4.77691281317847,-1.17231377775277,40.4480601166233));
#31696=CARTESIAN_POINT('Ctrl Pts',(4.79963651653507,-1.07426808123617,40.4537758792679));
#31697=CARTESIAN_POINT('Ctrl Pts',(4.80761241121767,-1.03799111234175,40.4558803574403));
#31698=CARTESIAN_POINT('Ctrl Pts',(4.82723479497463,-0.943659324131473,
40.4613267756976));
#31699=CARTESIAN_POINT('Ctrl Pts',(4.83824523540743,-0.885478318761359,
40.464661615081));
#31700=CARTESIAN_POINT('Ctrl Pts',(4.87814730463323,-0.651588277276984,
40.4779990118264));
#31701=CARTESIAN_POINT('Ctrl Pts',(4.89853807301753,-0.474566944708308,
40.4879433117897));
#31702=CARTESIAN_POINT('Ctrl Pts',(4.91409360002124,-0.217293229452264,
40.5024037716249));
#31703=CARTESIAN_POINT('Ctrl Pts',(4.91696898605229,-0.137652057999693,
40.5068804031427));
#31704=CARTESIAN_POINT('Ctrl Pts',(4.91877154398843,0.0152508559710218,
40.5154940979235));
#31705=CARTESIAN_POINT('Ctrl Pts',(4.91799916601728,0.0884880131010949,
40.5196282124979));
#31706=CARTESIAN_POINT('Ctrl Pts',(4.91350680327257,0.225070280268358,40.5273636706882));
#31707=CARTESIAN_POINT('Ctrl Pts',(4.91019582971013,0.288413833167033,40.5309614627255));
#31708=CARTESIAN_POINT('Ctrl Pts',(4.89615185819561,0.484318938605563,40.5421273142273));
#31709=CARTESIAN_POINT('Ctrl Pts',(4.88126714874111,0.616520971278551,40.5497189623331));
#31710=CARTESIAN_POINT('Ctrl Pts',(4.84266064773769,0.86742879772177,40.5642435882752));
#31711=CARTESIAN_POINT('Ctrl Pts',(4.8198792788169,0.986183903647256,40.5711684564434));
#31712=CARTESIAN_POINT('Ctrl Pts',(4.78122261590757,1.15400554892581,40.5810085312252));
#31713=CARTESIAN_POINT('Ctrl Pts',(4.76891667289989,1.20384896883195,40.5839377705937));
#31714=CARTESIAN_POINT('Ctrl Pts',(4.74503533034857,1.294456464318,40.5892717663854));
#31715=CARTESIAN_POINT('Ctrl Pts',(4.73370912296363,1.33528117599438,40.5916784867908));
#31716=CARTESIAN_POINT('Ctrl Pts',(4.71001478470901,1.41659291396916,40.5964764237059));
#31717=CARTESIAN_POINT('Ctrl Pts',(4.69764855134786,1.45707683399495,40.598867447045));
#31718=CARTESIAN_POINT('Ctrl Pts',(4.64565269589739,1.61975130641064,40.6084949389549));
#31719=CARTESIAN_POINT('Ctrl Pts',(4.6017653778865,1.7405284755397,40.6156892851189));
#31720=CARTESIAN_POINT('Ctrl Pts',(4.49289156162443,2.00712573965965,40.6318219193209));
#31721=CARTESIAN_POINT('Ctrl Pts',(4.42543504490809,2.15177885685023,40.6407530513677));
#31722=CARTESIAN_POINT('Ctrl Pts',(4.31646630008613,2.35856119924585,40.6539164922645));
#31723=CARTESIAN_POINT('Ctrl Pts',(4.28038124290289,2.42343320415657,40.6581055718187));
#31724=CARTESIAN_POINT('Ctrl Pts',(4.20676162634252,2.54900548150244,40.6663435008808));
#31725=CARTESIAN_POINT('Ctrl Pts',(4.16934661066024,2.60975497074282,40.6703904849311));
#31726=CARTESIAN_POINT('Ctrl Pts',(4.06911924840025,2.76483096808158,40.6808910946124));
#31727=CARTESIAN_POINT('Ctrl Pts',(4.00434517016673,2.85783852081929,40.6873573124425));
#31728=CARTESIAN_POINT('Ctrl Pts',(3.85766946311584,3.05365739186701,40.7013500266205));
#31729=CARTESIAN_POINT('Ctrl Pts',(3.77474120876909,3.15559280988947,40.7088761983449));
#31730=CARTESIAN_POINT('Ctrl Pts',(3.63952518434315,3.3088321486454,40.7205557069877));
#31731=CARTESIAN_POINT('Ctrl Pts',(3.59000463550267,3.36249619568968,40.7247205706407));
#31732=CARTESIAN_POINT('Ctrl Pts',(3.51323041248651,3.44206413862823,40.7310033986718));
#31733=CARTESIAN_POINT('Ctrl Pts',(3.48684462088458,3.46879058325829,40.7331327157336));
#31734=CARTESIAN_POINT('Ctrl Pts',(3.42301168752941,3.53198326123077,40.7382128296772));
#31735=CARTESIAN_POINT('Ctrl Pts',(3.38528431836948,3.56815988240232,40.7411592013476));
#31736=CARTESIAN_POINT('Ctrl Pts',(3.22714317723627,3.71503453358388,40.7533015844116));
#31737=CARTESIAN_POINT('Ctrl Pts',(3.10182062141677,3.82029374217735,40.7624416666057));
#31738=CARTESIAN_POINT('Ctrl Pts',(2.90022211939522,3.97314646910845,40.7766239956036));
#31739=CARTESIAN_POINT('Ctrl Pts',(2.82749778510871,4.02522512314026,40.7816425990572));
#31740=CARTESIAN_POINT('Ctrl Pts',(2.68885704562708,4.11889514288085,40.7910586284024));
#31741=CARTESIAN_POINT('Ctrl Pts',(2.62329348441445,4.16095908560212,40.7954512086737));
#31742=CARTESIAN_POINT('Ctrl Pts',(2.4980419819297,4.23717993590698,40.8037440839669));
#31743=CARTESIAN_POINT('Ctrl Pts',(2.43858257343126,4.27167677179018,40.8076406321834));
#31744=CARTESIAN_POINT('Ctrl Pts',(2.26891637771215,4.36541553953362,40.8186559488885));
#31745=CARTESIAN_POINT('Ctrl Pts',(2.15714528485309,4.42171436295713,40.8257934924014));
#31746=CARTESIAN_POINT('Ctrl Pts',(1.87424050601356,4.55093067861764,40.8435816087837));
#31747=CARTESIAN_POINT('Ctrl Pts',(1.70088588605657,4.61852090806383,40.8542427797494));
#31748=CARTESIAN_POINT('Ctrl Pts',(1.48368011510898,4.68931611296052,40.8672479811749));
#31749=CARTESIAN_POINT('Ctrl Pts',(1.44306938097336,4.70197225735915,40.8696644799418));
#31750=CARTESIAN_POINT('Ctrl Pts',(1.36755566561905,4.72443525714269,40.8741277826841));
#31751=CARTESIAN_POINT('Ctrl Pts',(1.33269860848281,4.73438606911129,40.8761762732633));
#31752=CARTESIAN_POINT('Ctrl Pts',(1.13905398316217,4.78735865039544,40.8875008827966));
#31753=CARTESIAN_POINT('Ctrl Pts',(0.978293493822922,4.82277824465111,40.8966997066159));
#31754=CARTESIAN_POINT('Ctrl Pts',(0.715559786213942,4.86698503455403,40.9116270542556));
#31755=CARTESIAN_POINT('Ctrl Pts',(0.614559663888879,4.88076687964144,40.9173396501757));
#31756=CARTESIAN_POINT('Ctrl Pts',(0.474073919237509,4.89550662134189,40.925282170632));
#31757=CARTESIAN_POINT('Ctrl Pts',(0.434895122296926,4.89914251381362,40.9274967489058));
#31758=CARTESIAN_POINT('Ctrl Pts',(0.324400570819698,4.90806079493912,40.9337441490601));
#31759=CARTESIAN_POINT('Ctrl Pts',(0.253007662664536,4.91225848914196,40.9377828339007));
#31760=CARTESIAN_POINT('Ctrl Pts',(0.107612537255581,4.91762917406558,40.9460219374882));
#31761=CARTESIAN_POINT('Ctrl Pts',(0.0336242836440473,4.91869153173761,
40.9502220685086));
#31762=CARTESIAN_POINT('Ctrl Pts',(-0.20218934826509,4.91675638125509,40.963642690932));
#31763=CARTESIAN_POINT('Ctrl Pts',(-0.363853708336036,4.90744161532399,
40.9728977025432));
#31764=CARTESIAN_POINT('Ctrl Pts',(-0.615182301461178,4.8804716733818,40.9873678651629));
#31765=CARTESIAN_POINT('Ctrl Pts',(-0.705316357912556,4.8682627283663,40.9925730679019));
#31766=CARTESIAN_POINT('Ctrl Pts',(-0.854659235233268,4.84379892228501,
41.0012122650179));
#31767=CARTESIAN_POINT('Ctrl Pts',(-0.914073810919858,4.83293902321936,
41.0046531009655));
#31768=CARTESIAN_POINT('Ctrl Pts',(-1.00966294806102,4.81364123458574,41.0101900135744));
#31769=CARTESIAN_POINT('Ctrl Pts',(-1.04596781231514,4.8058831217296,41.0122928324722));
#31770=CARTESIAN_POINT('Ctrl Pts',(-1.14281285486558,4.78403856520235,41.0179034113745));
#31771=CARTESIAN_POINT('Ctrl Pts',(-1.20317972634694,4.76921428551848,41.0214029176017));
#31772=CARTESIAN_POINT('Ctrl Pts',(-1.43190349461411,4.70842739372774,41.0347018143988));
#31773=CARTESIAN_POINT('Ctrl Pts',(-1.59805257712061,4.65466052639345,41.0444489906849));
#31774=CARTESIAN_POINT('Ctrl Pts',(-1.83496484749956,4.56381021311958,41.0586852454443));
#31775=CARTESIAN_POINT('Ctrl Pts',(-1.90824057283842,4.53366048709048,41.0631364932948));
#31776=CARTESIAN_POINT('Ctrl Pts',(-2.0475872034986,4.47234847398694,41.0717126478637));
#31777=CARTESIAN_POINT('Ctrl Pts',(-2.11375521471139,4.44145842680702,41.0758346904216));
#31778=CARTESIAN_POINT('Ctrl Pts',(-2.236185689482,4.38094690606733,41.0835655307352));
#31779=CARTESIAN_POINT('Ctrl Pts',(-2.29260931302714,4.35168526633352,41.087170876352));
#31780=CARTESIAN_POINT('Ctrl Pts',(-2.5206479958865,4.22775668742044,41.1019264655134));
#31781=CARTESIAN_POINT('Ctrl Pts',(-2.68709676478735,4.12396676932475,41.1131385912332));
#31782=CARTESIAN_POINT('Ctrl Pts',(-2.91209416945621,3.96425043423538,41.1289322758749));
#31783=CARTESIAN_POINT('Ctrl Pts',(-2.97614513104901,3.91639301420836,41.133505603347));
#31784=CARTESIAN_POINT('Ctrl Pts',(-3.06027010316607,3.85028073015547,41.1396105635951));
#31785=CARTESIAN_POINT('Ctrl Pts',(-3.08140068626419,3.83339074794697,41.1411525607872));
#31786=CARTESIAN_POINT('Ctrl Pts',(-3.13571229212046,3.78923944164817,41.1451374956286));
#31787=CARTESIAN_POINT('Ctrl Pts',(-3.16867773142135,3.76171617972036,41.1475773785419));
#31788=CARTESIAN_POINT('Ctrl Pts',(-3.23299913147575,3.70656788949798,41.1523777342265));
#31789=CARTESIAN_POINT('Ctrl Pts',(-3.26437189973619,3.67896793319757,41.1547382919601));
#31790=CARTESIAN_POINT('Ctrl Pts',(-3.37622277209184,3.5780106432003,41.1632334742143));
#31791=CARTESIAN_POINT('Ctrl Pts',(-3.45461167480752,3.50238476311132,41.1693387667494));
#31792=CARTESIAN_POINT('Ctrl Pts',(-3.64228781453872,3.30888754907747,41.1844435796004));
#31793=CARTESIAN_POINT('Ctrl Pts',(-3.74843005721304,3.18814506200019,41.1934318874686));
#31794=CARTESIAN_POINT('Ctrl Pts',(-3.89858136444738,2.99945375229901,41.2069967199575));
#31795=CARTESIAN_POINT('Ctrl Pts',(-3.94713751378956,2.93526228913609,41.2115333717542));
#31796=CARTESIAN_POINT('Ctrl Pts',(-4.03425418939779,2.81402067247793,41.2199746374233));
#31797=CARTESIAN_POINT('Ctrl Pts',(-4.07323422168457,2.75729614690125,41.2238746480174));
#31798=CARTESIAN_POINT('Ctrl Pts',(-4.17376648376287,2.60421318625216,41.234278772206));
#31799=CARTESIAN_POINT('Ctrl Pts',(-4.23317050561093,2.50649554384115,41.2407971078437));
#31800=CARTESIAN_POINT('Ctrl Pts',(-4.35885218952251,2.28252029276776,41.2554782933823));
#31801=CARTESIAN_POINT('Ctrl Pts',(-4.42315497298407,2.15527058597694,41.2636443295072));
#31802=CARTESIAN_POINT('Ctrl Pts',(-4.50442402279167,1.97543776803799,41.2749245689562));
#31803=CARTESIAN_POINT('Ctrl Pts',(-4.52616950938839,1.92509215259191,41.2780549932424));
#31804=CARTESIAN_POINT('Ctrl Pts',(-4.56392768442045,1.83349503360702,41.2836972046173));
#31805=CARTESIAN_POINT('Ctrl Pts',(-4.58023430526373,1.79237097641657,41.2862113376064));
#31806=CARTESIAN_POINT('Ctrl Pts',(-4.61049448332292,1.71294622759946,41.2910280207994));
#31807=CARTESIAN_POINT('Ctrl Pts',(-4.62453099647541,1.67468124173679,41.2933312389981));
#31808=CARTESIAN_POINT('Ctrl Pts',(-4.6790932645764,1.52001944019533,41.3025805678251));
#31809=CARTESIAN_POINT('Ctrl Pts',(-4.71571331130518,1.40229152375044,41.3094865621716));
#31810=CARTESIAN_POINT('Ctrl Pts',(-4.75339206495188,1.26289128003114,41.3175768139253));
#31811=CARTESIAN_POINT('Ctrl Pts',(-4.7587794745832,1.24243646034837,41.3187617358029));
#31812=CARTESIAN_POINT('Ctrl Pts',(-4.76403458753695,1.22194824409695,41.3199466556564));
#31813=CARTESIAN_POINT('Origin',(0.,0.,-3.23514056400928));
#31814=CARTESIAN_POINT('',(-4.76403458704966,1.22194824599677,43.4152064557962));
#31815=CARTESIAN_POINT('',(-4.76403458776301,1.22194824321562,43.0699834446552));
#31816=CARTESIAN_POINT('',(-4.76403458704967,1.22194824599672,-3.23514056400928));
#31817=CARTESIAN_POINT('',(-4.91824999998163,-1.34407408516682E-5,41.7351405640093));
#31818=CARTESIAN_POINT('Ctrl Pts',(-4.91824999998163,-1.34407408516682E-5,
41.7351405640093));
#31819=CARTESIAN_POINT('Ctrl Pts',(-4.9182496007205,-0.146111492021241,
41.7434115561549));
#31820=CARTESIAN_POINT('Ctrl Pts',(-4.91173503323865,-0.292193156995082,
41.7516825483005));
#31821=CARTESIAN_POINT('Ctrl Pts',(-4.89873667140923,-0.437678062838914,
41.7599535404461));
#31822=CARTESIAN_POINT('Ctrl Pts',(-4.88573395304958,-0.583211729395645,
41.768227304697));
#31823=CARTESIAN_POINT('Ctrl Pts',(-4.86624312668477,-0.728147924347313,
41.7765010689479));
#31824=CARTESIAN_POINT('Ctrl Pts',(-4.84034647390028,-0.871911162390469,
41.7847748331988));
#31825=CARTESIAN_POINT('Ctrl Pts',(-4.82220470072196,-0.972623794160462,
41.7905709781917));
#31826=CARTESIAN_POINT('Ctrl Pts',(-4.80092026754504,-1.07276089085213,
41.7963671231846));
#31827=CARTESIAN_POINT('Ctrl Pts',(-4.77653643689978,-1.17212743738414,
41.8021632681775));
#31828=CARTESIAN_POINT('Ctrl Pts',(-4.74222309626264,-1.31195772937941,
41.8103197018576));
#31829=CARTESIAN_POINT('Ctrl Pts',(-4.70175895042439,-1.45030636416344,
41.8184761355377));
#31830=CARTESIAN_POINT('Ctrl Pts',(-4.65529696866333,-1.58662950812534,
41.8266325692178));
#31831=CARTESIAN_POINT('Ctrl Pts',(-4.6088444432254,-1.72292490648424,41.8347873428337));
#31832=CARTESIAN_POINT('Ctrl Pts',(-4.55639662503431,-1.85719531987858,
41.8429421164495));
#31833=CARTESIAN_POINT('Ctrl Pts',(-4.49815595564138,-1.98891328650295,
41.8510968900654));
#31834=CARTESIAN_POINT('Ctrl Pts',(-4.43991322085102,-2.12063592426096,
41.8592519528753));
#31835=CARTESIAN_POINT('Ctrl Pts',(-4.37587735567236,-2.24980562657217,
41.8674070156851));
#31836=CARTESIAN_POINT('Ctrl Pts',(-4.30629864695912,-2.37591561838759,
41.8755620784949));
#31837=CARTESIAN_POINT('Ctrl Pts',(-4.23672401903191,-2.50201821386147,
41.8837166630109));
#31838=CARTESIAN_POINT('Ctrl Pts',(-4.16160736044227,-2.6250611653142,41.8918712475269));
#31839=CARTESIAN_POINT('Ctrl Pts',(-4.08124452071586,-2.74456302981491,
41.9000258320429));
#31840=CARTESIAN_POINT('Ctrl Pts',(-4.00086192258999,-2.86409427562645,
41.9081824214848));
#31841=CARTESIAN_POINT('Ctrl Pts',(-3.91523075255369,-2.98008241684767,
41.9163390109267));
#31842=CARTESIAN_POINT('Ctrl Pts',(-3.82469007041437,-3.09207518145561,
41.9244956003686));
#31843=CARTESIAN_POINT('Ctrl Pts',(-3.7632163498541,-3.16811405982065,41.9300336180666));
#31844=CARTESIAN_POINT('Ctrl Pts',(-3.69948028552799,-3.24231172587062,
41.9355716357646));
#31845=CARTESIAN_POINT('Ctrl Pts',(-3.63359857721944,-3.31453532823666,
41.9411096534626));
#31846=CARTESIAN_POINT('Ctrl Pts',(-3.53656750692421,-3.42090678729676,
41.9492660871427));
#31847=CARTESIAN_POINT('Ctrl Pts',(-3.43484415123915,-3.52303440723009,
41.9574225208228));
#31848=CARTESIAN_POINT('Ctrl Pts',(-3.32882302515633,-3.62051382122608,
41.9655789545029));
#31849=CARTESIAN_POINT('Ctrl Pts',(-3.22282347736149,-3.71797339541329,
41.9737337281188));
#31850=CARTESIAN_POINT('Ctrl Pts',(-3.1125281503641,-3.81078642461029,41.9818885017348));
#31851=CARTESIAN_POINT('Ctrl Pts',(-2.99836716903939,-3.89858658774263,
41.9900432753507));
#31852=CARTESIAN_POINT('Ctrl Pts',(-2.88420213920718,-3.98638986454493,
41.9981983381605));
#31853=CARTESIAN_POINT('Ctrl Pts',(-2.76617144368788,-4.06917971259167,
42.0063534009703));
#31854=CARTESIAN_POINT('Ctrl Pts',(-2.64473732413514,-4.14663086720129,
42.0145084637802));
#31855=CARTESIAN_POINT('Ctrl Pts',(-2.52331032668454,-4.22407747930641,
42.0226630482962));
#31856=CARTESIAN_POINT('Ctrl Pts',(-2.39848058719828,-4.29618584525402,
42.0308176328122));
#31857=CARTESIAN_POINT('Ctrl Pts',(-2.27073823717365,-4.3626747438627,42.0389722173282));
#31858=CARTESIAN_POINT('Ctrl Pts',(-2.14296447979213,-4.42917998975611,
42.0471288067701));
#31859=CARTESIAN_POINT('Ctrl Pts',(-2.01227697778862,-4.4900628527459,42.055285396212));
#31860=CARTESIAN_POINT('Ctrl Pts',(-1.87918985020415,-4.54508840061331,
42.0634419856539));
#31861=CARTESIAN_POINT('Ctrl Pts',(-1.78882869212653,-4.58244867969815,
42.0689800033519));
#31862=CARTESIAN_POINT('Ctrl Pts',(-1.69736181924629,-4.61710976318445,
42.0745180210498));
#31863=CARTESIAN_POINT('Ctrl Pts',(-1.60495526908678,-4.64901082454436,
42.0800560387478));
#31864=CARTESIAN_POINT('Ctrl Pts',(-1.4688582143122,-4.69599494512641,42.0882124724279));
#31865=CARTESIAN_POINT('Ctrl Pts',(-1.3306711589202,-4.73700749890126,42.096368906108));
#31866=CARTESIAN_POINT('Ctrl Pts',(-1.19093399887237,-4.77188215202658,
42.1045253397881));
#31867=CARTESIAN_POINT('Ctrl Pts',(-1.05122527927597,-4.80674970717683,
42.112680113404));
#31868=CARTESIAN_POINT('Ctrl Pts',(-0.909967408882027,-4.83548177285114,
42.1208348870199));
#31869=CARTESIAN_POINT('Ctrl Pts',(-0.767713351081594,-4.8579624610603,
42.1289896606358));
#31870=CARTESIAN_POINT('Ctrl Pts',(-0.625454248504764,-4.88044394650539,
42.1371447234456));
#31871=CARTESIAN_POINT('Ctrl Pts',(-0.482199217757345,-4.89667355493871,
42.1452997862555));
#31872=CARTESIAN_POINT('Ctrl Pts',(-0.338509781880459,-4.90658681672619,
42.1534548490653));
#31873=CARTESIAN_POINT('Ctrl Pts',(-0.194828773378184,-4.91649949710161,
42.1616094335813));
#31874=CARTESIAN_POINT('Ctrl Pts',(-0.0507137446299321,-4.92009654988941,
42.1697640180973));
#31875=CARTESIAN_POINT('Ctrl Pts',(0.0932703625784521,-4.91736552454304,
42.1779186026133));
#31876=CARTESIAN_POINT('Ctrl Pts',(0.23728987042118,-4.91463382773348,42.1860751920552));
#31877=CARTESIAN_POINT('Ctrl Pts',(0.381178057679785,-4.90557094998026,
42.1942317814971));
#31878=CARTESIAN_POINT('Ctrl Pts',(0.524371064830764,-4.89021656461841,
42.202388370939));
#31879=CARTESIAN_POINT('Ctrl Pts',(0.621593735344925,-4.87979151399139,
42.207926388637));
#31880=CARTESIAN_POINT('Ctrl Pts',(0.718495968908813,-4.86646722514291,
42.213464406335));
#31881=CARTESIAN_POINT('Ctrl Pts',(0.814902862627231,-4.85026972311664,
42.219002424033));
#31882=CARTESIAN_POINT('Ctrl Pts',(0.956891653165912,-4.82641392158884,
42.2271588577131));
#31883=CARTESIAN_POINT('Ctrl Pts',(1.09785871281386,-4.7963144209411,42.2353152913931));
#31884=CARTESIAN_POINT('Ctrl Pts',(1.23725036662756,-4.76008346489639,42.2434717250732));
#31885=CARTESIAN_POINT('Ctrl Pts',(1.37661365031004,-4.72385988287263,42.2516264986891));
#31886=CARTESIAN_POINT('Ctrl Pts',(1.51440184414399,-4.68150741911794,42.259781272305));
#31887=CARTESIAN_POINT('Ctrl Pts',(1.65007393345286,-4.63318886692949,42.2679360459209));
#31888=CARTESIAN_POINT('Ctrl Pts',(1.78575083412094,-4.58486860121314,42.2760911087307));
#31889=CARTESIAN_POINT('Ctrl Pts',(1.91931116362224,-4.53058193242733,42.2842461715406));
#31890=CARTESIAN_POINT('Ctrl Pts',(2.05023099121036,-4.47054090073903,42.2924012343504));
#31891=CARTESIAN_POINT('Ctrl Pts',(2.18114314036044,-4.41050339045273,42.3005558188664));
#31892=CARTESIAN_POINT('Ctrl Pts',(2.30941479364516,-4.34471233282722,42.3087104033824));
#31893=CARTESIAN_POINT('Ctrl Pts',(2.43454390600623,-4.27342708282567,42.3168649878984));
#31894=CARTESIAN_POINT('Ctrl Pts',(2.55970378322067,-4.20212430628515,42.3250215773403));
#31895=CARTESIAN_POINT('Ctrl Pts',(2.68171928460811,-4.12532480363762,42.3331781667822));
#31896=CARTESIAN_POINT('Ctrl Pts',(2.80011425337252,-4.04333318322397,42.3413347562241));
#31897=CARTESIAN_POINT('Ctrl Pts',(2.88049998775817,-3.987663954293,42.3468727739221));
#31898=CARTESIAN_POINT('Ctrl Pts',(2.95921724134023,-3.9296021464371,42.3524107916201));
#31899=CARTESIAN_POINT('Ctrl Pts',(3.03612487919264,-3.86925429255399,42.357948809318));
#31900=CARTESIAN_POINT('Ctrl Pts',(3.14939502057598,-3.7803735242402,42.3661052429981));
#31901=CARTESIAN_POINT('Ctrl Pts',(3.25878075090655,-3.68649885329559,42.3742616766782));
#31902=CARTESIAN_POINT('Ctrl Pts',(3.36384957693318,-3.58799374111305,42.3824181103582));
#31903=CARTESIAN_POINT('Ctrl Pts',(3.46889701849171,-3.48950867749782,42.3905728839741));
#31904=CARTESIAN_POINT('Ctrl Pts',(3.56962906455316,-3.38639528146084,42.39872765759));
#31905=CARTESIAN_POINT('Ctrl Pts',(3.66564852383467,-3.27905534601182,42.4068824312059));
#31906=CARTESIAN_POINT('Ctrl Pts',(3.76167138826832,-3.17171160395096,42.4150374940157));
#31907=CARTESIAN_POINT('Ctrl Pts',(3.85298110562048,-3.0601412694471,42.4231925568255));
#31908=CARTESIAN_POINT('Ctrl Pts',(3.93921904783645,-2.94478120675586,42.4313476196353));
#31909=CARTESIAN_POINT('Ctrl Pts',(4.02545193220359,-2.82942790992361,42.4395022041513));
#31910=CARTESIAN_POINT('Ctrl Pts',(4.1066134369395,-2.71028559817519,42.4476567886673));
#31911=CARTESIAN_POINT('Ctrl Pts',(4.18238678937876,-2.58782221308382,42.4558113731833));
#31912=CARTESIAN_POINT('Ctrl Pts',(4.25817877182373,-2.46532871854776,42.4639679626251));
#31913=CARTESIAN_POINT('Ctrl Pts',(4.32857977847528,-2.33951280362419,42.472124552067));
#31914=CARTESIAN_POINT('Ctrl Pts',(4.39331742055376,-2.21086976205268,42.4802811415089));
#31915=CARTESIAN_POINT('Ctrl Pts',(4.43727184661854,-2.1235259713621,42.485819159207));
#31916=CARTESIAN_POINT('Ctrl Pts',(4.47861644747507,-2.03487946255657,42.4913571769051));
#31917=CARTESIAN_POINT('Ctrl Pts',(4.51727825841816,-1.94509130853095,42.4968951946032));
#31918=CARTESIAN_POINT('Ctrl Pts',(4.57421966129932,-1.81285064707162,42.5050516282833));
#31919=CARTESIAN_POINT('Ctrl Pts',(4.62536081504526,-1.67808316494529,42.5132080619634));
#31920=CARTESIAN_POINT('Ctrl Pts',(4.67049583020718,-1.54131494592031,42.5213644956435));
#31921=CARTESIAN_POINT('Ctrl Pts',(4.7156216591211,-1.4045745630836,42.5295192692594));
#31922=CARTESIAN_POINT('Ctrl Pts',(4.75474368330076,-1.26583457328144,42.5376740428753));
#31923=CARTESIAN_POINT('Ctrl Pts',(4.78770535195877,-1.12563783044339,42.5458288164913));
#31924=CARTESIAN_POINT('Ctrl Pts',(4.82066818954128,-0.985436115787674,
42.5539838793011));
#31925=CARTESIAN_POINT('Ctrl Pts',(4.84747015421667,-0.843777869596382,
42.5621389421109));
#31926=CARTESIAN_POINT('Ctrl Pts',(4.86800533776923,-0.701218292652367,
42.5702940049208));
#31927=CARTESIAN_POINT('Ctrl Pts',(4.88853931693481,-0.558667076816868,
42.5784485894368));
#31928=CARTESIAN_POINT('Ctrl Pts',(4.9028072035336,-0.415214967344868,42.5866031739529));
#31929=CARTESIAN_POINT('Ctrl Pts',(4.91075471200728,-0.271424429627003,
42.5947577584689));
#31930=CARTESIAN_POINT('Ctrl Pts',(4.91870417449412,-0.127598538866687,
42.6029143479108));
#31931=CARTESIAN_POINT('Ctrl Pts',(4.92033013500527,0.0165656121496476,
42.6110709373527));
#31932=CARTESIAN_POINT('Ctrl Pts',(4.91563036872653,0.160502774285812,42.6192275267946));
#31933=CARTESIAN_POINT('Ctrl Pts',(4.91243940404543,0.258230698066434,42.6247655444925));
#31934=CARTESIAN_POINT('Ctrl Pts',(4.90633342599113,0.355853935948479,42.6303035621903));
#31935=CARTESIAN_POINT('Ctrl Pts',(4.89732542554343,0.453196137258323,42.6358415798882));
#31936=CARTESIAN_POINT('Ctrl Pts',(4.88405837544527,0.596562455781503,42.6439980135683));
#31937=CARTESIAN_POINT('Ctrl Pts',(4.8644890740699,0.739372589486145,42.6521544472484));
#31938=CARTESIAN_POINT('Ctrl Pts',(4.83868842221904,0.881066067433885,42.6603108809285));
#31939=CARTESIAN_POINT('Ctrl Pts',(4.81289302152819,1.02273070676431,42.6684656545444));
#31940=CARTESIAN_POINT('Ctrl Pts',(4.78086886036851,1.16327881471372,42.6766204281603));
#31941=CARTESIAN_POINT('Ctrl Pts',(4.74273818838301,1.30215879943787,42.6847752017762));
#31942=CARTESIAN_POINT('Ctrl Pts',(4.70460616416389,1.4410437092833,42.692930264586));
#31943=CARTESIAN_POINT('Ctrl Pts',(4.66036728076453,1.57826005386353,42.7010853273959));
#31944=CARTESIAN_POINT('Ctrl Pts',(4.61019416539617,1.71326962847273,42.7092403902057));
#31945=CARTESIAN_POINT('Ctrl Pts',(4.56002399267726,1.84827128478053,42.7173949747217));
#31946=CARTESIAN_POINT('Ctrl Pts',(4.50392040175792,1.98106611670505,42.7255495592377));
#31947=CARTESIAN_POINT('Ctrl Pts',(4.44210482652777,2.11113423842225,42.7337041437537));
#31948=CARTESIAN_POINT('Ctrl Pts',(4.38027405301901,2.24123433932179,42.7418607331956));
#31949=CARTESIAN_POINT('Ctrl Pts',(4.31272863244719,2.368606087938,42.7500173226375));
#31950=CARTESIAN_POINT('Ctrl Pts',(4.23973704627174,2.4927520616722,42.7581739120795));
#31951=CARTESIAN_POINT('Ctrl Pts',(4.19017850235765,2.57704251230405,42.7637119297775));
#31952=CARTESIAN_POINT('Ctrl Pts',(4.13811030408637,2.65984639066669,42.7692499474755));
#31953=CARTESIAN_POINT('Ctrl Pts',(4.08362823151483,2.74101505455097,42.7747879651735));
#31954=CARTESIAN_POINT('Ctrl Pts',(4.00338662957051,2.86056086678492,42.7829443988536));
#31955=CARTESIAN_POINT('Ctrl Pts',(3.91787697535166,2.97660306118204,42.7911008325337));
#31956=CARTESIAN_POINT('Ctrl Pts',(3.8274296775319,3.08868339686153,42.7992572662139));
#31957=CARTESIAN_POINT('Ctrl Pts',(3.73700078828703,3.20074092103308,42.8074120398298));
#31958=CARTESIAN_POINT('Ctrl Pts',(3.64163647027939,3.30883793485481,42.8155668134457));
#31959=CARTESIAN_POINT('Ctrl Pts',(3.54170797470053,3.41254856147758,42.8237215870616));
#31960=CARTESIAN_POINT('Ctrl Pts',(3.44177593534285,3.51626286600543,42.8318766498715));
#31961=CARTESIAN_POINT('Ctrl Pts',(3.3372796240035,3.61559022850392,42.8400317126813));
#31962=CARTESIAN_POINT('Ctrl Pts',(3.22862812468748,3.71014063008089,42.8481867754912));
#31963=CARTESIAN_POINT('Ctrl Pts',(3.11998299777377,3.80468548628387,42.8563413600072));
#31964=CARTESIAN_POINT('Ctrl Pts',(3.00718342350491,3.89445372312028,42.8644959445232));
#31965=CARTESIAN_POINT('Ctrl Pts',(2.89067257974526,3.97909475876221,42.8726505290392));
#31966=CARTESIAN_POINT('Ctrl Pts',(2.77413309006171,4.06375660466169,42.8808071184811));
#31967=CARTESIAN_POINT('Ctrl Pts',(2.65388077829091,4.1432885334677,42.8889637079231));
#31968=CARTESIAN_POINT('Ctrl Pts',(2.53038938864306,4.21738219803975,42.897120297365));
#31969=CARTESIAN_POINT('Ctrl Pts',(2.44654337600825,4.26768901176646,42.9026583150629));
#31970=CARTESIAN_POINT('Ctrl Pts',(2.36120480719153,4.31548972530622,42.9081963327607));
#31971=CARTESIAN_POINT('Ctrl Pts',(2.27452890452171,4.36069963709899,42.9137343504586));
#31972=CARTESIAN_POINT('Ctrl Pts',(2.14687199001629,4.42728513164541,42.9218907841386));
#31973=CARTESIAN_POINT('Ctrl Pts',(2.01626533288119,4.48827359741473,42.9300472178187));
#31974=CARTESIAN_POINT('Ctrl Pts',(1.88321831111146,4.54342072179041,42.9382036514988));
#31975=CARTESIAN_POINT('Ctrl Pts',(1.75019836816146,4.5985566221716,42.9463584251146));
#31976=CARTESIAN_POINT('Ctrl Pts',(1.61473936037004,4.64785342484836,42.9545131987305));
#31977=CARTESIAN_POINT('Ctrl Pts',(1.4773710463855,4.69111477729993,42.9626679723464));
#31978=CARTESIAN_POINT('Ctrl Pts',(1.33999786088837,4.73437766393517,42.9708230351562));
#31979=CARTESIAN_POINT('Ctrl Pts',(1.20071555174455,4.77160456796668,42.9789780979659));
#31980=CARTESIAN_POINT('Ctrl Pts',(1.06006994374836,4.80264872511631,42.9871331607757));
#31981=CARTESIAN_POINT('Ctrl Pts',(0.91943258460651,4.83369106152846,42.9952877452917));
#31982=CARTESIAN_POINT('Ctrl Pts',(0.777432413556998,4.85855130532537,43.0034423298077));
#31983=CARTESIAN_POINT('Ctrl Pts',(0.634626325908003,4.87713363451982,43.0115969143237));
#31984=CARTESIAN_POINT('Ctrl Pts',(0.491785127258248,4.8957205324563,43.0197535037656));
#31985=CARTESIAN_POINT('Ctrl Pts',(0.348137948020462,4.90802638808052,43.0279100932075));
#31986=CARTESIAN_POINT('Ctrl Pts',(0.204248317945032,4.91400709066609,43.0360666826493));
#31987=CARTESIAN_POINT('Ctrl Pts',(0.106552666642415,4.91806776296081,43.0416047003474));
#31988=CARTESIAN_POINT('Ctrl Pts',(0.00874537439048287,4.91921367996508,
43.0471427180455));
#31989=CARTESIAN_POINT('Ctrl Pts',(-0.0889967303273905,4.91744472714143,
43.0526807357436));
#31990=CARTESIAN_POINT('Ctrl Pts',(-0.232952029559441,4.91483940025809,
43.0608371694237));
#31991=CARTESIAN_POINT('Ctrl Pts',(-0.376819749187822,4.905907933752,43.0689936031038));
#31992=CARTESIAN_POINT('Ctrl Pts',(-0.52003570499664,4.89067949553318,43.0771500367839));
#31993=CARTESIAN_POINT('Ctrl Pts',(-0.663222512320933,4.87545415673085,
43.0853048103998));
#31994=CARTESIAN_POINT('Ctrl Pts',(-0.805757487907615,4.85393443831742,
43.0934595840157));
#31995=CARTESIAN_POINT('Ctrl Pts',(-0.94708149662502,4.82620137388096,43.1016143576316));
#31996=CARTESIAN_POINT('Ctrl Pts',(-1.08841051713654,4.79846732594277,43.1097694204414));
#31997=CARTESIAN_POINT('Ctrl Pts',(-1.22852815577192,4.76451955182446,43.1179244832513));
#31998=CARTESIAN_POINT('Ctrl Pts',(-1.36688489411388,4.72449031629268,43.1260795460611));
#31999=CARTESIAN_POINT('Ctrl Pts',(-1.5052335178435,4.68446342847256,43.1342341305771));
#32000=CARTESIAN_POINT('Ctrl Pts',(-1.64182112670667,4.63835588673699,43.1423887150931));
#32001=CARTESIAN_POINT('Ctrl Pts',(-1.77611285360357,4.58634998596533,43.1505432996091));
#32002=CARTESIAN_POINT('Ctrl Pts',(-1.91043759811896,4.53433129876944,43.158699889051));
#32003=CARTESIAN_POINT('Ctrl Pts',(-2.04246502045123,4.47641147540973,43.1668564784929));
#32004=CARTESIAN_POINT('Ctrl Pts',(-2.17167916813614,4.41282139375519,43.1750130679348));
#32005=CARTESIAN_POINT('Ctrl Pts',(-2.2594107184132,4.36964611809264,43.1805510856328));
#32006=CARTESIAN_POINT('Ctrl Pts',(-2.34584578144019,4.32385791630896,43.1860891033308));
#32007=CARTESIAN_POINT('Ctrl Pts',(-2.43082902529071,4.27554128880826,43.1916271210288));
#32008=CARTESIAN_POINT('Ctrl Pts',(-2.55599297928736,4.20438020024817,43.1997835547089));
#32009=CARTESIAN_POINT('Ctrl Pts',(-2.67805337935609,4.12770588525251,43.207939988389));
#32010=CARTESIAN_POINT('Ctrl Pts',(-2.79652875741529,4.04581388245298,43.2160964220691));
#32011=CARTESIAN_POINT('Ctrl Pts',(-2.91498002239503,3.9639385469847,43.224251195685));
#32012=CARTESIAN_POINT('Ctrl Pts',(-3.02984744587769,3.87684783239057,43.2324059693009));
#32013=CARTESIAN_POINT('Ctrl Pts',(-3.14067880786713,3.78488040607815,43.2405607429167));
#32014=CARTESIAN_POINT('Ctrl Pts',(-3.25151410028544,3.69290971831139,43.2487158057266));
#32015=CARTESIAN_POINT('Ctrl Pts',(-3.35831278490299,3.59606218355564,43.2568708685364));
#32016=CARTESIAN_POINT('Ctrl Pts',(-3.46065559718248,3.49471685551055,43.2650259313462));
#32017=CARTESIAN_POINT('Ctrl Pts',(-3.56299240706367,3.39337747136139,43.2731805158622));
#32018=CARTESIAN_POINT('Ctrl Pts',(-3.66087363033313,3.2875410578211,43.2813351003782));
#32019=CARTESIAN_POINT('Ctrl Pts',(-3.75391680428009,3.17762359146636,43.2894896848942));
#32020=CARTESIAN_POINT('Ctrl Pts',(-3.84698285427533,3.06767910026755,43.2976462743361));
#32021=CARTESIAN_POINT('Ctrl Pts',(-3.93520826158491,2.95365180664556,43.3058028637779));
#32022=CARTESIAN_POINT('Ctrl Pts',(-4.01825041668673,2.8359912995806,43.3139594532198));
#32023=CARTESIAN_POINT('Ctrl Pts',(-4.07463291919139,2.7561042370862,43.3194974709179));
#32024=CARTESIAN_POINT('Ctrl Pts',(-4.12862683064958,2.67454298974028,43.3250354886159));
#32025=CARTESIAN_POINT('Ctrl Pts',(-4.18013617852421,2.59145607554769,43.3305735063139));
#32026=CARTESIAN_POINT('Ctrl Pts',(-4.25600134786581,2.46908211673472,43.3387301355048));
#32027=CARTESIAN_POINT('Ctrl Pts',(-4.32650323642781,2.34335155656871,43.3468867646957));
#32028=CARTESIAN_POINT('Ctrl Pts',(-4.39136043250718,2.21475430111566,43.3550433938866));
#32029=CARTESIAN_POINT('Ctrl Pts',(-4.45620317192563,2.08618570997482,43.3631982049659));
#32030=CARTESIAN_POINT('Ctrl Pts',(-4.51540357895127,1.95475199723756,43.3713530160451));
#32031=CARTESIAN_POINT('Ctrl Pts',(-4.56872657731634,1.82096692013427,43.3795078271244));
#32032=CARTESIAN_POINT('Ctrl Pts',(-4.62204717503142,1.68718786615712,43.3876622710666));
#32033=CARTESIAN_POINT('Ctrl Pts',(-4.66949076638975,1.55105796907826,43.3958167150089));
#32034=CARTESIAN_POINT('Ctrl Pts',(-4.71087058034712,1.41311055396241,43.4039711589511));
#32035=CARTESIAN_POINT('Ctrl Pts',(-4.72987512545567,1.34975531810086,43.4077162578995));
#32036=CARTESIAN_POINT('Ctrl Pts',(-4.74760132066462,1.2860169573297,43.4114613568478));
#32037=CARTESIAN_POINT('Ctrl Pts',(-4.76403458704966,1.22194824599677,43.4152064557962));
#32038=CARTESIAN_POINT('Ctrl Pts',(-4.91825,1.96574826549505E-7,41.7353816909288));
#32039=CARTESIAN_POINT('Ctrl Pts',(-4.91824999834295,0.0414589360189329,
41.7330369454177));
#32040=CARTESIAN_POINT('Ctrl Pts',(-4.91772577769449,0.0829158324192955,
41.7306889405423));
#32041=CARTESIAN_POINT('Ctrl Pts',(-4.91548943751206,0.171330746432081,
41.7256725857789));
#32042=CARTESIAN_POINT('Ctrl Pts',(-4.91362840060294,0.218280854469932,
41.7230035077778));
#32043=CARTESIAN_POINT('Ctrl Pts',(-4.89973690176757,0.47553305094118,41.7083457066833));
#32044=CARTESIAN_POINT('Ctrl Pts',(-4.8748779851534,0.684920402260462,41.6962822342288));
#32045=CARTESIAN_POINT('Ctrl Pts',(-4.82016070712283,0.981591332392883,
41.6790240941856));
#32046=CARTESIAN_POINT('Ctrl Pts',(-4.80116587870783,1.07064340167463,41.6738235979937));
#32047=CARTESIAN_POINT('Ctrl Pts',(-4.77462291799058,1.18009533524281,41.6674182063602));
#32048=CARTESIAN_POINT('Ctrl Pts',(-4.76939760283999,1.20103934678713,41.6661919108348));
#32049=CARTESIAN_POINT('Ctrl Pts',(-4.76403458703735,1.22194824604475,41.6649672278726));
#32050=CARTESIAN_POINT('Ctrl Pts',(-4.76403458753695,1.22194824409695,41.3199466556564));
#32051=CARTESIAN_POINT('Ctrl Pts',(-4.78146826213841,1.15397922070302,41.3238775906026));
#32052=CARTESIAN_POINT('Ctrl Pts',(-4.79744593121697,1.08564265453963,41.3278086211273));
#32053=CARTESIAN_POINT('Ctrl Pts',(-4.82856266766962,0.938411061313462,
41.3362508087374));
#32054=CARTESIAN_POINT('Ctrl Pts',(-4.84324183803197,0.85944231530701,41.3407623404201));
#32055=CARTESIAN_POINT('Ctrl Pts',(-4.86764476894113,0.707548263030418,
41.3494276890275));
#32056=CARTESIAN_POINT('Ctrl Pts',(-4.87767903794038,0.634694554188753,
41.3535784405592));
#32057=CARTESIAN_POINT('Ctrl Pts',(-4.89329972388572,0.498800862294033,
41.3613209097401));
#32058=CARTESIAN_POINT('Ctrl Pts',(-4.8993102704684,0.435824793795507,41.3649089413183));
#32059=CARTESIAN_POINT('Ctrl Pts',(-4.91353476725405,0.248679868191117,
41.3755781364691));
#32060=CARTESIAN_POINT('Ctrl Pts',(-4.91825326332636,0.124297130125559,
41.3826790327516));
#32061=CARTESIAN_POINT('Ctrl Pts',(-4.91824574010828,-0.1624042430336,41.3990785586708));
#32062=CARTESIAN_POINT('Ctrl Pts',(-4.91021021276699,-0.324580208915229,
41.4083802955372));
#32063=CARTESIAN_POINT('Ctrl Pts',(-4.88910641188229,-0.537074989393775,
41.4205565815289));
#32064=CARTESIAN_POINT('Ctrl Pts',(-4.88324277856568,-0.588006039819476,
41.4234737795619));
#32065=CARTESIAN_POINT('Ctrl Pts',(-4.87216394035304,-0.672576795189148,
41.4283123647917));
#32066=CARTESIAN_POINT('Ctrl Pts',(-4.86739390232583,-0.706270223200602,
41.4302383250399));
#32067=CARTESIAN_POINT('Ctrl Pts',(-4.85179189954285,-0.808797601554587,
41.4360963932494));
#32068=CARTESIAN_POINT('Ctrl Pts',(-4.83984645842322,-0.877453497385237,
41.4400163536086));
#32069=CARTESIAN_POINT('Ctrl Pts',(-4.8035306635876,-1.06276764506488,41.4506201536484));
#32070=CARTESIAN_POINT('Ctrl Pts',(-4.77637297764575,-1.1788313272625,41.4572871740324));
#32071=CARTESIAN_POINT('Ctrl Pts',(-4.72158223677762,-1.3797779098776,41.4689588645705));
#32072=CARTESIAN_POINT('Ctrl Pts',(-4.69580498276877,-1.4651079493051,41.4739565132086));
#32073=CARTESIAN_POINT('Ctrl Pts',(-4.64125945435373,-1.62940110503214,
41.4836895547584));
#32074=CARTESIAN_POINT('Ctrl Pts',(-4.61275798093255,-1.70842057510187,
41.4884218349828));
#32075=CARTESIAN_POINT('Ctrl Pts',(-4.55768556048281,-1.84966397523924,
41.4969901704153));
#32076=CARTESIAN_POINT('Ctrl Pts',(-4.53182761265929,-1.91214352038963,
41.5008200851241));
#32077=CARTESIAN_POINT('Ctrl Pts',(-4.46325790356814,-2.06861484280862,
41.5105206741375));
#32078=CARTESIAN_POINT('Ctrl Pts',(-4.41885999090842,-2.1618312711739,41.5164016534291));
#32079=CARTESIAN_POINT('Ctrl Pts',(-4.29866052499536,-2.39499775533076,
41.5313862491259));
#32080=CARTESIAN_POINT('Ctrl Pts',(-4.218939539997,-2.53279399962172,41.5405044053925));
#32081=CARTESIAN_POINT('Ctrl Pts',(-4.093039384906,-2.72792189764397,41.5537789531341));
#32082=CARTESIAN_POINT('Ctrl Pts',(-4.05203221930347,-2.78846989642242,
41.5579514992963));
#32083=CARTESIAN_POINT('Ctrl Pts',(-3.9876225795225,-2.87914942521153,41.5642752737863));
#32084=CARTESIAN_POINT('Ctrl Pts',(-3.96519455160005,-2.90996004754042,
41.5664373587103));
#32085=CARTESIAN_POINT('Ctrl Pts',(-3.9133204888078,-2.97950888002416,41.5713473573929));
#32086=CARTESIAN_POINT('Ctrl Pts',(-3.88365313393125,-3.01807700826094,
41.5740921488104));
#32087=CARTESIAN_POINT('Ctrl Pts',(-3.81392824469116,-3.10598985877714,
41.5804091673296));
#32088=CARTESIAN_POINT('Ctrl Pts',(-3.77347674232078,-3.15501109885914,
41.5839769189638));
#32089=CARTESIAN_POINT('Ctrl Pts',(-3.61433353977853,-3.3404287153667,41.597680022568));
#32090=CARTESIAN_POINT('Ctrl Pts',(-3.48910572376429,-3.47102461797935,
41.6077826755011));
#32091=CARTESIAN_POINT('Ctrl Pts',(-3.29552091304719,-3.65182080666722,
41.6226752660742));
#32092=CARTESIAN_POINT('Ctrl Pts',(-3.23260775601761,-3.70762729462033,
41.6274128515409));
#32093=CARTESIAN_POINT('Ctrl Pts',(-3.11658926656789,-3.80534156308915,
41.6359858943804));
#32094=CARTESIAN_POINT('Ctrl Pts',(-3.06399109516278,-3.84781905772406,
41.6398151745791));
#32095=CARTESIAN_POINT('Ctrl Pts',(-2.92906990638334,-3.95225828566908,
41.6495033929913));
#32096=CARTESIAN_POINT('Ctrl Pts',(-2.84564497834878,-4.01274224378397,
41.6553725639357));
#32097=CARTESIAN_POINT('Ctrl Pts',(-2.62934323322113,-4.15942366759067,
41.6703010095844));
#32098=CARTESIAN_POINT('Ctrl Pts',(-2.49408883822089,-4.24190660855192,
41.6793746433789));
#32099=CARTESIAN_POINT('Ctrl Pts',(-2.29031221491431,-4.35305618020056,
41.6926441160747));
#32100=CARTESIAN_POINT('Ctrl Pts',(-2.22474380789676,-4.38692868939593,
41.6968553380419));
#32101=CARTESIAN_POINT('Ctrl Pts',(-2.12410379889378,-4.43608229456852,
41.7032235085133));
#32102=CARTESIAN_POINT('Ctrl Pts',(-2.08957541505977,-4.45245075421542,
41.7053915271734));
#32103=CARTESIAN_POINT('Ctrl Pts',(-2.01095020546772,-4.48860758762265,
41.7102891033817));
#32104=CARTESIAN_POINT('Ctrl Pts',(-1.96674540493424,-4.50815166045702,
41.7130156688082));
#32105=CARTESIAN_POINT('Ctrl Pts',(-1.75946466278393,-4.59616662170835,
41.725694401423));
#32106=CARTESIAN_POINT('Ctrl Pts',(-1.59305844408722,-4.65646103651712,
41.735573553184));
#32107=CARTESIAN_POINT('Ctrl Pts',(-1.31732343863914,-4.73985319136102,
41.7517240623595));
#32108=CARTESIAN_POINT('Ctrl Pts',(-1.20982105121891,-4.76842551994967,
41.757967355431));
#32109=CARTESIAN_POINT('Ctrl Pts',(-1.03905534991093,-4.80766521969745,
41.76784349767));
#32110=CARTESIAN_POINT('Ctrl Pts',(-0.976393545826604,-4.82078172258966,
41.7714587199712));
#32111=CARTESIAN_POINT('Ctrl Pts',(-0.842422662975426,-4.84610552273386,
41.7791768761075));
#32112=CARTESIAN_POINT('Ctrl Pts',(-0.771064179777369,-4.85797020850202,
41.7832812456696));
#32113=CARTESIAN_POINT('Ctrl Pts',(-0.659604062264066,-4.87398478606708,
41.7896868500276));
#32114=CARTESIAN_POINT('Ctrl Pts',(-0.61966882467819,-4.87922286191881,
41.7919808347281));
#32115=CARTESIAN_POINT('Ctrl Pts',(-0.388317381686593,-4.90668175349458,
41.8052656342146));
#32116=CARTESIAN_POINT('Ctrl Pts',(-0.195792174507083,-4.91812776017984,
41.816310381747));
#32117=CARTESIAN_POINT('Ctrl Pts',(0.0703404427072187,-4.91829523973346,
41.831524776406));
#32118=CARTESIAN_POINT('Ctrl Pts',(0.143768449695054,-4.91669672222125,
41.8357159642206));
#32119=CARTESIAN_POINT('Ctrl Pts',(0.252195212667689,-4.91190516517075,
41.8418875414384));
#32120=CARTESIAN_POINT('Ctrl Pts',(0.28723949564373,-4.90998047784177,41.8438795131818));
#32121=CARTESIAN_POINT('Ctrl Pts',(0.367011835674681,-4.90474226574988,
41.8484062294555));
#32122=CARTESIAN_POINT('Ctrl Pts',(0.411721264180349,-4.90119169651795,
41.8509380988311));
#32123=CARTESIAN_POINT('Ctrl Pts',(0.512136669721743,-4.89183353431111,
41.8566200353967));
#32124=CARTESIAN_POINT('Ctrl Pts',(0.567804666801672,-4.88568492997573,
41.8597668434518));
#32125=CARTESIAN_POINT('Ctrl Pts',(0.772791134399405,-4.85949302046122,
41.8713639172521));
#32126=CARTESIAN_POINT('Ctrl Pts',(0.921270353701851,-4.83354317513823,
41.8797852251462));
#32127=CARTESIAN_POINT('Ctrl Pts',(1.17326617207594,-4.77746666718741,41.8942693710833));
#32128=CARTESIAN_POINT('Ctrl Pts',(1.27741335768919,-4.75067952679031,41.9003124181546));
#32129=CARTESIAN_POINT('Ctrl Pts',(1.44628443532835,-4.70129005464826,41.9102415177723));
#32130=CARTESIAN_POINT('Ctrl Pts',(1.5115622398915,-4.68071002102609,41.9141120872799));
#32131=CARTESIAN_POINT('Ctrl Pts',(1.65464142399416,-4.63229634138064,41.9226762255247));
#32132=CARTESIAN_POINT('Ctrl Pts',(1.7322137797442,-4.60385086888244,41.9273729490046));
#32133=CARTESIAN_POINT('Ctrl Pts',(1.85425940333453,-4.5555757781442,41.934853965427));
#32134=CARTESIAN_POINT('Ctrl Pts',(1.89921861626164,-4.5370163340833,41.9376299426208));
#32135=CARTESIAN_POINT('Ctrl Pts',(2.10339276094308,-4.44916523608741,41.9503299228384));
#32136=CARTESIAN_POINT('Ctrl Pts',(2.25914398675065,-4.37213914781538,41.960284849285));
#32137=CARTESIAN_POINT('Ctrl Pts',(2.46532365935948,-4.25620945680664,41.9737915474427));
#32138=CARTESIAN_POINT('Ctrl Pts',(2.51955652948589,-4.22433127473398,41.9773762863516));
#32139=CARTESIAN_POINT('Ctrl Pts',(2.60480794058896,-4.1719944195412,41.983057178481));
#32140=CARTESIAN_POINT('Ctrl Pts',(2.63623149898349,-4.152209697445,41.9851609705178));
#32141=CARTESIAN_POINT('Ctrl Pts',(2.7176023189276,-4.09968135243938,41.9906355123418));
#32142=CARTESIAN_POINT('Ctrl Pts',(2.76718258044623,-4.066380485095,41.9939989621819));
#32143=CARTESIAN_POINT('Ctrl Pts',(2.85374281739485,-4.00592538377377,41.9999335679571));
#32144=CARTESIAN_POINT('Ctrl Pts',(2.89097217574454,-3.97914138467089,42.002507123327));
#32145=CARTESIAN_POINT('Ctrl Pts',(3.11348802312907,-3.81428485716825,42.0180358591635));
#32146=CARTESIAN_POINT('Ctrl Pts',(3.28922797512425,-3.66381696173719,42.0309388891167));
#32147=CARTESIAN_POINT('Ctrl Pts',(3.50264312886879,-3.45331621944992,42.0478459158636));
#32148=CARTESIAN_POINT('Ctrl Pts',(3.55053288105708,-3.40405903592437,42.0517286284355));
#32149=CARTESIAN_POINT('Ctrl Pts',(3.65057592248512,-3.29675070719402,42.0600420731277));
#32150=CARTESIAN_POINT('Ctrl Pts',(3.70241120154293,-3.23842876781273,42.0644745158542));
#32151=CARTESIAN_POINT('Ctrl Pts',(3.81303424578794,-3.10783316743587,42.0742228383146));
#32152=CARTESIAN_POINT('Ctrl Pts',(3.87120050215024,-3.03507225320405,42.0795416393546));
#32153=CARTESIAN_POINT('Ctrl Pts',(4.02498294934978,-2.83108549920251,42.0941540510023));
#32154=CARTESIAN_POINT('Ctrl Pts',(4.11622385892783,-2.69670805516866,42.1034587297558));
#32155=CARTESIAN_POINT('Ctrl Pts',(4.22734513521814,-2.51423345371774,42.1156411936139));
#32156=CARTESIAN_POINT('Ctrl Pts',(4.25334981672572,-2.46998627023712,42.1185615790627));
#32157=CARTESIAN_POINT('Ctrl Pts',(4.29543329902736,-2.39574479742117,42.1234028100309));
#32158=CARTESIAN_POINT('Ctrl Pts',(4.31190159806422,-2.36597654064881,42.1253282482596));
#32159=CARTESIAN_POINT('Ctrl Pts',(4.36109527402262,-2.27483374092049,42.1311786574019));
#32160=CARTESIAN_POINT('Ctrl Pts',(4.39282891291845,-2.21293354247245,42.1350915324189));
#32161=CARTESIAN_POINT('Ctrl Pts',(4.47514653178693,-2.04360978529466,42.1456636650785));
#32162=CARTESIAN_POINT('Ctrl Pts',(4.52317095601327,-1.934994096763,42.1523062186312));
#32163=CARTESIAN_POINT('Ctrl Pts',(4.61849258626033,-1.69641050550479,42.1667033427042));
#32164=CARTESIAN_POINT('Ctrl Pts',(4.66433442413089,-1.56597128063498,42.174455701559));
#32165=CARTESIAN_POINT('Ctrl Pts',(4.72301572900435,-1.37342146409309,42.1858057609224));
#32166=CARTESIAN_POINT('Ctrl Pts',(4.74024615203225,-1.31271870740899,42.1893703817511));
#32167=CARTESIAN_POINT('Ctrl Pts',(4.7750972473327,-1.18028907343636,42.197124778236));
#32168=CARTESIAN_POINT('Ctrl Pts',(4.79227982713729,-1.10846285581646,42.2013166561303));
#32169=CARTESIAN_POINT('Ctrl Pts',(4.82489694221028,-0.957134852701533,
42.2101262170268));
#32170=CARTESIAN_POINT('Ctrl Pts',(4.83999841036697,-0.877583519891493,
42.2147447034327));
#32171=CARTESIAN_POINT('Ctrl Pts',(4.88128329827952,-0.626409115539993,
42.2292918013363));
#32172=CARTESIAN_POINT('Ctrl Pts',(4.90034941114294,-0.453751745148835,
42.2392442297513));
#32173=CARTESIAN_POINT('Ctrl Pts',(4.91364998682027,-0.220878031865666,
42.2525589626708));
#32174=CARTESIAN_POINT('Ctrl Pts',(4.91596805240399,-0.161249893960139,
42.255958178116));
#32175=CARTESIAN_POINT('Ctrl Pts',(4.91796763627068,-0.0644689256229611,
42.2614541200559));
#32176=CARTESIAN_POINT('Ctrl Pts',(4.91831421026547,-0.0273364577794288,
42.2635573301803));
#32177=CARTESIAN_POINT('Ctrl Pts',(4.91811482613601,0.0727585668633859,
42.2692137532208));
#32178=CARTESIAN_POINT('Ctrl Pts',(4.91678039762902,0.135712632036464,42.2727583931672));
#32179=CARTESIAN_POINT('Ctrl Pts',(4.91027865480378,0.296574726575932,42.2818043622942));
#32180=CARTESIAN_POINT('Ctrl Pts',(4.90339202350842,0.394385463358169,42.2872941489556));
#32181=CARTESIAN_POINT('Ctrl Pts',(4.87821013162124,0.644890503382736,42.3013983236737));
#32182=CARTESIAN_POINT('Ctrl Pts',(4.8556698595457,0.797049138790904,42.31000967247));
#32183=CARTESIAN_POINT('Ctrl Pts',(4.81193781434942,1.01970183974714,42.3227916363123));
#32184=CARTESIAN_POINT('Ctrl Pts',(4.79623455846469,1.09117884259339,42.3269224504351));
#32185=CARTESIAN_POINT('Ctrl Pts',(4.761889151693,1.23239693843704,42.3351492623066));
#32186=CARTESIAN_POINT('Ctrl Pts',(4.74329471029247,1.30213118950776,42.3392439508935));
#32187=CARTESIAN_POINT('Ctrl Pts',(4.67551976107667,1.53554644809615,42.3530697073029));
#32188=CARTESIAN_POINT('Ctrl Pts',(4.61934581909466,1.69706534359335,42.3628420665752));
#32189=CARTESIAN_POINT('Ctrl Pts',(4.50793384068396,1.97058445732451,42.379749043948));
#32190=CARTESIAN_POINT('Ctrl Pts',(4.45662949106227,2.08401648138289,42.3868714550785));
#32191=CARTESIAN_POINT('Ctrl Pts',(4.38199739879884,2.23363135011527,42.396389986966));
#32192=CARTESIAN_POINT('Ctrl Pts',(4.36241905275076,2.2716316330271,42.3988185436065));
#32193=CARTESIAN_POINT('Ctrl Pts',(4.32264400770027,2.34642125744497,42.4036176959562));
#32194=CARTESIAN_POINT('Ctrl Pts',(4.30246683418375,2.38321697022707,42.4059882827341));
#32195=CARTESIAN_POINT('Ctrl Pts',(4.26897887899566,2.44247491864791,42.4098257045104));
#32196=CARTESIAN_POINT('Ctrl Pts',(4.25595590086876,2.46509711315591,42.4112953992567));
#32197=CARTESIAN_POINT('Ctrl Pts',(4.22304820135549,2.52122286989272,42.4149550547808));
#32198=CARTESIAN_POINT('Ctrl Pts',(4.20294428298014,2.55459590699801,42.4171431101807));
#32199=CARTESIAN_POINT('Ctrl Pts',(4.09959651579776,2.7216330402359,42.4281650431971));
#32200=CARTESIAN_POINT('Ctrl Pts',(4.01036416074755,2.85148336686231,42.4369659108808));
#32201=CARTESIAN_POINT('Ctrl Pts',(3.85314607296535,3.05825296477085,42.4515444357786));
#32202=CARTESIAN_POINT('Ctrl Pts',(3.78871071201494,3.13772475324658,42.4572964803272));
#32203=CARTESIAN_POINT('Ctrl Pts',(3.67727937162022,3.26671808171373,42.466918262427));
#32204=CARTESIAN_POINT('Ctrl Pts',(3.6316463498605,3.31737475322205,42.470774777077));
#32205=CARTESIAN_POINT('Ctrl Pts',(3.52687976890691,3.42892160478497,42.4794533848701));
#32206=CARTESIAN_POINT('Ctrl Pts',(3.46719346185386,3.48926260437263,42.4842794034255));
#32207=CARTESIAN_POINT('Ctrl Pts',(3.3302643955707,3.62070945306302,42.495101915236));
#32208=CARTESIAN_POINT('Ctrl Pts',(3.25224577050737,3.69094771674969,42.5011024751879));
#32209=CARTESIAN_POINT('Ctrl Pts',(3.06031456817439,3.85292498969766,42.5154772245449));
#32210=CARTESIAN_POINT('Ctrl Pts',(2.94443930401921,3.94218644690316,42.5238516332486));
#32211=CARTESIAN_POINT('Ctrl Pts',(2.78817973782896,4.05181855244548,42.5347233063918));
#32212=CARTESIAN_POINT('Ctrl Pts',(2.75125136656222,4.07698366603932,42.5372631715959));
#32213=CARTESIAN_POINT('Ctrl Pts',(2.68024814915421,4.12396525308612,42.5420884841774));
#32214=CARTESIAN_POINT('Ctrl Pts',(2.64623720515661,4.14587122816908,42.5443747948112));
#32215=CARTESIAN_POINT('Ctrl Pts',(2.50070328490251,4.23708704330978,42.5540622592568));
#32216=CARTESIAN_POINT('Ctrl Pts',(2.3866978821204,4.30233628899259,42.5614168332966));
#32217=CARTESIAN_POINT('Ctrl Pts',(2.12034410681707,4.44093093359853,42.5782377961459));
#32218=CARTESIAN_POINT('Ctrl Pts',(1.96655363436262,4.51114094362899,42.5876958784504));
#32219=CARTESIAN_POINT('Ctrl Pts',(1.74207641943565,4.59995692338875,42.6012972717376));
#32220=CARTESIAN_POINT('Ctrl Pts',(1.67411537574065,4.6251239438558,42.6053887537905));
#32221=CARTESIAN_POINT('Ctrl Pts',(1.53676941519557,4.67256131950116,42.6136153181782));
#32222=CARTESIAN_POINT('Ctrl Pts',(1.46739589457291,4.69480975555188,42.6177495008221));
#32223=CARTESIAN_POINT('Ctrl Pts',(1.25647007972896,4.75732269014025,42.6302658115973));
#32224=CARTESIAN_POINT('Ctrl Pts',(1.1135817956926,4.79278321057714,42.6386752162634));
#32225=CARTESIAN_POINT('Ctrl Pts',(0.82283836947627,4.85123121956217,42.655650466277));
#32226=CARTESIAN_POINT('Ctrl Pts',(0.675088926216493,4.87398840557148,42.664207994878));
#32227=CARTESIAN_POINT('Ctrl Pts',(0.485613891280755,4.89439025113594,42.6750528853812));
#32228=CARTESIAN_POINT('Ctrl Pts',(0.44464152595815,4.89828242925173,42.677390146362));
#32229=CARTESIAN_POINT('Ctrl Pts',(0.373172931873519,4.9041674755618,42.6814514838657));
#32230=CARTESIAN_POINT('Ctrl Pts',(0.342698195547312,4.906391202701,42.6831784322127));
#32231=CARTESIAN_POINT('Ctrl Pts',(0.267370112003826,4.91118260147091,42.6874377134781));
#32232=CARTESIAN_POINT('Ctrl Pts',(0.222498420766049,4.91341997237629,42.6899666637));
#32233=CARTESIAN_POINT('Ctrl Pts',(0.0881691570063345,4.91827388017301,
42.6975219476056));
#32234=CARTESIAN_POINT('Ctrl Pts',(-0.00133584464349756,4.91906395062976,
42.7025358593237));
#32235=CARTESIAN_POINT('Ctrl Pts',(-0.267548819225381,4.91414763037331,
42.7174524170193));
#32236=CARTESIAN_POINT('Ctrl Pts',(-0.443978456498547,4.90135811955894,
42.7273472855319));
#32237=CARTESIAN_POINT('Ctrl Pts',(-0.688651192920981,4.87030027957279,
42.7412487119144));
#32238=CARTESIAN_POINT('Ctrl Pts',(-0.757771915560402,4.86002539675946,
42.7451953835747));
#32239=CARTESIAN_POINT('Ctrl Pts',(-0.892579329077979,4.83704024000851,
42.7529396669971));
#32240=CARTESIAN_POINT('Ctrl Pts',(-0.958272284839683,4.82445543459781,
42.7567356097733));
#32241=CARTESIAN_POINT('Ctrl Pts',(-1.03624041182122,4.8078637229758,42.7612702051106));
#32242=CARTESIAN_POINT('Ctrl Pts',(-1.04878265084448,4.8051433610489,42.7620005632548));
#32243=CARTESIAN_POINT('Ctrl Pts',(-1.14409409369169,4.78407974174795,42.7675577146463));
#32244=CARTESIAN_POINT('Ctrl Pts',(-1.2263866504212,4.76364837644357,42.7723962213351));
#32245=CARTESIAN_POINT('Ctrl Pts',(-1.46839870945811,4.69687522113875,42.7867494447251));
#32246=CARTESIAN_POINT('Ctrl Pts',(-1.62634219057828,4.64454979553626,42.7962818887211));
#32247=CARTESIAN_POINT('Ctrl Pts',(-1.83466955684611,4.56360002301108,42.8090373401861));
#32248=CARTESIAN_POINT('Ctrl Pts',(-1.8876422479082,4.54194500264105,42.8122966466697));
#32249=CARTESIAN_POINT('Ctrl Pts',(-1.95666861961231,4.5123110696327,42.8165611780751));
#32250=CARTESIAN_POINT('Ctrl Pts',(-1.97307327511633,4.50516205399251,42.8175759824567));
#32251=CARTESIAN_POINT('Ctrl Pts',(-2.02355886129832,4.48283220070061,42.8207028098465));
#32252=CARTESIAN_POINT('Ctrl Pts',(-2.05750652017929,4.46735290334963,42.8228107355714));
#32253=CARTESIAN_POINT('Ctrl Pts',(-2.13523119218239,4.43083845345193,42.8276536085707));
#32254=CARTESIAN_POINT('Ctrl Pts',(-2.17887940099541,4.40953810049727,42.8303856012945));
#32255=CARTESIAN_POINT('Ctrl Pts',(-2.31696911647927,4.33959916798679,42.8390806380816));
#32256=CARTESIAN_POINT('Ctrl Pts',(-2.41015364556278,4.28854595845796,42.8450270439978));
#32257=CARTESIAN_POINT('Ctrl Pts',(-2.63199588235986,4.15748887254156,42.8594622899541));
#32258=CARTESIAN_POINT('Ctrl Pts',(-2.75875114599003,4.07448246509674,42.867949850611));
#32259=CARTESIAN_POINT('Ctrl Pts',(-2.93795315082703,3.94492985015892,42.8804142172744));
#32260=CARTESIAN_POINT('Ctrl Pts',(-2.99355816187002,3.90290271797784,42.8843509852368));
#32261=CARTESIAN_POINT('Ctrl Pts',(-3.08440312362127,3.83115682498211,42.890906758271));
#32262=CARTESIAN_POINT('Ctrl Pts',(-3.12015226109768,3.80209877189608,42.8935197178163));
#32263=CARTESIAN_POINT('Ctrl Pts',(-3.24396531794798,3.69853717286071,42.90268991511));
#32264=CARTESIAN_POINT('Ctrl Pts',(-3.32981107334528,3.62144251197732,42.9092671208973));
#32265=CARTESIAN_POINT('Ctrl Pts',(-3.53288014011062,3.42574388892629,42.9253893071764));
#32266=CARTESIAN_POINT('Ctrl Pts',(-3.6469373827041,3.30405978711162,42.9349444609925));
#32267=CARTESIAN_POINT('Ctrl Pts',(-3.79268107286734,3.13180934805247,42.9478233518442));
#32268=CARTESIAN_POINT('Ctrl Pts',(-3.82995358195832,3.0861165228147,42.9511820532796));
#32269=CARTESIAN_POINT('Ctrl Pts',(-3.87143139036323,3.03335926540453,42.9549920174652));
#32270=CARTESIAN_POINT('Ctrl Pts',(-3.87645106761062,3.02694178407111,42.9554543419386));
#32271=CARTESIAN_POINT('Ctrl Pts',(-3.8857439279696,3.01500015990591,42.9563125299532));
#32272=CARTESIAN_POINT('Ctrl Pts',(-3.89002133424432,3.00947933327095,42.9567084549936));
#32273=CARTESIAN_POINT('Ctrl Pts',(-3.8988101777436,2.99808557321972,42.9575238358861));
#32274=CARTESIAN_POINT('Ctrl Pts',(-3.90332012976419,2.99221153517322,42.9579432639995));
#32275=CARTESIAN_POINT('Ctrl Pts',(-3.91893154896809,2.97178290833572,42.9593987236394));
#32276=CARTESIAN_POINT('Ctrl Pts',(-3.92996504307406,2.95717650889248,42.9604337221512));
#32277=CARTESIAN_POINT('Ctrl Pts',(-3.98092501990951,2.88892555672449,42.9652447742594));
#32278=CARTESIAN_POINT('Ctrl Pts',(-4.0198366551823,2.83453141035297,42.9690072756262));
#32279=CARTESIAN_POINT('Ctrl Pts',(-4.12204467152367,2.68531648394671,42.9791645813815));
#32280=CARTESIAN_POINT('Ctrl Pts',(-4.18317332321165,2.58906123063226,42.985543652617));
#32281=CARTESIAN_POINT('Ctrl Pts',(-4.31291479187739,2.3681571857558,42.9998980479385));
#32282=CARTESIAN_POINT('Ctrl Pts',(-4.37957514475913,2.2424815012222,43.0078718919144));
#32283=CARTESIAN_POINT('Ctrl Pts',(-4.47047247709351,2.05155002280497,43.0197932973901));
#32284=CARTESIAN_POINT('Ctrl Pts',(-4.49892386330193,1.9883826579067,43.0237068213598));
#32285=CARTESIAN_POINT('Ctrl Pts',(-4.5501795236974,1.86784831648449,43.031125494135));
#32286=CARTESIAN_POINT('Ctrl Pts',(-4.57325664898741,1.81061165126279,43.0346279032179));
#32287=CARTESIAN_POINT('Ctrl Pts',(-4.65598482595438,1.59374561061086,43.0478294624908));
#32288=CARTESIAN_POINT('Ctrl Pts',(-4.70840320228429,1.43148792899286,43.0575726033839));
#32289=CARTESIAN_POINT('Ctrl Pts',(-4.75627833364298,1.2518940575934,43.0682126656554));
#32290=CARTESIAN_POINT('Ctrl Pts',(-4.76019186091467,1.23692996090985,43.0690981020617));
#32291=CARTESIAN_POINT('Ctrl Pts',(-4.76403458776301,1.22194824321562,43.0699834446552));
#32292=CARTESIAN_POINT('Origin',(0.,0.,-3.23514056400928));
#32293=CARTESIAN_POINT('',(-4.76410171059494,1.22196554825755,45.1652160615516));
#32294=CARTESIAN_POINT('',(-4.76403458711239,1.22194824575222,44.8197276177568));
#32295=CARTESIAN_POINT('',(-4.76403458704967,1.22194824599672,-3.23514056400928));
#32296=CARTESIAN_POINT('',(-4.91826402150649,8.74528832110429E-5,43.4851405645849));
#32297=CARTESIAN_POINT('Ctrl Pts',(-4.91853989040247,8.72578364425628E-5,
43.4851405759104));
#32298=CARTESIAN_POINT('Ctrl Pts',(-4.91793986603997,-0.725688019748913,
43.5262491429017));
#32299=CARTESIAN_POINT('Ctrl Pts',(-4.57197699803157,-2.26971971343868,
43.6136731716547));
#32300=CARTESIAN_POINT('Ctrl Pts',(-3.0169439135882,-4.14532980999643,43.7474126621693));
#32301=CARTESIAN_POINT('Ctrl Pts',(-0.665975355898803,-5.08352108648301,
43.8863590474545));
#32302=CARTESIAN_POINT('Ctrl Pts',(1.84732758978621,-4.78258200007033,44.0253054327396));
#32303=CARTESIAN_POINT('Ctrl Pts',(3.91033640512676,-3.31586776125381,44.1642518180246));
#32304=CARTESIAN_POINT('Ctrl Pts',(5.02018372348306,-1.04089634155263,44.3031982033099));
#32305=CARTESIAN_POINT('Ctrl Pts',(4.90633943649889,1.48779808617899,44.4421445885949));
#32306=CARTESIAN_POINT('Ctrl Pts',(3.59655358400776,3.65383526294536,44.5810909738801));
#32307=CARTESIAN_POINT('Ctrl Pts',(1.41009216119427,4.9292342111448,44.7200373591652));
#32308=CARTESIAN_POINT('Ctrl Pts',(-1.12008535558171,5.00311089299382,44.8589837444503));
#32309=CARTESIAN_POINT('Ctrl Pts',(-3.37723719792296,3.85745754614969,44.9979301297354));
#32310=CARTESIAN_POINT('Ctrl Pts',(-4.43068290595709,2.32502529465259,45.1000075687692));
#32311=CARTESIAN_POINT('Ctrl Pts',(-4.72283062116011,1.38357984648488,45.1557695460413));
#32312=CARTESIAN_POINT('Ctrl Pts',(-4.76410171059494,1.22196554825755,45.1652160615516));
#32313=CARTESIAN_POINT('Ctrl Pts',(-4.76403458704966,1.22194824599677,43.4152064557962));
#32314=CARTESIAN_POINT('Ctrl Pts',(-4.79981655617157,1.08244435207326,43.4233610741045));
#32315=CARTESIAN_POINT('Ctrl Pts',(-4.8294652316512,0.941373571802003,43.4315156924128));
#32316=CARTESIAN_POINT('Ctrl Pts',(-4.85286714489056,0.79928939473872,43.4396703107211));
#32317=CARTESIAN_POINT('Ctrl Pts',(-4.87627408384022,0.657174704191096,
43.4478266802858));
#32318=CARTESIAN_POINT('Ctrl Pts',(-4.89343152795028,0.514046512543163,
43.4559830498505));
#32319=CARTESIAN_POINT('Ctrl Pts',(-4.90427748832079,0.370466435794071,
43.4641394194152));
#32320=CARTESIAN_POINT('Ctrl Pts',(-4.90666238876036,0.338894848174818,
43.4659329101431));
#32321=CARTESIAN_POINT('Ctrl Pts',(-4.90874232238476,0.307301430314587,
43.4677264008711));
#32322=CARTESIAN_POINT('Ctrl Pts',(-4.91051696718809,0.275692178811611,
43.469519891599));
#32323=CARTESIAN_POINT('Ctrl Pts',(-4.91566914420344,0.183923697163315,
43.4747267824024));
#32324=CARTESIAN_POINT('Ctrl Pts',(-4.9182483645321,0.0920101472215629,
43.4799336732058));
#32325=CARTESIAN_POINT('Ctrl Pts',(-4.91824999922231,8.74627973450961E-5,
43.4851405640092));
#32326=CARTESIAN_POINT('',(-4.91824996470145,0.000108738790900998,43.139742923523));
#32327=CARTESIAN_POINT('Ctrl Pts',(-4.76403458776301,1.22194824321562,43.0699834446552));
#32328=CARTESIAN_POINT('Ctrl Pts',(-4.79189833239463,1.11331529259219,43.0764030942714));
#32329=CARTESIAN_POINT('Ctrl Pts',(-4.81603955611608,1.00375592104383,43.0828186703034));
#32330=CARTESIAN_POINT('Ctrl Pts',(-4.84411789010124,0.851764604974871,
43.0916172854435));
#32331=CARTESIAN_POINT('Ctrl Pts',(-4.8512814194585,0.809968962579472,43.0940262068267));
#32332=CARTESIAN_POINT('Ctrl Pts',(-4.86304828365612,0.735547190689884,
43.0982946416439));
#32333=CARTESIAN_POINT('Ctrl Pts',(-4.86786593734639,0.702957695771933,
43.1001567008045));
#32334=CARTESIAN_POINT('Ctrl Pts',(-4.87850356111361,0.625636224684664,
43.1045608288938));
#32335=CARTESIAN_POINT('Ctrl Pts',(-4.88403629378671,0.58086763831187,43.1070999139326));
#32336=CARTESIAN_POINT('Ctrl Pts',(-4.9084655631868,0.358055942048074,43.1196982949649));
#32337=CARTESIAN_POINT('Ctrl Pts',(-4.91824603941655,0.179149652822579,
43.1296969762547));
#32338=CARTESIAN_POINT('Ctrl Pts',(-4.91824999879737,0.0001087641201062,
43.1397428629973));
#32339=CARTESIAN_POINT('Ctrl Pts',(-4.91824999879801,0.000108735485710791,
43.1397428646039));
#32340=CARTESIAN_POINT('Ctrl Pts',(-4.91825152194942,-0.0687854197295842,
43.1436084781282));
#32341=CARTESIAN_POINT('Ctrl Pts',(-4.9168054561655,-0.137671642017828,
43.1474788561221));
#32342=CARTESIAN_POINT('Ctrl Pts',(-4.91160569186403,-0.261403590180769,
43.1544514189466));
#32343=CARTESIAN_POINT('Ctrl Pts',(-4.90837874198007,-0.316259967515485,
43.1575499875871));
#32344=CARTESIAN_POINT('Ctrl Pts',(-4.89945320902016,-0.434230174882583,
43.164234601591));
#32345=CARTESIAN_POINT('Ctrl Pts',(-4.89345267333092,-0.497311184277488,
43.1678220396809));
#32346=CARTESIAN_POINT('Ctrl Pts',(-4.87562860837595,-0.652761965568253,
43.176701583363));
#32347=CARTESIAN_POINT('Ctrl Pts',(-4.86239746973484,-0.74494498870768,
43.1820016202339));
#32348=CARTESIAN_POINT('Ctrl Pts',(-4.81391824608007,-1.02576070165565,
43.1982653853273));
#32349=CARTESIAN_POINT('Ctrl Pts',(-4.77024343597705,-1.21275342141534,
43.2092662593913));
#32350=CARTESIAN_POINT('Ctrl Pts',(-4.69748845637275,-1.45839771490939,
43.2239010116868));
#32351=CARTESIAN_POINT('Ctrl Pts',(-4.67801035633782,-1.51971738745896,
43.2275691629555));
#32352=CARTESIAN_POINT('Ctrl Pts',(-4.64530932989608,-1.61607066537207,
43.2333509970956));
#32353=CARTESIAN_POINT('Ctrl Pts',(-4.63287982700165,-1.65136541355251,
43.2354725534302));
#32354=CARTESIAN_POINT('Ctrl Pts',(-4.60218738190195,-1.73544445172709,
43.2405349039856));
#32355=CARTESIAN_POINT('Ctrl Pts',(-4.58354985423037,-1.78408715263861,
43.2434712945121));
#32356=CARTESIAN_POINT('Ctrl Pts',(-4.50325552019519,-1.98408160034568,
43.2555962912099));
#32357=CARTESIAN_POINT('Ctrl Pts',(-4.43484659970565,-2.13261025295212,
43.264728842634));
#32358=CARTESIAN_POINT('Ctrl Pts',(-4.31766666575353,-2.35689859237798,
43.2789143731951));
#32359=CARTESIAN_POINT('Ctrl Pts',(-4.27399931413035,-2.43518912683911,
43.2839439081805));
#32360=CARTESIAN_POINT('Ctrl Pts',(-4.1889920758613,-2.57826015933935,43.2933092356987));
#32361=CARTESIAN_POINT('Ctrl Pts',(-4.14822629805028,-2.64334985518144,
43.2976398604482));
#32362=CARTESIAN_POINT('Ctrl Pts',(-4.10154774336163,-2.71413950040063,
43.3024353799353));
#32363=CARTESIAN_POINT('Ctrl Pts',(-4.09712557371794,-2.72081038510047,
43.3028881406173));
#32364=CARTESIAN_POINT('Ctrl Pts',(-4.05424209950545,-2.78515888950665,
43.3072638649707));
#32365=CARTESIAN_POINT('Ctrl Pts',(-4.01458193948964,-2.8420275766671,43.3111957826454));
#32366=CARTESIAN_POINT('Ctrl Pts',(-3.85883546036585,-3.05558408193904,
43.3262232539209));
#32367=CARTESIAN_POINT('Ctrl Pts',(-3.73467142405501,-3.2061554208934,43.3373783649993));
#32368=CARTESIAN_POINT('Ctrl Pts',(-3.54715267866821,-3.40783732797696,
43.3531416420693));
#32369=CARTESIAN_POINT('Ctrl Pts',(-3.49096980813066,-3.4653682783922,43.3577412841364));
#32370=CARTESIAN_POINT('Ctrl Pts',(-3.42012805940218,-3.53443783255248,
43.3633868034433));
#32371=CARTESIAN_POINT('Ctrl Pts',(-3.40678135616785,-3.54730426230337,
43.3644439141571));
#32372=CARTESIAN_POINT('Ctrl Pts',(-3.38327652929071,-3.56970826894852,
43.3662940902315));
#32373=CARTESIAN_POINT('Ctrl Pts',(-3.37315003515859,-3.57927870400781,
43.3670875064247));
#32374=CARTESIAN_POINT('Ctrl Pts',(-3.33409833211508,-3.61587310702537,
43.3701329697306));
#32375=CARTESIAN_POINT('Ctrl Pts',(-3.30488771661572,-3.64259073257102,
43.3723811388362));
#32376=CARTESIAN_POINT('Ctrl Pts',(-3.2433600458981,-3.69751787899867,43.3770530295919));
#32377=CARTESIAN_POINT('Ctrl Pts',(-3.21099000400205,-3.72566317654222,
43.3794756011215));
#32378=CARTESIAN_POINT('Ctrl Pts',(-3.08418950153598,-3.8330341975231,43.3888408558411));
#32379=CARTESIAN_POINT('Ctrl Pts',(-2.9871612144794,-3.90912324501609,43.3957457254493));
#32380=CARTESIAN_POINT('Ctrl Pts',(-2.79082122974245,-4.05150908185092,
43.4093332183293));
#32381=CARTESIAN_POINT('Ctrl Pts',(-2.6917514812885,-4.11799498736891,43.4160112617119));
#32382=CARTESIAN_POINT('Ctrl Pts',(-2.53056583311945,-4.21786297190447,
43.4266641301714));
#32383=CARTESIAN_POINT('Ctrl Pts',(-2.46998067228436,-4.25362514070655,
43.4306226212917));
#32384=CARTESIAN_POINT('Ctrl Pts',(-2.35533552972503,-4.31802232909803,
43.438040267627));
#32385=CARTESIAN_POINT('Ctrl Pts',(-2.30146783739031,-4.3469722781125,43.4414963826605));
#32386=CARTESIAN_POINT('Ctrl Pts',(-2.17971443465775,-4.40950819080015,
43.4492497933608));
#32387=CARTESIAN_POINT('Ctrl Pts',(-2.11156464249852,-4.44254567513833,
43.4535502341621));
#32388=CARTESIAN_POINT('Ctrl Pts',(-1.85495803309457,-4.55970383136814,
43.4696100326151));
#32389=CARTESIAN_POINT('Ctrl Pts',(-1.66202950947703,-4.63351103337953,
43.481431899591));
#32390=CARTESIAN_POINT('Ctrl Pts',(-1.40518128028971,-4.71365893260436,
43.496821811754));
#32391=CARTESIAN_POINT('Ctrl Pts',(-1.34497087940044,-4.73119101145091,
43.5004044386737));
#32392=CARTESIAN_POINT('Ctrl Pts',(-1.28044691334274,-4.74864779581115,
43.5042140730092));
#32393=CARTESIAN_POINT('Ctrl Pts',(-1.27645103650703,-4.74972345910679,
43.5044498773198));
#32394=CARTESIAN_POINT('Ctrl Pts',(-1.26994867456583,-4.75146505326014,
43.504833395909));
#32395=CARTESIAN_POINT('Ctrl Pts',(-1.26744301332547,-4.75213404654851,
43.5049811355492));
#32396=CARTESIAN_POINT('Ctrl Pts',(-1.26026571492561,-4.75404425253578,
43.5054041881589));
#32397=CARTESIAN_POINT('Ctrl Pts',(-1.2555927731346,-4.75528056116606,43.5056794591307));
#32398=CARTESIAN_POINT('Ctrl Pts',(-1.24693613082025,-4.75755717781354,
43.5061890875975));
#32399=CARTESIAN_POINT('Ctrl Pts',(-1.24295293264208,-4.75859937605481,
43.5064234617508));
#32400=CARTESIAN_POINT('Ctrl Pts',(-1.23550191162642,-4.76053893166058,
43.506861654641));
#32401=CARTESIAN_POINT('Ctrl Pts',(-1.23203440854394,-4.76143750454435,
43.5070654845116));
#32402=CARTESIAN_POINT('Ctrl Pts',(-1.2254779833316,-4.76312890281656,43.5074507127246));
#32403=CARTESIAN_POINT('Ctrl Pts',(-1.22238926604898,-4.76392251351199,
43.5076321184935));
#32404=CARTESIAN_POINT('Ctrl Pts',(-1.21647893336233,-4.76543497966646,
43.5079790994748));
#32405=CARTESIAN_POINT('Ctrl Pts',(-1.21365744738248,-4.76615433459436,
43.5081446795374));
#32406=CARTESIAN_POINT('Ctrl Pts',(-1.20818530755234,-4.76754431555724,
43.5084656926403));
#32407=CARTESIAN_POINT('Ctrl Pts',(-1.20553473012765,-4.76821523766048,
43.5086211286155));
#32408=CARTESIAN_POINT('Ctrl Pts',(-1.20031339704241,-4.76953224515539,
43.508927210094));
#32409=CARTESIAN_POINT('Ctrl Pts',(-1.1977426758357,-4.77017846324344,43.5090778569212));
#32410=CARTESIAN_POINT('Ctrl Pts',(-1.19258302455681,-4.77147104280929,
43.5093801121957));
#32411=CARTESIAN_POINT('Ctrl Pts',(-1.1899940883102,-4.77211737624181,43.5095317203012));
#32412=CARTESIAN_POINT('Ctrl Pts',(-1.18467288872386,-4.77344122552053,
43.509843219756));
#32413=CARTESIAN_POINT('Ctrl Pts',(-1.18194056694358,-4.77411850324285,
43.5100031084844));
#32414=CARTESIAN_POINT('Ctrl Pts',(-1.17613687005925,-4.77555181422003,
43.5103425993022));
#32415=CARTESIAN_POINT('Ctrl Pts',(-1.17306534360852,-4.77630723122596,
43.5105221945211));
#32416=CARTESIAN_POINT('Ctrl Pts',(-1.16499849169799,-4.77828295721755,
43.5109936715882));
#32417=CARTESIAN_POINT('Ctrl Pts',(-1.16000197425946,-4.77949839676865,
43.5112854981055));
#32418=CARTESIAN_POINT('Ctrl Pts',(-1.14101242568745,-4.78408621206411,
43.5123938292887));
#32419=CARTESIAN_POINT('Ctrl Pts',(-1.1270064778424,-4.78740500087081,43.513209693763));
#32420=CARTESIAN_POINT('Ctrl Pts',(-1.09857621702696,-4.79401003440417,
43.5148624930978));
#32421=CARTESIAN_POINT('Ctrl Pts',(-1.08415126491305,-4.79729277321717,
43.5156993958202));
#32422=CARTESIAN_POINT('Ctrl Pts',(-1.0109486525758,-4.81360472404153,43.5199384505068));
#32423=CARTESIAN_POINT('Ctrl Pts',(-0.951949604644167,-4.82561909995732,
43.5233289638008));
#32424=CARTESIAN_POINT('Ctrl Pts',(-0.718843264655956,-4.8686465656558,
43.5366521493606));
#32425=CARTESIAN_POINT('Ctrl Pts',(-0.543336824073945,-4.8913434457931,
43.5465286802935));
#32426=CARTESIAN_POINT('Ctrl Pts',(-0.28768509905184,-4.91047296356192,
43.5609121230679));
#32427=CARTESIAN_POINT('Ctrl Pts',(-0.20824910604204,-4.91448263746963,
43.5653800949922));
#32428=CARTESIAN_POINT('Ctrl Pts',(-0.0625257815231578,-4.91829873303621,
43.5735917279016));
#32429=CARTESIAN_POINT('Ctrl Pts',(0.00372761654206807,-4.91869473374925,
43.5773308871879));
#32430=CARTESIAN_POINT('Ctrl Pts',(0.133591835348735,-4.9168470646973,43.5846792309233));
#32431=CARTESIAN_POINT('Ctrl Pts',(0.197191344654252,-4.91470724423495,
43.5882870112361));
#32432=CARTESIAN_POINT('Ctrl Pts',(0.264306035919613,-4.91114428612059,
43.5921062525523));
#32433=CARTESIAN_POINT('Ctrl Pts',(0.267880906296425,-4.91095059023615,
43.5923097206624));
#32434=CARTESIAN_POINT('Ctrl Pts',(0.277024215157225,-4.91044516835131,
43.5928302157821));
#32435=CARTESIAN_POINT('Ctrl Pts',(0.282592338782104,-4.91012787380908,
43.5931472764935));
#32436=CARTESIAN_POINT('Ctrl Pts',(0.419981805093912,-4.90206438304695,
43.6009727177338));
#32437=CARTESIAN_POINT('Ctrl Pts',(0.551437185719577,-4.88902201066443,
43.608511856771));
#32438=CARTESIAN_POINT('Ctrl Pts',(0.800702634722884,-4.85410909537207,
43.6229133671223));
#32439=CARTESIAN_POINT('Ctrl Pts',(0.918553642928687,-4.83319346971291,
43.6297678095367));
#32440=CARTESIAN_POINT('Ctrl Pts',(1.10378012428121,-4.79330026578439,43.6405936498856));
#32441=CARTESIAN_POINT('Ctrl Pts',(1.17171561318913,-4.77714775757889,43.6445753914178));
#32442=CARTESIAN_POINT('Ctrl Pts',(1.27222541599587,-4.75097718474871,43.6504761216196));
#32443=CARTESIAN_POINT('Ctrl Pts',(1.30507640472475,-4.74205834412482,43.6524061444718));
#32444=CARTESIAN_POINT('Ctrl Pts',(1.38710409641628,-4.7188713645488,43.6572284453613));
#32445=CARTESIAN_POINT('Ctrl Pts',(1.43615557325238,-4.70417495287262,43.6601156540084));
#32446=CARTESIAN_POINT('Ctrl Pts',(1.63961572576907,-4.63973682689297,43.6721257048677));
#32447=CARTESIAN_POINT('Ctrl Pts',(1.79174573737449,-4.58313708931061,43.6811916988123));
#32448=CARTESIAN_POINT('Ctrl Pts',(2.02467078138749,-4.48310414457963,43.6954006543413));
#32449=CARTESIAN_POINT('Ctrl Pts',(2.10752090735759,-4.44475758323726,43.7005218232959));
#32450=CARTESIAN_POINT('Ctrl Pts',(2.25977492548273,-4.36907337798522,43.7100889134839));
#32451=CARTESIAN_POINT('Ctrl Pts',(2.32944172869235,-4.33233031184398,43.714529606242));
#32452=CARTESIAN_POINT('Ctrl Pts',(2.45797913870795,-4.26054110918708,43.7228557515115));
#32453=CARTESIAN_POINT('Ctrl Pts',(2.5170583063794,-4.22590692402754,43.7267371005422));
#32454=CARTESIAN_POINT('Ctrl Pts',(2.6778979148647,-4.1270476308415,43.7374642158904));
#32455=CARTESIAN_POINT('Ctrl Pts',(2.77805364377879,-4.06030500447411,43.7443267719396));
#32456=CARTESIAN_POINT('Ctrl Pts',(2.98593512170801,-3.91047975207628,43.7589792175998));
#32457=CARTESIAN_POINT('Ctrl Pts',(3.09286788981614,-3.82646424809568,43.7667680185261));
#32458=CARTESIAN_POINT('Ctrl Pts',(3.23710332245792,-3.70313971808879,43.7776142300466));
#32459=CARTESIAN_POINT('Ctrl Pts',(3.27744670811001,-3.66748208397733,43.7806872929668));
#32460=CARTESIAN_POINT('Ctrl Pts',(3.34946688956328,-3.60168919332307,43.7862419467441));
#32461=CARTESIAN_POINT('Ctrl Pts',(3.38134289213546,-3.57178019971043,43.7887257731442));
#32462=CARTESIAN_POINT('Ctrl Pts',(3.43845085668424,-3.51674653172386,43.7932198893034));
#32463=CARTESIAN_POINT('Ctrl Pts',(3.46381666399771,-3.49176525674311,43.7952322845823));
#32464=CARTESIAN_POINT('Ctrl Pts',(3.53761271156044,-3.41749238387668,43.8011398078678));
#32465=CARTESIAN_POINT('Ctrl Pts',(3.58527826249944,-3.36745272188013,43.8050241595341));
#32466=CARTESIAN_POINT('Ctrl Pts',(3.76314911357139,-3.1726632967138,43.8198284837509));
#32467=CARTESIAN_POINT('Ctrl Pts',(3.88577237932801,-3.02123428987749,43.83069907988));
#32468=CARTESIAN_POINT('Ctrl Pts',(4.02257731209639,-2.83013814319236,43.8439100293275));
#32469=CARTESIAN_POINT('Ctrl Pts',(4.04565323581996,-2.7970520218841,43.8461797843625));
#32470=CARTESIAN_POINT('Ctrl Pts',(4.10899410627445,-2.70381027725212,43.8525308285746));
#32471=CARTESIAN_POINT('Ctrl Pts',(4.14834163122497,-2.64304448146158,43.8566179668104));
#32472=CARTESIAN_POINT('Ctrl Pts',(4.22461127774127,-2.51935729789091,43.8648449470911));
#32473=CARTESIAN_POINT('Ctrl Pts',(4.26150342148319,-2.45643849157217,43.8689839367867));
#32474=CARTESIAN_POINT('Ctrl Pts',(4.37410946980738,-2.25421441809336,43.882152972803));
#32475=CARTESIAN_POINT('Ctrl Pts',(4.44449343058884,-2.11205902867539,43.8912164077224));
#32476=CARTESIAN_POINT('Ctrl Pts',(4.5618893399295,-1.84298249834645,43.9080219693431));
#32477=CARTESIAN_POINT('Ctrl Pts',(4.61077025079294,-1.71703730889549,43.9157530254212));
#32478=CARTESIAN_POINT('Ctrl Pts',(4.66802201502881,-1.54936405509511,43.925838364569));
#32479=CARTESIAN_POINT('Ctrl Pts',(4.68112459044695,-1.50931478938031,43.9282319666503));
#32480=CARTESIAN_POINT('Ctrl Pts',(4.70642425042748,-1.42848356832004,43.9330299208329));
#32481=CARTESIAN_POINT('Ctrl Pts',(4.7186098155937,-1.38770169528908,43.9354339648089));
#32482=CARTESIAN_POINT('Ctrl Pts',(4.76478296272886,-1.22552718041598,43.9449389932172));
#32483=CARTESIAN_POINT('Ctrl Pts',(4.79462780010521,-1.1030042958544,43.9519998448588));
#32484=CARTESIAN_POINT('Ctrl Pts',(4.85361559189301,-0.812739563426895,
43.9685934888011));
#32485=CARTESIAN_POINT('Ctrl Pts',(4.87882382755338,-0.644365628404013,
43.9781183433983));
#32486=CARTESIAN_POINT('Ctrl Pts',(4.90221759773451,-0.403287236064732,
43.9917663677502));
#32487=CARTESIAN_POINT('Ctrl Pts',(4.90760111699421,-0.331404719414036,
43.995836419478));
#32488=CARTESIAN_POINT('Ctrl Pts',(4.91526798566742,-0.186259532728857,
44.0040660205995));
#32489=CARTESIAN_POINT('Ctrl Pts',(4.91749734151612,-0.113011991461616,
44.008224908637));
#32490=CARTESIAN_POINT('Ctrl Pts',(4.91931423056557,0.111825301323258,44.0210185839678));
#32491=CARTESIAN_POINT('Ctrl Pts',(4.91353173762474,0.263367203574707,44.0296827038052));
#32492=CARTESIAN_POINT('Ctrl Pts',(4.89240617472781,0.513202781487619,44.044035220973));
#32493=CARTESIAN_POINT('Ctrl Pts',(4.88106529612849,0.611732774583815,44.0497125846265));
#32494=CARTESIAN_POINT('Ctrl Pts',(4.85760980282273,0.772543745433108,44.0589927581509));
#32495=CARTESIAN_POINT('Ctrl Pts',(4.84725528944837,0.835052773569074,44.062603465774));
#32496=CARTESIAN_POINT('Ctrl Pts',(4.82891980000988,0.933860782855306,44.0683106679693));
#32497=CARTESIAN_POINT('Ctrl Pts',(4.82173023134731,0.970298931859938,44.0704149637746));
#32498=CARTESIAN_POINT('Ctrl Pts',(4.80198473120465,1.06472810337526,44.0758681358995));
#32499=CARTESIAN_POINT('Ctrl Pts',(4.78879092047,1.12257959120609,44.0792098635822));
#32500=CARTESIAN_POINT('Ctrl Pts',(4.73186296571308,1.35288842193023,44.0925454329489));
#32501=CARTESIAN_POINT('Ctrl Pts',(4.67983255726093,1.52315530015966,44.1024812832804));
#32502=CARTESIAN_POINT('Ctrl Pts',(4.59131419391572,1.76503913388939,44.1169321438822));
#32503=CARTESIAN_POINT('Ctrl Pts',(4.56212365262991,1.83917285515254,44.1214076994404));
#32504=CARTESIAN_POINT('Ctrl Pts',(4.50267115091603,1.98002455630716,44.1300198024367));
#32505=CARTESIAN_POINT('Ctrl Pts',(4.47269393182329,2.04683989701316,44.1341534047749));
#32506=CARTESIAN_POINT('Ctrl Pts',(4.4139858934759,2.17023845461827,44.1418886587215));
#32507=CARTESIAN_POINT('Ctrl Pts',(4.38563005420559,2.22698346058748,44.1454867629376));
#32508=CARTESIAN_POINT('Ctrl Pts',(4.29435899740368,2.40112497673351,44.1566641574443));
#32509=CARTESIAN_POINT('Ctrl Pts',(4.22776795189248,2.51652493076823,44.1642671275171));
#32510=CARTESIAN_POINT('Ctrl Pts',(4.09204669346087,2.73110041870683,44.1787938270226));
#32511=CARTESIAN_POINT('Ctrl Pts',(4.02378243538841,2.83071203725729,44.185709372804));
#32512=CARTESIAN_POINT('Ctrl Pts',(3.9213802026044,2.96893800221093,44.1955384898348));
#32513=CARTESIAN_POINT('Ctrl Pts',(3.89019450002176,3.00968476244383,44.1984660742475));
#32514=CARTESIAN_POINT('Ctrl Pts',(3.83211505739118,3.08315920574389,44.2037975218062));
#32515=CARTESIAN_POINT('Ctrl Pts',(3.80542510614915,3.11604177090318,44.2062033458529));
#32516=CARTESIAN_POINT('Ctrl Pts',(3.75503337655157,3.17651220958853,44.2106625547058));
#32517=CARTESIAN_POINT('Ctrl Pts',(3.73144385901205,3.20418979464799,44.2127175589637));
#32518=CARTESIAN_POINT('Ctrl Pts',(3.64675734031835,3.30134882480061,44.2199875894225));
#32519=CARTESIAN_POINT('Ctrl Pts',(3.58400871081726,3.3693656765768,44.2251808833597));
#32520=CARTESIAN_POINT('Ctrl Pts',(3.40078275337822,3.5570611626929,44.2398863386702));
#32521=CARTESIAN_POINT('Ctrl Pts',(3.27597656962778,3.67232687045935,44.2493771226828));
#32522=CARTESIAN_POINT('Ctrl Pts',(3.11465286673802,3.80653735209783,44.261174233773));
#32523=CARTESIAN_POINT('Ctrl Pts',(3.08353295378834,3.8317898680272,44.2634294158171));
#32524=CARTESIAN_POINT('Ctrl Pts',(2.99553047140354,3.90143384544104,44.2697529721591));
#32525=CARTESIAN_POINT('Ctrl Pts',(2.93797496275479,3.9449577709444,44.2738271988745));
#32526=CARTESIAN_POINT('Ctrl Pts',(2.82015164935803,4.0300476360955,44.2820560083392));
#32527=CARTESIAN_POINT('Ctrl Pts',(2.75987150822825,4.07156583672237,44.2862098823285));
#32528=CARTESIAN_POINT('Ctrl Pts',(2.57038848720667,4.19593110155218,44.2991060364627));
#32529=CARTESIAN_POINT('Ctrl Pts',(2.4382194291894,4.27408701243943,44.3078787247829));
#32530=CARTESIAN_POINT('Ctrl Pts',(2.1802038551831,4.41079189045899,44.324593648911));
#32531=CARTESIAN_POINT('Ctrl Pts',(2.05510640848856,4.47044876979039,44.3325256961509));
#32532=CARTESIAN_POINT('Ctrl Pts',(1.88870662544854,4.54133932124927,44.3428217522653));
#32533=CARTESIAN_POINT('Ctrl Pts',(1.84954332404184,4.55742965889241,44.3452269303542));
#32534=CARTESIAN_POINT('Ctrl Pts',(1.77079475246199,4.58860141814315,44.3500248391241));
#32535=CARTESIAN_POINT('Ctrl Pts',(1.73121258765669,4.60368114258355,44.3524173633981));
#32536=CARTESIAN_POINT('Ctrl Pts',(1.60719969005676,4.64910105499918,44.3598624188259));
#32537=CARTESIAN_POINT('Ctrl Pts',(1.52212989081448,4.67764388889822,44.3648969773721));
#32538=CARTESIAN_POINT('Ctrl Pts',(1.41643970189314,4.70991655851346,44.3710918161928));
#32539=CARTESIAN_POINT('Ctrl Pts',(1.39651469062305,4.71586282003662,44.3722570723154));
#32540=CARTESIAN_POINT('Ctrl Pts',(1.2219272239183,4.76676179962567,44.3824467752625));
#32541=CARTESIAN_POINT('Ctrl Pts',(1.06518191466581,4.80421805641786,44.391458088435));
#32542=CARTESIAN_POINT('Ctrl Pts',(0.829006286209752,4.8485265656227,44.4049779487915));
#32543=CARTESIAN_POINT('Ctrl Pts',(0.750788706982978,4.86125265716742,44.4094455413212));
#32544=CARTESIAN_POINT('Ctrl Pts',(0.60382814628672,4.88153173638036,44.4178348827674));
#32545=CARTESIAN_POINT('Ctrl Pts',(0.535166757228402,4.88953545036023,44.4217525293836));
#32546=CARTESIAN_POINT('Ctrl Pts',(0.347228864718613,4.90743682421646,44.432479229111));
#32547=CARTESIAN_POINT('Ctrl Pts',(0.227724530074298,4.91443231737883,44.4393046159908));
#32548=CARTESIAN_POINT('Ctrl Pts',(-0.0284992312444243,4.92006455991003,
44.4539588428542));
#32549=CARTESIAN_POINT('Ctrl Pts',(-0.165149669952706,4.91737460881972,
44.4617870193344));
#32550=CARTESIAN_POINT('Ctrl Pts',(-0.355354550713006,4.90569223810771,
44.4726786749573));
#32551=CARTESIAN_POINT('Ctrl Pts',(-0.409140973214535,4.90149945678584,
44.4757578700689));
#32552=CARTESIAN_POINT('Ctrl Pts',(-0.506418699326991,4.89230401232429,
44.4813218964911));
#32553=CARTESIAN_POINT('Ctrl Pts',(-0.549933019911619,4.88760393050412,
44.4838089750873));
#32554=CARTESIAN_POINT('Ctrl Pts',(-0.634181586608494,4.87736467880084,
44.4886181356272));
#32555=CARTESIAN_POINT('Ctrl Pts',(-0.674920539169764,4.87189437521179,
44.490940682854));
#32556=CARTESIAN_POINT('Ctrl Pts',(-0.835270375089106,4.84831316159673,
44.500080271994));
#32557=CARTESIAN_POINT('Ctrl Pts',(-0.954265594341402,4.82630240713895,
44.5068592329808));
#32558=CARTESIAN_POINT('Ctrl Pts',(-1.23079571487627,4.76452410618217,44.5227341499816));
#32559=CARTESIAN_POINT('Ctrl Pts',(-1.38741068144754,4.72129632564498,44.5318211275747));
#32560=CARTESIAN_POINT('Ctrl Pts',(-1.61423249430184,4.64642732618781,44.5452666552413));
#32561=CARTESIAN_POINT('Ctrl Pts',(-1.68629601843619,4.62076173346113,44.5495814572408));
#32562=CARTESIAN_POINT('Ctrl Pts',(-1.82241014731488,4.56867598705532,44.5578262192476));
#32563=CARTESIAN_POINT('Ctrl Pts',(-1.8865587344623,4.54256260446731,44.5617530296328));
#32564=CARTESIAN_POINT('Ctrl Pts',(-2.14553186450071,4.43070862474541,44.5777874913885));
#32565=CARTESIAN_POINT('Ctrl Pts',(-2.33524290391109,4.33371942045568,44.5899694233154));
#32566=CARTESIAN_POINT('Ctrl Pts',(-2.60732342661571,4.17155171382374,44.608095779479));
#32567=CARTESIAN_POINT('Ctrl Pts',(-2.69486924348881,4.11553876427635,44.6140348314711));
#32568=CARTESIAN_POINT('Ctrl Pts',(-2.81305613806979,4.03453204446409,44.6221842074669));
#32569=CARTESIAN_POINT('Ctrl Pts',(-2.84526829709359,4.01188011238394,44.624419209061));
#32570=CARTESIAN_POINT('Ctrl Pts',(-2.91503657216522,3.96155533802634,44.6292887831803));
#32571=CARTESIAN_POINT('Ctrl Pts',(-2.95247803262843,3.9337300938032,44.6319212070173));
#32572=CARTESIAN_POINT('Ctrl Pts',(-3.14467766014315,3.78660360301213,44.6455531729767));
#32573=CARTESIAN_POINT('Ctrl Pts',(-3.29262223916538,3.65868891842791,44.6564593687879));
#32574=CARTESIAN_POINT('Ctrl Pts',(-3.49128952495236,3.4650835679661,44.6720190452396));
#32575=CARTESIAN_POINT('Ctrl Pts',(-3.54857319080975,3.4063961635706,44.6766243590785));
#32576=CARTESIAN_POINT('Ctrl Pts',(-3.65494335109643,3.29182302379609,44.6854286590018));
#32577=CARTESIAN_POINT('Ctrl Pts',(-3.70428201514352,3.23620214148702,44.6896242629739));
#32578=CARTESIAN_POINT('Ctrl Pts',(-3.79840661379017,3.12511887595006,44.6978640857508));
#32579=CARTESIAN_POINT('Ctrl Pts',(-3.84328532062073,3.06975871671379,44.7019063797617));
#32580=CARTESIAN_POINT('Ctrl Pts',(-4.00255738073668,2.86431874773125,44.7166889804901));
#32581=CARTESIAN_POINT('Ctrl Pts',(-4.10949075247443,2.70866599345547,44.7274832124058));
#32582=CARTESIAN_POINT('Ctrl Pts',(-4.24965152698669,2.47716742973605,44.7429741166421));
#32583=CARTESIAN_POINT('Ctrl Pts',(-4.29032986445171,2.40602709019556,44.7476619728084));
#32584=CARTESIAN_POINT('Ctrl Pts',(-4.34224490486388,2.30972866904664,44.7539048644201));
#32585=CARTESIAN_POINT('Ctrl Pts',(-4.35507502159775,2.28544501256247,44.7554705843189));
#32586=CARTESIAN_POINT('Ctrl Pts',(-4.38763808194379,2.22254264641352,44.7595036035274));
#32587=CARTESIAN_POINT('Ctrl Pts',(-4.40706496472573,2.1837678925486,44.7619678364715));
#32588=CARTESIAN_POINT('Ctrl Pts',(-4.44403863021987,2.10746750041819,44.7667720063706));
#32589=CARTESIAN_POINT('Ctrl Pts',(-4.46162918476925,2.06996707114031,44.7691122265992));
#32590=CARTESIAN_POINT('Ctrl Pts',(-4.51849525913774,1.94464353446965,44.7768722064486));
#32591=CARTESIAN_POINT('Ctrl Pts',(-4.55566793852529,1.85589004967326,44.7822699029138));
#32592=CARTESIAN_POINT('Ctrl Pts',(-4.63959016408138,1.6377708246366,44.7953695725174));
#32593=CARTESIAN_POINT('Ctrl Pts',(-4.68356273362564,1.50742500397142,44.8030611906426));
#32594=CARTESIAN_POINT('Ctrl Pts',(-4.73483317319724,1.33140471479133,44.8133551025073));
#32595=CARTESIAN_POINT('Ctrl Pts',(-4.74703467783705,1.28722392333865,44.8159310232576));
#32596=CARTESIAN_POINT('Ctrl Pts',(-4.76043811642558,1.23590612239217,44.8189161372267));
#32597=CARTESIAN_POINT('Ctrl Pts',(-4.76224403384605,1.22892911234828,44.8193218361234));
#32598=CARTESIAN_POINT('Ctrl Pts',(-4.76403458711239,1.22194824575222,44.8197276177568));
#32599=CARTESIAN_POINT('Origin',(0.,0.,-3.23514056400928));
#32600=CARTESIAN_POINT('',(-4.76403458328184,1.22194826068645,46.9151580697526));
#32601=CARTESIAN_POINT('',(-4.7640345870679,1.22194824592564,46.5701705954582));
#32602=CARTESIAN_POINT('',(-4.76403458704967,1.22194824599672,-3.23514056400928));
#32603=CARTESIAN_POINT('',(-4.91809585794598,-0.000121275114829886,45.2351405640092));
#32604=CARTESIAN_POINT('Ctrl Pts',(-4.76403458328184,1.22194826068643,46.9151580697526));
#32605=CARTESIAN_POINT('Ctrl Pts',(-4.71829633738443,1.40026889196382,46.9048442910559));
#32606=CARTESIAN_POINT('Ctrl Pts',(-4.66257828953066,1.57589625349177,46.8945393837931));
#32607=CARTESIAN_POINT('Ctrl Pts',(-4.57485811836119,1.80659514119114,46.8806232551198));
#32608=CARTESIAN_POINT('Ctrl Pts',(-4.55146015251469,1.86475821003725,46.877081893628));
#32609=CARTESIAN_POINT('Ctrl Pts',(-4.4985369661167,1.98938045016523,46.8694155881345));
#32610=CARTESIAN_POINT('Ctrl Pts',(-4.46863670209117,2.05566419179987,46.8652887488593));
#32611=CARTESIAN_POINT('Ctrl Pts',(-4.40312557083084,2.19270118742757,46.8566462277294));
#32612=CARTESIAN_POINT('Ctrl Pts',(-4.36725278360166,2.26330648404268,46.8521298839995));
#32613=CARTESIAN_POINT('Ctrl Pts',(-4.24587540400877,2.48856295555406,46.8375092242518));
#32614=CARTESIAN_POINT('Ctrl Pts',(-4.15373819642433,2.63948147354595,46.8273784154705));
#32615=CARTESIAN_POINT('Ctrl Pts',(-4.01977395516314,2.83446387712191,46.8138739176265));
#32616=CARTESIAN_POINT('Ctrl Pts',(-3.98496898468178,2.8831910161078,46.8104626875148));
#32617=CARTESIAN_POINT('Ctrl Pts',(-3.92738047219344,2.96077965509931,46.8049764144071));
#32618=CARTESIAN_POINT('Ctrl Pts',(-3.90514815369414,2.9900420526465,46.8028947300049));
#32619=CARTESIAN_POINT('Ctrl Pts',(-3.84526250171788,3.06705673866384,46.7973810619885));
#32620=CARTESIAN_POINT('Ctrl Pts',(-3.8070479376242,3.1143646027068,46.7939568800489));
#32621=CARTESIAN_POINT('Ctrl Pts',(-3.73744712227841,3.19733121443554,46.787870657866));
#32622=CARTESIAN_POINT('Ctrl Pts',(-3.70640321966736,3.23326662893186,46.7852063645276));
#32623=CARTESIAN_POINT('Ctrl Pts',(-3.52498281349164,3.43722601838593,46.7699015439434));
#32624=CARTESIAN_POINT('Ctrl Pts',(-3.36371447869876,3.59519821461685,46.7573069935311));
#32625=CARTESIAN_POINT('Ctrl Pts',(-3.14020836540225,3.78588715187681,46.7407378109123));
#32626=CARTESIAN_POINT('Ctrl Pts',(-3.08731951954971,3.82913934868015,46.7368768655856));
#32627=CARTESIAN_POINT('Ctrl Pts',(-2.97343879118533,3.91837675327876,46.7286795283935));
#32628=CARTESIAN_POINT('Ctrl Pts',(-2.91224195402836,3.96407129564699,46.7243417949505));
#32629=CARTESIAN_POINT('Ctrl Pts',(-2.76228098598692,4.0706968954961,46.7138637119489));
#32630=CARTESIAN_POINT('Ctrl Pts',(-2.67253209244462,4.13017448846413,46.7077151318762));
#32631=CARTESIAN_POINT('Ctrl Pts',(-2.43379607890237,4.27734553015157,46.6916687777684));
#32632=CARTESIAN_POINT('Ctrl Pts',(-2.28200887370927,4.36021609426409,46.6817631515585));
#32633=CARTESIAN_POINT('Ctrl Pts',(-2.08891893302936,4.45278651543154,46.6695759620893));
#32634=CARTESIAN_POINT('Ctrl Pts',(-2.05143937259055,4.47017747054437,46.6672292422945));
#32635=CARTESIAN_POINT('Ctrl Pts',(-1.97499716930681,4.50448365712826,46.6624832453279));
#32636=CARTESIAN_POINT('Ctrl Pts',(-1.93602556904247,4.5213705763197,46.6600844502966));
#32637=CARTESIAN_POINT('Ctrl Pts',(-1.87221255391581,4.5480452610561,46.6561858685435));
#32638=CARTESIAN_POINT('Ctrl Pts',(-1.84750176980017,4.55813917784168,46.6546832536173));
#32639=CARTESIAN_POINT('Ctrl Pts',(-1.68011192540942,4.62493012222541,46.6445477994749));
#32640=CARTESIAN_POINT('Ctrl Pts',(-1.53492696585616,4.67512080476925,46.6359651676596));
#32641=CARTESIAN_POINT('Ctrl Pts',(-1.26821306145229,4.75355792218286,46.6203821569913));
#32642=CARTESIAN_POINT('Ctrl Pts',(-1.14750526013454,4.78413089519121,46.6133959611574));
#32643=CARTESIAN_POINT('Ctrl Pts',(-0.964357641728391,4.82318776978269,
46.6028377616425));
#32644=CARTESIAN_POINT('Ctrl Pts',(-0.902701577565472,4.83510658410881,
46.5992906476204));
#32645=CARTESIAN_POINT('Ctrl Pts',(-0.769380522184149,4.85824001980595,
46.5916292234332));
#32646=CARTESIAN_POINT('Ctrl Pts',(-0.697661492040328,4.86905645431831,
46.5875130966142));
#32647=CARTESIAN_POINT('Ctrl Pts',(-0.547571828709803,4.88830823290698,
46.5789035041631));
#32648=CARTESIAN_POINT('Ctrl Pts',(-0.469184453617907,4.89645362118847,
46.5744094233842));
#32649=CARTESIAN_POINT('Ctrl Pts',(-0.217473951707847,4.91650928446453,
46.5599819139811));
#32650=CARTESIAN_POINT('Ctrl Pts',(-0.0437030836795273,4.92112267538409,
46.5500228363498));
#32651=CARTESIAN_POINT('Ctrl Pts',(0.192304227126251,4.91488487502529,46.5365421886008));
#32652=CARTESIAN_POINT('Ctrl Pts',(0.254625398569367,4.91205051805763,46.5329873186813));
#32653=CARTESIAN_POINT('Ctrl Pts',(0.353567273468456,4.90566255337063,46.5273567588795));
#32654=CARTESIAN_POINT('Ctrl Pts',(0.390230646557007,4.90288231451022,46.525273543407));
#32655=CARTESIAN_POINT('Ctrl Pts',(0.485099032185484,4.89461740406166,46.5198905551969));
#32656=CARTESIAN_POINT('Ctrl Pts',(0.543243609524901,4.88850561057316,46.5165976785536));
#32657=CARTESIAN_POINT('Ctrl Pts',(0.686824790330378,4.87081986581729,46.5084651316182));
#32658=CARTESIAN_POINT('Ctrl Pts',(0.772092326465536,4.85803335332093,46.5036343240458));
#32659=CARTESIAN_POINT('Ctrl Pts',(1.03210607265405,4.81202343571052,46.4888403984732));
#32660=CARTESIAN_POINT('Ctrl Pts',(1.20542061327895,4.77155872572109,46.4788872265183));
#32661=CARTESIAN_POINT('Ctrl Pts',(1.44466309460734,4.70183185228411,46.4648448524049));
#32662=CARTESIAN_POINT('Ctrl Pts',(1.51272226326294,4.6803787693242,46.46081551324));
#32663=CARTESIAN_POINT('Ctrl Pts',(1.64899073096502,4.63414240051098,46.4526679213942));
#32664=CARTESIAN_POINT('Ctrl Pts',(1.71716665962803,4.60931499431087,46.4485503048024));
#32665=CARTESIAN_POINT('Ctrl Pts',(1.85824513156154,4.55437435756275,46.4399361312323));
#32666=CARTESIAN_POINT('Ctrl Pts',(1.93102308037085,4.52399717607071,46.4354389526067));
#32667=CARTESIAN_POINT('Ctrl Pts',(2.16206595986506,4.42096961395716,46.420984776249));
#32668=CARTESIAN_POINT('Ctrl Pts',(2.31721480760218,4.34166062297294,46.4110020137675));
#32669=CARTESIAN_POINT('Ctrl Pts',(2.52148431848557,4.22316792620064,46.3975184266756));
#32670=CARTESIAN_POINT('Ctrl Pts',(2.57454526237661,4.19103177350427,46.3939837301457));
#32671=CARTESIAN_POINT('Ctrl Pts',(2.65806273235386,4.13826497142618,46.3883736237236));
#32672=CARTESIAN_POINT('Ctrl Pts',(2.68891984521939,4.11828174988093,46.3862908127575));
#32673=CARTESIAN_POINT('Ctrl Pts',(2.76851107397061,4.06546213526557,46.3808912603567));
#32674=CARTESIAN_POINT('Ctrl Pts',(2.81688592508844,4.03209495761634,46.3775815307427));
#32675=CARTESIAN_POINT('Ctrl Pts',(2.97986067101228,3.91531626694129,46.3663109617165));
#32676=CARTESIAN_POINT('Ctrl Pts',(3.09144805251376,3.82782189873297,46.3583850282051));
#32677=CARTESIAN_POINT('Ctrl Pts',(3.28333377693483,3.66349572118424,46.3442262202962));
#32678=CARTESIAN_POINT('Ctrl Pts',(3.36510175102538,3.58853332738484,46.3380046869931));
#32679=CARTESIAN_POINT('Ctrl Pts',(3.49712502614329,3.45901473316727,46.3275897818657));
#32680=CARTESIAN_POINT('Ctrl Pts',(3.54880654167161,3.40597098250362,46.3234109394979));
#32681=CARTESIAN_POINT('Ctrl Pts',(3.64715120612894,3.30036473128972,46.3152449062796));
#32682=CARTESIAN_POINT('Ctrl Pts',(3.69392446893139,3.24792874710778,46.3112598096743));
#32683=CARTESIAN_POINT('Ctrl Pts',(3.8442606265884,3.07194215766255,46.2980993818115));
#32684=CARTESIAN_POINT('Ctrl Pts',(3.94287285336128,2.94430311175795,46.2888874862038));
#32685=CARTESIAN_POINT('Ctrl Pts',(4.11704541404574,2.69438161071431,46.2714501179665));
#32686=CARTESIAN_POINT('Ctrl Pts',(4.19386668191552,2.57317665846754,46.2632368223855));
#32687=CARTESIAN_POINT('Ctrl Pts',(4.28583639555978,2.41298441772688,46.2527239727575));
#32688=CARTESIAN_POINT('Ctrl Pts',(4.30594005857007,2.37692399513839,46.2503790955165));
#32689=CARTESIAN_POINT('Ctrl Pts',(4.34581672495327,2.30322966723391,46.2456329036836));
#32690=CARTESIAN_POINT('Ctrl Pts',(4.36556062182158,2.26558390277515,46.2432320883855));
#32691=CARTESIAN_POINT('Ctrl Pts',(4.3969201104466,2.20385819730931,46.2393295327536));
#32692=CARTESIAN_POINT('Ctrl Pts',(4.40883166269966,2.17993137319487,46.2378249636799));
#32693=CARTESIAN_POINT('Ctrl Pts',(4.48788547468902,2.01783677074203,46.2276827769044));
#32694=CARTESIAN_POINT('Ctrl Pts',(4.54871794328296,1.87668509633149,46.2190953559161));
#32695=CARTESIAN_POINT('Ctrl Pts',(4.64664277458122,1.61658455481906,46.2035170184832));
#32696=CARTESIAN_POINT('Ctrl Pts',(4.68601429891415,1.49863409309824,46.1965403654574));
#32697=CARTESIAN_POINT('Ctrl Pts',(4.73848308488248,1.31905389560385,46.1859921495881));
#32698=CARTESIAN_POINT('Ctrl Pts',(4.75493557021535,1.25845649207369,46.1824453855905));
#32699=CARTESIAN_POINT('Ctrl Pts',(4.78788457113782,1.12721134326059,46.1747836785361));
#32700=CARTESIAN_POINT('Ctrl Pts',(4.80398728777969,1.05648002941471,46.1706669141112));
#32701=CARTESIAN_POINT('Ctrl Pts',(4.83431240041154,0.908195753898404,46.1620553609223));
#32702=CARTESIAN_POINT('Ctrl Pts',(4.8482462702304,0.830604505002049,46.1575599542294));
#32703=CARTESIAN_POINT('Ctrl Pts',(4.88692178095068,0.580874442767008,46.1431210393416));
#32704=CARTESIAN_POINT('Ctrl Pts',(4.90440235258711,0.407746317549911,46.133151832666));
#32705=CARTESIAN_POINT('Ctrl Pts',(4.91563894851584,0.17189882885378,46.119669941679));
#32706=CARTESIAN_POINT('Ctrl Pts',(4.91742044614293,0.109689423657436,46.1161237133948));
#32707=CARTESIAN_POINT('Ctrl Pts',(4.91837577122531,0.0106994988674436,
46.1105019219746));
#32708=CARTESIAN_POINT('Ctrl Pts',(4.91831833985244,-0.0260663951433238,
46.1084188866038));
#32709=CARTESIAN_POINT('Ctrl Pts',(4.91710024160612,-0.121411742409218,
46.1030288676961));
#32710=CARTESIAN_POINT('Ctrl Pts',(4.91530506649278,-0.179977281530277,
46.0997288294157));
#32711=CARTESIAN_POINT('Ctrl Pts',(4.90564257606118,-0.379001129087812,
46.0885275193828));
#32712=CARTESIAN_POINT('Ctrl Pts',(4.89279636445741,-0.519148470412448,
46.0806606819802));
#32713=CARTESIAN_POINT('Ctrl Pts',(4.86509016957856,-0.7242025145272,46.0690643097286));
#32714=CARTESIAN_POINT('Ctrl Pts',(4.85489433259876,-0.789666130355734,
46.0653494360601));
#32715=CARTESIAN_POINT('Ctrl Pts',(4.82742813259212,-0.945273422047215,
46.0564734425241));
#32716=CARTESIAN_POINT('Ctrl Pts',(4.80895100234762,-1.0351783370182,46.0513080612167));
#32717=CARTESIAN_POINT('Ctrl Pts',(4.77259420047312,-1.18997893895328,46.0423272270238));
#32718=CARTESIAN_POINT('Ctrl Pts',(4.75587775141555,-1.25512228792961,46.0385208845561));
#32719=CARTESIAN_POINT('Ctrl Pts',(4.7136476917026,-1.40670846880949,46.0295922723431));
#32720=CARTESIAN_POINT('Ctrl Pts',(4.68708352755543,-1.49283320902282,46.024464148853));
#32721=CARTESIAN_POINT('Ctrl Pts',(4.62008054158398,-1.69059991955772,46.0125503270132));
#32722=CARTESIAN_POINT('Ctrl Pts',(4.57793534893185,-1.80160481476745,46.0057582715919));
#32723=CARTESIAN_POINT('Ctrl Pts',(4.48368623628308,-2.02511352720993,45.9918725160006));
#32724=CARTESIAN_POINT('Ctrl Pts',(4.43126123044029,-2.13739361469917,45.984783386783));
#32725=CARTESIAN_POINT('Ctrl Pts',(4.35521275984951,-2.28541342564937,45.9753093380816));
#32726=CARTESIAN_POINT('Ctrl Pts',(4.33528231373689,-2.32299806834949,45.9728923727802));
#32727=CARTESIAN_POINT('Ctrl Pts',(4.29506805752893,-2.39651317463609,45.9681447086321));
#32728=CARTESIAN_POINT('Ctrl Pts',(4.27481473373422,-2.43245638287808,45.9658138903839));
#32729=CARTESIAN_POINT('Ctrl Pts',(4.18269845006276,-2.59122890727786,45.9554639504351));
#32730=CARTESIAN_POINT('Ctrl Pts',(4.10597613768451,-2.71116108722591,45.947498707409));
#32731=CARTESIAN_POINT('Ctrl Pts',(3.93742793656346,-2.95103427388295,45.9310748895479));
#32732=CARTESIAN_POINT('Ctrl Pts',(3.84506251068321,-3.07041294065444,45.9226236895386));
#32733=CARTESIAN_POINT('Ctrl Pts',(3.70020168996147,-3.24083194870978,45.9100246764066));
#32734=CARTESIAN_POINT('Ctrl Pts',(3.65182025248989,-3.29525309312637,45.90591463613));
#32735=CARTESIAN_POINT('Ctrl Pts',(3.55381731617338,-3.40068017127785,45.8977672463934));
#32736=CARTESIAN_POINT('Ctrl Pts',(3.50426149556493,-3.45172338956551,45.8937313668823));
#32737=CARTESIAN_POINT('Ctrl Pts',(3.33925555592471,-3.61446478811092,45.8805501341912));
#32738=CARTESIAN_POINT('Ctrl Pts',(3.21943917343033,-3.72158482322258,45.871369199878));
#32739=CARTESIAN_POINT('Ctrl Pts',(2.98655140186315,-3.91011748273077,45.854217062773));
#32740=CARTESIAN_POINT('Ctrl Pts',(2.87484361366755,-3.99296666932025,45.8462576994823));
#32741=CARTESIAN_POINT('Ctrl Pts',(2.72540167993102,-4.09427568056966,45.8359816074918));
#32742=CARTESIAN_POINT('Ctrl Pts',(2.6907334647845,-4.11714235151632,45.8336226896286));
#32743=CARTESIAN_POINT('Ctrl Pts',(2.62022911982501,-4.1623750968099,45.8288776399587));
#32744=CARTESIAN_POINT('Ctrl Pts',(2.58438608307903,-4.18472409079444,45.8264918788485));
#32745=CARTESIAN_POINT('Ctrl Pts',(2.43378455237123,-4.27595476609958,45.8165662075385));
#32746=CARTESIAN_POINT('Ctrl Pts',(2.31652553851776,-4.34059979757258,45.8090722171698));
#32747=CARTESIAN_POINT('Ctrl Pts',(2.05517012920957,-4.471074611123,45.7927075363262));
#32748=CARTESIAN_POINT('Ctrl Pts',(1.91023678398102,-4.53488997572871,45.7838436410365));
#32749=CARTESIAN_POINT('Ctrl Pts',(1.69485149291074,-4.61756527383395,45.7708468930203));
#32750=CARTESIAN_POINT('Ctrl Pts',(1.62665768730089,-4.64202706256713,45.7667573187759));
#32751=CARTESIAN_POINT('Ctrl Pts',(1.49018242909036,-4.68760534848185,45.7586125550724));
#32752=CARTESIAN_POINT('Ctrl Pts',(1.42193127862445,-4.70875767643545,45.7545586366489));
#32753=CARTESIAN_POINT('Ctrl Pts',(1.31513742115687,-4.73932143739167,45.7482403036438));
#32754=CARTESIAN_POINT('Ctrl Pts',(1.27690040848821,-4.74976625173223,45.7459829888365));
#32755=CARTESIAN_POINT('Ctrl Pts',(1.05951530639952,-4.80633237304636,45.7331759636513));
#32756=CARTESIAN_POINT('Ctrl Pts',(0.87800434484672,-4.84277926103134,45.7225764625679));
#32757=CARTESIAN_POINT('Ctrl Pts',(0.615322965076392,-4.88026823936189,
45.7074016408119));
#32758=CARTESIAN_POINT('Ctrl Pts',(0.535504223934996,-4.88967032495199,
45.7028131341762));
#32759=CARTESIAN_POINT('Ctrl Pts',(0.416644779359256,-4.90072568377732,
45.6960233371103));
#32760=CARTESIAN_POINT('Ctrl Pts',(0.377757163252485,-4.9038764958753,45.6938087915722));
#32761=CARTESIAN_POINT('Ctrl Pts',(0.294426287644029,-4.90963112990521,
45.689079850044));
#32762=CARTESIAN_POINT('Ctrl Pts',(0.249976850757127,-4.91209490004657,
45.6865670378003));
#32763=CARTESIAN_POINT('Ctrl Pts',(0.149126167680454,-4.91631243814184,
45.6808805802136));
#32764=CARTESIAN_POINT('Ctrl Pts',(0.0927158106556685,-4.91769971238357,
45.6777103648157));
#32765=CARTESIAN_POINT('Ctrl Pts',(-0.118632671288443,-4.91925938131254,
45.6658500944445));
#32766=CARTESIAN_POINT('Ctrl Pts',(-0.273526647587613,-4.91308150290417,
45.6571901711359));
#32767=CARTESIAN_POINT('Ctrl Pts',(-0.531096265295244,-4.89058858306286,
45.6426806924273));
#32768=CARTESIAN_POINT('Ctrl Pts',(-0.634010610454954,-4.87831426813296,
45.6368546467032));
#32769=CARTESIAN_POINT('Ctrl Pts',(-0.798060326823833,-4.8534693248098,
45.6274900316041));
#32770=CARTESIAN_POINT('Ctrl Pts',(-0.859477973920052,-4.84297039832362,
45.6239666039346));
#32771=CARTESIAN_POINT('Ctrl Pts',(-0.997534905257617,-4.8166615502822,
45.6160004844995));
#32772=CARTESIAN_POINT('Ctrl Pts',(-1.07402957555589,-4.8001838137992,45.6115542391892));
#32773=CARTESIAN_POINT('Ctrl Pts',(-1.23980319591408,-4.7603133949289,45.6018405855674));
#32774=CARTESIAN_POINT('Ctrl Pts',(-1.32888295479029,-4.73621847495473,
45.5965706526828));
#32775=CARTESIAN_POINT('Ctrl Pts',(-1.5952954816186,-4.65604911203259,45.5806554692814));
#32776=CARTESIAN_POINT('Ctrl Pts',(-1.77017828285838,-4.59241012163614,
45.569993560613));
#32777=CARTESIAN_POINT('Ctrl Pts',(-1.97381314194537,-4.50494363580632,
45.5573868473431));
#32778=CARTESIAN_POINT('Ctrl Pts',(-2.00643472182376,-4.49050946167834,
45.5553614692509));
#32779=CARTESIAN_POINT('Ctrl Pts',(-2.0722276873717,-4.46053774599917,45.5512661881276));
#32780=CARTESIAN_POINT('Ctrl Pts',(-2.1053883419589,-4.44498195027296,45.5491966218872));
#32781=CARTESIAN_POINT('Ctrl Pts',(-2.18119156068468,-4.40838375251777,
45.5444490418963));
#32782=CARTESIAN_POINT('Ctrl Pts',(-2.2237089892051,-4.38709041637629,45.5417738555316));
#32783=CARTESIAN_POINT('Ctrl Pts',(-2.35642603836265,-4.31819868952703,
45.5333730602532));
#32784=CARTESIAN_POINT('Ctrl Pts',(-2.44545801023026,-4.26840941292869,
45.5276629591504));
#32785=CARTESIAN_POINT('Ctrl Pts',(-2.66849277034031,-4.13441159042388,
45.5130863070386));
#32786=CARTESIAN_POINT('Ctrl Pts',(-2.80009584349005,-4.04643982449125,
45.5042215704652));
#32787=CARTESIAN_POINT('Ctrl Pts',(-2.98266977194936,-3.91121769796303,
45.4914144368207));
#32788=CARTESIAN_POINT('Ctrl Pts',(-3.03724017144362,-3.86899403593224,
45.4875172119113));
#32789=CARTESIAN_POINT('Ctrl Pts',(-3.11812769450088,-3.80364137067469,
45.481628016656));
#32790=CARTESIAN_POINT('Ctrl Pts',(-3.14511586641018,-3.78135612761962,
45.4796435766889));
#32791=CARTESIAN_POINT('Ctrl Pts',(-3.24354500284124,-3.69829635506482,
45.4723322009953));
#32792=CARTESIAN_POINT('Ctrl Pts',(-3.31348057206347,-3.63577038494733,
45.4669914571636));
#32793=CARTESIAN_POINT('Ctrl Pts',(-3.47919239790801,-3.47886081016615,
45.4539633308183));
#32794=CARTESIAN_POINT('Ctrl Pts',(-3.5729694486368,-3.38247560916495,45.4462660998323));
#32795=CARTESIAN_POINT('Ctrl Pts',(-3.73071931371786,-3.20644820971547,
45.4327386917358));
#32796=CARTESIAN_POINT('Ctrl Pts',(-3.79638231995738,-3.12842745854271,
45.4269103566911));
#32797=CARTESIAN_POINT('Ctrl Pts',(-3.88478515410035,-3.01650159951331,
45.4187942619907));
#32798=CARTESIAN_POINT('Ctrl Pts',(-3.90960010995299,-2.9842695309423,45.4164842906093));
#32799=CARTESIAN_POINT('Ctrl Pts',(-3.94016573632975,-2.94353225687743,
45.4135999223398));
#32800=CARTESIAN_POINT('Ctrl Pts',(-3.94629324613586,-2.93531221395766,
45.4130196662068));
#32801=CARTESIAN_POINT('Ctrl Pts',(-3.97819155417054,-2.89224027434051,
45.4099881611807));
#32802=CARTESIAN_POINT('Ctrl Pts',(-4.00352667541658,-2.85706773806111,
45.4075431858685));
#32803=CARTESIAN_POINT('Ctrl Pts',(-4.06403028740322,-2.77068574808417,
45.4016051695881));
#32804=CARTESIAN_POINT('Ctrl Pts',(-4.09869998123625,-2.71913593828919,
45.3981173214067));
#32805=CARTESIAN_POINT('Ctrl Pts',(-4.24245398656462,-2.49639148142515,
45.3832485894215));
#32806=CARTESIAN_POINT('Ctrl Pts',(-4.34185928119416,-2.31919031614372,
45.3719111584013));
#32807=CARTESIAN_POINT('Ctrl Pts',(-4.46322210869182,-2.06752761826943,
45.3561848729021));
#32808=CARTESIAN_POINT('Ctrl Pts',(-4.49480514123492,-1.99793608595011,
45.3518746839423));
#32809=CARTESIAN_POINT('Ctrl Pts',(-4.54736991113381,-1.87455052746062,
45.3442882728012));
#32810=CARTESIAN_POINT('Ctrl Pts',(-4.56904990644319,-1.82106992082375,
45.3410179082324));
#32811=CARTESIAN_POINT('Ctrl Pts',(-4.6248079596991,-1.67625641721646,45.3322052631621));
#32812=CARTESIAN_POINT('Ctrl Pts',(-4.65711992502933,-1.58427203858187,
45.3266522593378));
#32813=CARTESIAN_POINT('Ctrl Pts',(-4.73251613712062,-1.34734014180293,
45.3124518738064));
#32814=CARTESIAN_POINT('Ctrl Pts',(-4.77168960456113,-1.20125453203193,
45.3037906890913));
#32815=CARTESIAN_POINT('Ctrl Pts',(-4.82128742319234,-0.975104243802025,
45.2905499286726));
#32816=CARTESIAN_POINT('Ctrl Pts',(-4.83657599270369,-0.89619952656837,
45.2859613501807));
#32817=CARTESIAN_POINT('Ctrl Pts',(-4.85640129066845,-0.778504932870294,
45.2791727311883));
#32818=CARTESIAN_POINT('Ctrl Pts',(-4.86242068863167,-0.739978739340114,
45.2769594213734));
#32819=CARTESIAN_POINT('Ctrl Pts',(-4.87276911943305,-0.668155141811244,
45.2728512291904));
#32820=CARTESIAN_POINT('Ctrl Pts',(-4.8772165272004,-0.63487727907879,45.2709547399077));
#32821=CARTESIAN_POINT('Ctrl Pts',(-4.9059127981702,-0.402021658618577,
45.2577235429393));
#32822=CARTESIAN_POINT('Ctrl Pts',(-4.91824524434851,-0.201164899637867,
45.246503398605));
#32823=CARTESIAN_POINT('Ctrl Pts',(-4.91824999862486,-0.000116303819701243,
45.2352292809051));
#32824=CARTESIAN_POINT('Ctrl Pts',(-4.76410171059494,1.22196554825755,45.1652160615516));
#32825=CARTESIAN_POINT('Ctrl Pts',(-4.86593327629969,0.823201249710175,
45.1885242290375));
#32826=CARTESIAN_POINT('Ctrl Pts',(-4.91771545987082,0.411493494414974,
45.2118323965233));
#32827=CARTESIAN_POINT('Ctrl Pts',(-4.91809585794598,-0.000121275114829886,
45.2351405640092));
#32828=CARTESIAN_POINT('Ctrl Pts',(-4.76403458711239,1.22194824575222,44.8197276177568));
#32829=CARTESIAN_POINT('Ctrl Pts',(-4.78147306724803,1.15396048702209,44.8236795889637));
#32830=CARTESIAN_POINT('Ctrl Pts',(-4.79745423809204,1.08560693764343,44.8276395483669));
#32831=CARTESIAN_POINT('Ctrl Pts',(-4.82621356990646,0.949522500739756,
44.835507064092));
#32832=CARTESIAN_POINT('Ctrl Pts',(-4.83904177594388,0.881819113438545,
44.8394133260436));
#32833=CARTESIAN_POINT('Ctrl Pts',(-4.88760472540874,0.592396864119301,
44.8560915905761));
#32834=CARTESIAN_POINT('Ctrl Pts',(-4.90955337029353,0.368641935581625,
44.8689486163543));
#32835=CARTESIAN_POINT('Ctrl Pts',(-4.91754602003831,0.0961080499181013,
44.8845482598853));
#32836=CARTESIAN_POINT('Ctrl Pts',(-4.91825066357339,0.0480214367964797,
44.8872977785004));
#32837=CARTESIAN_POINT('Ctrl Pts',(-4.91824915193266,-0.0614515277800697,
44.8935479337799));
#32838=CARTESIAN_POINT('Ctrl Pts',(-4.91709913051757,-0.122830297982319,
44.8970455825798));
#32839=CARTESIAN_POINT('Ctrl Pts',(-4.91341047784258,-0.221265452992939,
44.9026389389286));
#32840=CARTESIAN_POINT('Ctrl Pts',(-4.91160058697769,-0.258342098878533,
44.9047417421161));
#32841=CARTESIAN_POINT('Ctrl Pts',(-4.90569947848665,-0.356416578897101,
44.910294751197));
#32842=CARTESIAN_POINT('Ctrl Pts',(-4.90089042376304,-0.417364756830315,
44.9137371053922));
#32843=CARTESIAN_POINT('Ctrl Pts',(-4.89030397002876,-0.525727918636804,
44.919856063389));
#32844=CARTESIAN_POINT('Ctrl Pts',(-4.88496978675967,-0.573177965872096,
44.9225349406054));
#32845=CARTESIAN_POINT('Ctrl Pts',(-4.85048853898785,-0.844282686854085,
44.9378572043362));
#32846=CARTESIAN_POINT('Ctrl Pts',(-4.80667514669203,-1.06579787208497,
44.9504548561697));
#32847=CARTESIAN_POINT('Ctrl Pts',(-4.72984274491612,-1.35000509945235,
44.9670586788879));
#32848=CARTESIAN_POINT('Ctrl Pts',(-4.71047529309354,-1.41610329152046,
44.9709510725384));
#32849=CARTESIAN_POINT('Ctrl Pts',(-4.66638171085826,-1.5556569962177,44.9792437336011));
#32850=CARTESIAN_POINT('Ctrl Pts',(-4.64129448645505,-1.62897889896192,
44.9836455046313));
#32851=CARTESIAN_POINT('Ctrl Pts',(-4.58383752609168,-1.78478658035925,
44.993103171769));
#32852=CARTESIAN_POINT('Ctrl Pts',(-4.55094981229441,-1.86705254122267,
44.9981608313546));
#32853=CARTESIAN_POINT('Ctrl Pts',(-4.43965684316422,-2.12500123890288,
45.0142274204489));
#32854=CARTESIAN_POINT('Ctrl Pts',(-4.35315904673104,-2.29699591107445,
45.0252592667991));
#32855=CARTESIAN_POINT('Ctrl Pts',(-4.23635465308391,-2.49882976287675,
45.0385286882637));
#32856=CARTESIAN_POINT('Ctrl Pts',(-4.21545903316833,-2.53392109838937,
45.0408478323642));
#32857=CARTESIAN_POINT('Ctrl Pts',(-4.17108537046679,-2.60637227553136,
45.045659182157));
#32858=CARTESIAN_POINT('Ctrl Pts',(-4.14753674819023,-2.64368466175158,
45.0481503436669));
#32859=CARTESIAN_POINT('Ctrl Pts',(-4.09372132608914,-2.72646503287223,
45.053714003143));
#32860=CARTESIAN_POINT('Ctrl Pts',(-4.0631927155725,-2.7717559239983,45.0567834507257));
#32861=CARTESIAN_POINT('Ctrl Pts',(-3.95116145863184,-2.93213083132849,
45.0677636302119));
#32862=CARTESIAN_POINT('Ctrl Pts',(-3.86547246288805,-3.04420612027864,
45.0756481712745));
#32863=CARTESIAN_POINT('Ctrl Pts',(-3.70176399972585,-3.24024877220388,
45.0899715782027));
#32864=CARTESIAN_POINT('Ctrl Pts',(-3.62540139433064,-3.32546734697227,
45.0963975378458));
#32865=CARTESIAN_POINT('Ctrl Pts',(-3.49829802155035,-3.45772478439933,
45.106745162313));
#32866=CARTESIAN_POINT('Ctrl Pts',(-3.44941569582427,-3.50649125863305,
45.1106482971718));
#32867=CARTESIAN_POINT('Ctrl Pts',(-3.3420480249422,-3.60918600269272,45.1190690694249));
#32868=CARTESIAN_POINT('Ctrl Pts',(-3.28324817274271,-3.66275713458285,
45.1235887592863));
#32869=CARTESIAN_POINT('Ctrl Pts',(-3.1015997039072,-3.8203625438863,45.137290088674));
#32870=CARTESIAN_POINT('Ctrl Pts',(-2.97491976406715,-3.91981404814937,
45.1465019642358));
#32871=CARTESIAN_POINT('Ctrl Pts',(-2.75509996294093,-4.07558225388335,
45.1619234007074));
#32872=CARTESIAN_POINT('Ctrl Pts',(-2.66455543958162,-4.1353465643569,45.1681270977999));
#32873=CARTESIAN_POINT('Ctrl Pts',(-2.53556579594329,-4.21449015284746,
45.1767428586038));
#32874=CARTESIAN_POINT('Ctrl Pts',(-2.49873113073566,-4.23643292728247,
45.1791787489918));
#32875=CARTESIAN_POINT('Ctrl Pts',(-2.42538674489026,-4.27883550380349,
45.1839786375755));
#32876=CARTESIAN_POINT('Ctrl Pts',(-2.38889339339521,-4.29931651966843,
45.1863426877605));
#32877=CARTESIAN_POINT('Ctrl Pts',(-2.32931919006218,-4.33175836946534,
45.1901672043361));
#32878=CARTESIAN_POINT('Ctrl Pts',(-2.30639727224754,-4.34400622616873,
45.1916305298068));
#32879=CARTESIAN_POINT('Ctrl Pts',(-2.14570565593726,-4.42823805645539,
45.2018361203679));
#32880=CARTESIAN_POINT('Ctrl Pts',(-2.00468730842697,-4.49383739311481,
45.2105251286182));
#32881=CARTESIAN_POINT('Ctrl Pts',(-1.74399514514285,-4.60038980030157,
45.2263102457428));
#32882=CARTESIAN_POINT('Ctrl Pts',(-1.62539858494433,-4.64361758291524,
45.2333918448791));
#32883=CARTESIAN_POINT('Ctrl Pts',(-1.44504962988017,-4.70159720010369,
45.2440728013173));
#32884=CARTESIAN_POINT('Ctrl Pts',(-1.38445951213296,-4.71979410733264,
45.2476463712113));
#32885=CARTESIAN_POINT('Ctrl Pts',(-1.25271796180907,-4.75660461544544,
45.2553917219798));
#32886=CARTESIAN_POINT('Ctrl Pts',(-1.18146597885301,-4.77480132867078,
45.2595654741251));
#32887=CARTESIAN_POINT('Ctrl Pts',(-1.03160015752544,-4.80951484064551,
45.2683191855076));
#32888=CARTESIAN_POINT('Ctrl Pts',(-0.952935360993312,-4.82571713900363,
45.2728998674771));
#32889=CARTESIAN_POINT('Ctrl Pts',(-0.784055679698201,-4.85621012026275,
45.2827065869128));
#32890=CARTESIAN_POINT('Ctrl Pts',(-0.693767484465915,-4.86992881010696,
45.2879332572902));
#32891=CARTESIAN_POINT('Ctrl Pts',(-0.480772577535112,-4.89624812934193,
45.3002188192861));
#32892=CARTESIAN_POINT('Ctrl Pts',(-0.357868443759488,-4.906762551033,45.3072741196621));
#32893=CARTESIAN_POINT('Ctrl Pts',(-0.193997010645465,-4.91459139746558,
45.3166092103907));
#32894=CARTESIAN_POINT('Ctrl Pts',(-0.153272672446668,-4.916030003469,45.3189230803034));
#32895=CARTESIAN_POINT('Ctrl Pts',(-0.0682974750299268,-4.91797483546348,
45.3237364407185));
#32896=CARTESIAN_POINT('Ctrl Pts',(-0.0240481534612602,-4.91839026268566,
45.3262348282295));
#32897=CARTESIAN_POINT('Ctrl Pts',(0.0750607126872912,-4.91798318241482,
45.331819415762));
#32898=CARTESIAN_POINT('Ctrl Pts',(0.129913093959658,-4.91683997672672,
45.3349025288631));
#32899=CARTESIAN_POINT('Ctrl Pts',(0.327297973552554,-4.90942073636624,
45.3459887146251));
#32900=CARTESIAN_POINT('Ctrl Pts',(0.469560334053181,-4.89786169636462,
45.3539651252594));
#32901=CARTESIAN_POINT('Ctrl Pts',(0.724419954522954,-4.8659466958023,45.3683704476158));
#32902=CARTESIAN_POINT('Ctrl Pts',(0.837191476444289,-4.84781718668231,
45.3747855686281));
#32903=CARTESIAN_POINT('Ctrl Pts',(1.01674672871117,-4.81249875069379,45.3851099342859));
#32904=CARTESIAN_POINT('Ctrl Pts',(1.08397814171372,-4.79780255767535,45.3890006288279));
#32905=CARTESIAN_POINT('Ctrl Pts',(1.22915563487059,-4.76286066769494,45.3974649394445));
#32906=CARTESIAN_POINT('Ctrl Pts',(1.30695761432919,-4.74210152671356,45.4020409669084));
#32907=CARTESIAN_POINT('Ctrl Pts',(1.53837871150379,-4.67422562807143,45.4157832002721));
#32908=CARTESIAN_POINT('Ctrl Pts',(1.69023383771123,-4.62148276795247,45.4249788318269));
#32909=CARTESIAN_POINT('Ctrl Pts',(1.94021197405011,-4.5206874544515,45.440406653718));
#32910=CARTESIAN_POINT('Ctrl Pts',(2.03981162916243,-4.47662892002235,45.4466335932149));
#32911=CARTESIAN_POINT('Ctrl Pts',(2.17547080189338,-4.41115101470767,45.4552071992276));
#32912=CARTESIAN_POINT('Ctrl Pts',(2.21284176093993,-4.39252295204843,45.4575788890642));
#32913=CARTESIAN_POINT('Ctrl Pts',(2.28818566128753,-4.35376116652488,45.462378257421));
#32914=CARTESIAN_POINT('Ctrl Pts',(2.32614103420452,-4.33360102719604,45.4648054270167));
#32915=CARTESIAN_POINT('Ctrl Pts',(2.38757678877729,-4.29992948677457,45.4687541801362));
#32916=CARTESIAN_POINT('Ctrl Pts',(2.41121815923586,-4.28671710203116,45.470278636189));
#32917=CARTESIAN_POINT('Ctrl Pts',(2.50434035968479,-4.2336600558457,45.4763055907572));
#32918=CARTESIAN_POINT('Ctrl Pts',(2.57295291932214,-4.19231577167686,45.4807957195664));
#32919=CARTESIAN_POINT('Ctrl Pts',(2.76532995400544,-4.06989157198333,45.4935728907672));
#32920=CARTESIAN_POINT('Ctrl Pts',(2.88648683390808,-3.9848789883527,45.5018500353024));
#32921=CARTESIAN_POINT('Ctrl Pts',(3.0701713919727,-3.84321385976401,45.5148906865811));
#32922=CARTESIAN_POINT('Ctrl Pts',(3.13538891367781,-3.79019541417164,45.5196249140204));
#32923=CARTESIAN_POINT('Ctrl Pts',(3.25094911806792,-3.69122639542088,45.528222906272));
#32924=CARTESIAN_POINT('Ctrl Pts',(3.30175638848861,-3.64585066650713,45.5320806511759));
#32925=CARTESIAN_POINT('Ctrl Pts',(3.42548881726068,-3.53063753149932,45.5416796818153));
#32926=CARTESIAN_POINT('Ctrl Pts',(3.49723662300532,-3.45958243495677,45.5474303063531));
#32927=CARTESIAN_POINT('Ctrl Pts',(3.67060040491588,-3.27698440018866,45.5618104408424));
#32928=CARTESIAN_POINT('Ctrl Pts',(3.76936744070082,-3.16287888960564,45.570452604867));
#32929=CARTESIAN_POINT('Ctrl Pts',(3.91256339638757,-2.98119286481434,45.5836829904189));
#32930=CARTESIAN_POINT('Ctrl Pts',(3.96083360627183,-2.91675514774713,45.5882798741798));
#32931=CARTESIAN_POINT('Ctrl Pts',(4.02834085870301,-2.82186911917654,45.5949039482558));
#32932=CARTESIAN_POINT('Ctrl Pts',(4.04885930054713,-2.79234915496851,45.5969450939073));
#32933=CARTESIAN_POINT('Ctrl Pts',(4.09323065663019,-2.726994439585,45.6014194959053));
#32934=CARTESIAN_POINT('Ctrl Pts',(4.11694055136381,-2.69106604098175,45.6038505428661));
#32935=CARTESIAN_POINT('Ctrl Pts',(4.15483112291298,-2.63197616066168,45.6078069404788));
#32936=CARTESIAN_POINT('Ctrl Pts',(4.16929688215022,-2.60900051542786,45.6093351645887));
#32937=CARTESIAN_POINT('Ctrl Pts',(4.26500760017117,-2.4541562857412,45.6195716104849));
#32938=CARTESIAN_POINT('Ctrl Pts',(4.34017487930515,-2.31863225346499,45.6282293075763));
#32939=CARTESIAN_POINT('Ctrl Pts',(4.46334856339671,-2.06950201170173,45.6438078149792));
#32940=CARTESIAN_POINT('Ctrl Pts',(4.51371724031227,-1.95721105543012,45.6507134327288));
#32941=CARTESIAN_POINT('Ctrl Pts',(4.58350017711509,-1.78457311327604,45.6612125309867));
#32942=CARTESIAN_POINT('Ctrl Pts',(4.60604708267867,-1.72554490935836,45.6647819285775));
#32943=CARTESIAN_POINT('Ctrl Pts',(4.65240790264874,-1.59678162770063,45.6725313247727));
#32944=CARTESIAN_POINT('Ctrl Pts',(4.67580457067836,-1.52691267040807,45.6767133548468));
#32945=CARTESIAN_POINT('Ctrl Pts',(4.72149373703652,-1.37955680553916,45.6854925785876));
#32946=CARTESIAN_POINT('Ctrl Pts',(4.74346834116466,-1.30199385716819,45.690090531822));
#32947=CARTESIAN_POINT('Ctrl Pts',(4.80615380373544,-1.05802179905042,45.7044857041688));
#32948=CARTESIAN_POINT('Ctrl Pts',(4.84008449222577,-0.890003687634916,
45.7143061898907));
#32949=CARTESIAN_POINT('Ctrl Pts',(4.87421350493816,-0.65956612092834,45.7276064794889));
#32950=CARTESIAN_POINT('Ctrl Pts',(4.88209915447133,-0.59840850403533,45.7311198635342));
#32951=CARTESIAN_POINT('Ctrl Pts',(4.89288675943224,-0.500220087212699,
45.7367289499389));
#32952=CARTESIAN_POINT('Ctrl Pts',(4.89652278201866,-0.463277091424875,
45.7388318459252));
#32953=CARTESIAN_POINT('Ctrl Pts',(4.90501570200407,-0.365661572513761,
45.7443698473908));
#32954=CARTESIAN_POINT('Ctrl Pts',(4.90916519024006,-0.304933912648089,
45.7477972063098));
#32955=CARTESIAN_POINT('Ctrl Pts',(4.91453866462116,-0.196819580531643,
45.7538808705548));
#32956=CARTESIAN_POINT('Ctrl Pts',(4.91620677564324,-0.14946306025981,45.756539474544));
#32957=CARTESIAN_POINT('Ctrl Pts',(4.92189361766895,0.124445970225819,45.7719002336401));
#32958=CARTESIAN_POINT('Ctrl Pts',(4.91093653285998,0.35103376294935,45.7845554754239));
#32959=CARTESIAN_POINT('Ctrl Pts',(4.87633525461716,0.644419187943354,45.801216469747));
#32960=CARTESIAN_POINT('Ctrl Pts',(4.86683833838516,0.712605116679588,45.8051070538033));
#32961=CARTESIAN_POINT('Ctrl Pts',(4.84360078178829,0.857165824375748,45.8134033725237));
#32962=CARTESIAN_POINT('Ctrl Pts',(4.82947756941413,0.933460224990087,45.8178106482833));
#32963=CARTESIAN_POINT('Ctrl Pts',(4.7925450630197,1.10958346863074,45.8280595391863));
#32964=CARTESIAN_POINT('Ctrl Pts',(4.7684112608404,1.20909775560047,45.8339071619055));
#32965=CARTESIAN_POINT('Ctrl Pts',(4.69363257252425,1.48019723089021,45.8499966389717));
#32966=CARTESIAN_POINT('Ctrl Pts',(4.63670598893177,1.64988755801779,45.8602497912168));
#32967=CARTESIAN_POINT('Ctrl Pts',(4.55565763015683,1.85386569439065,45.8727386064233));
#32968=CARTESIAN_POINT('Ctrl Pts',(4.54018436532252,1.89144401138239,45.8750461274306));
#32969=CARTESIAN_POINT('Ctrl Pts',(4.50683097991679,1.96967756261372,45.8798621378424));
#32970=CARTESIAN_POINT('Ctrl Pts',(4.48886231822726,2.01029110656977,45.8823694520126));
#32971=CARTESIAN_POINT('Ctrl Pts',(4.44734563362257,2.1007957745788,45.8879799326976));
#32972=CARTESIAN_POINT('Ctrl Pts',(4.42350323855633,2.15054533695899,45.8910799668493));
#32973=CARTESIAN_POINT('Ctrl Pts',(4.33408973731834,2.32933420408152,45.9022991385344));
#32974=CARTESIAN_POINT('Ctrl Pts',(4.26366779019489,2.45586417089325,45.9103910202634));
#32975=CARTESIAN_POINT('Ctrl Pts',(4.13423258206288,2.66603198931017,45.9242355283345));
#32976=CARTESIAN_POINT('Ctrl Pts',(4.07800350870618,2.75127109863211,45.9299709606919));
#32977=CARTESIAN_POINT('Ctrl Pts',(3.98276619241932,2.88630288358257,45.9392878330335));
#32978=CARTESIAN_POINT('Ctrl Pts',(3.94537908589322,2.9372018384532,45.9428554071447));
#32979=CARTESIAN_POINT('Ctrl Pts',(3.86223383904292,3.04594322102908,45.9506066642937));
#32980=CARTESIAN_POINT('Ctrl Pts',(3.81613385355502,3.10350488505543,45.9547924055763));
#32981=CARTESIAN_POINT('Ctrl Pts',(3.71688262317771,3.22187605485955,45.9635830636077));
#32982=CARTESIAN_POINT('Ctrl Pts',(3.6634924841453,3.28245706514346,45.9681887564415));
#32983=CARTESIAN_POINT('Ctrl Pts',(3.49410966722076,3.46537044293843,45.9824354613477));
#32984=CARTESIAN_POINT('Ctrl Pts',(3.37330172476866,3.58307550573625,45.992098569051));
#32985=CARTESIAN_POINT('Ctrl Pts',(3.19928904300579,3.7360025212468,46.0053271329495));
#32986=CARTESIAN_POINT('Ctrl Pts',(3.15109042672226,3.77674389937413,46.0089234974014));
#32987=CARTESIAN_POINT('Ctrl Pts',(3.07330409305374,3.83996927440544,46.0146161569135));
#32988=CARTESIAN_POINT('Ctrl Pts',(3.04422297677568,3.86306466273359,46.0167201634709));
#32989=CARTESIAN_POINT('Ctrl Pts',(2.96783759724997,3.92232948639487,46.0221850312358));
#32990=CARTESIAN_POINT('Ctrl Pts',(2.92013309032495,3.95797315113337,46.0255386609284));
#32991=CARTESIAN_POINT('Ctrl Pts',(2.74281942140944,4.08550658480868,46.0378157037036));
#32992=CARTESIAN_POINT('Ctrl Pts',(2.60942651138046,4.17196791134512,46.046694222768));
#32993=CARTESIAN_POINT('Ctrl Pts',(2.37761780984614,4.30674550923241,46.0617287780626));
#32994=CARTESIAN_POINT('Ctrl Pts',(2.28134937478438,4.35850524529504,46.0678644043568));
#32995=CARTESIAN_POINT('Ctrl Pts',(2.12623389667045,4.43535658165048,46.0776224300681));
#32996=CARTESIAN_POINT('Ctrl Pts',(2.06848398677221,4.46258136903618,46.0812280333307));
#32997=CARTESIAN_POINT('Ctrl Pts',(1.94398460985409,4.518337533471,46.088950646614));
#32998=CARTESIAN_POINT('Ctrl Pts',(1.87710039746283,4.54653100302939,46.0930692070675));
#32999=CARTESIAN_POINT('Ctrl Pts',(1.67116933721871,4.62801741629052,46.1056683798968));
#33000=CARTESIAN_POINT('Ctrl Pts',(1.53030648425855,4.67648514033887,46.1141773521644));
#33001=CARTESIAN_POINT('Ctrl Pts',(1.24482303005975,4.76043111830867,46.1312104941889));
#33002=CARTESIAN_POINT('Ctrl Pts',(1.10035218850052,4.79588517080334,46.1397258550696));
#33003=CARTESIAN_POINT('Ctrl Pts',(0.914075982469187,4.83273689943749,46.150531978856));
#33004=CARTESIAN_POINT('Ctrl Pts',(0.873556017561933,4.84022528260812,46.152872071233));
#33005=CARTESIAN_POINT('Ctrl Pts',(0.800161749142142,4.85283739778018,46.1570897455529));
#33006=CARTESIAN_POINT('Ctrl Pts',(0.767320586425377,4.85813840678994,46.158969551156));
#33007=CARTESIAN_POINT('Ctrl Pts',(0.688458665127323,4.87004816219177,46.1634688761364));
#33008=CARTESIAN_POINT('Ctrl Pts',(0.64239293493654,4.87633836058237,46.1660851459559));
#33009=CARTESIAN_POINT('Ctrl Pts',(0.500571608007378,4.89365926467313,46.1741135716464));
#33010=CARTESIAN_POINT('Ctrl Pts',(0.404575224987392,4.9025291443336,46.1795116060477));
#33011=CARTESIAN_POINT('Ctrl Pts',(0.151696715111516,4.91841617697642,46.1937059351767));
#33012=CARTESIAN_POINT('Ctrl Pts',(-0.00536645851149809,4.92075197685467,
46.2024986355026));
#33013=CARTESIAN_POINT('Ctrl Pts',(-0.234024423337686,4.9132036235554,46.2153867872758));
#33014=CARTESIAN_POINT('Ctrl Pts',(-0.305717154346934,4.90926411420714,
46.2194397057122));
#33015=CARTESIAN_POINT('Ctrl Pts',(-0.440949467733291,4.89885927575076,
46.227116910916));
#33016=CARTESIAN_POINT('Ctrl Pts',(-0.504499709232383,4.89272302161677,
46.2307381972687));
#33017=CARTESIAN_POINT('Ctrl Pts',(-0.640936127073086,4.87686256991019,
46.2385468276733));
#33018=CARTESIAN_POINT('Ctrl Pts',(-0.713760196841688,4.86673749824665,
46.2427358358964));
#33019=CARTESIAN_POINT('Ctrl Pts',(-0.921122730406577,4.83315237106078,
46.2547286568073));
#33020=CARTESIAN_POINT('Ctrl Pts',(-1.05494785602666,4.80571676176551,46.262548459722));
#33021=CARTESIAN_POINT('Ctrl Pts',(-1.28355799641268,4.74883870666813,46.2760300861809));
#33022=CARTESIAN_POINT('Ctrl Pts',(-1.37891600958028,4.7220314666776,46.281690961334));
#33023=CARTESIAN_POINT('Ctrl Pts',(-1.51247704811039,4.68009335263922,46.289657048049));
#33024=CARTESIAN_POINT('Ctrl Pts',(-1.55139937187478,4.66733549915466,46.2919829932017));
#33025=CARTESIAN_POINT('Ctrl Pts',(-1.62172062730431,4.64330892283432,46.2961914964924));
#33026=CARTESIAN_POINT('Ctrl Pts',(-1.65317279934575,4.63220414806112,46.2980762050619));
#33027=CARTESIAN_POINT('Ctrl Pts',(-1.72850363467977,4.60474222141809,46.3025992078367));
#33028=CARTESIAN_POINT('Ctrl Pts',(-1.77226649997432,4.58807663937436,46.3052341896939));
#33029=CARTESIAN_POINT('Ctrl Pts',(-1.90678503063754,4.53463799956344,46.313367181336));
#33030=CARTESIAN_POINT('Ctrl Pts',(-1.99668569373937,4.49577772737781,46.3188506841471));
#33031=CARTESIAN_POINT('Ctrl Pts',(-2.22479790096022,4.38898161815378,46.332960827835));
#33032=CARTESIAN_POINT('Ctrl Pts',(-2.36108582819033,4.31719333819467,46.3415843953433));
#33033=CARTESIAN_POINT('Ctrl Pts',(-2.55579287632227,4.20265179746592,46.3543096493054));
#33034=CARTESIAN_POINT('Ctrl Pts',(-2.61699645376738,4.16481557356469,46.3583710833446));
#33035=CARTESIAN_POINT('Ctrl Pts',(-2.73093110491114,4.0908775022895,46.366058860214));
#33036=CARTESIAN_POINT('Ctrl Pts',(-2.78383178685674,4.05506398308684,46.369682164309));
#33037=CARTESIAN_POINT('Ctrl Pts',(-2.89594346897092,3.97593688581185,46.377483053367));
#33038=CARTESIAN_POINT('Ctrl Pts',(-2.95491341700867,3.93230838627995,46.3816622509292));
#33039=CARTESIAN_POINT('Ctrl Pts',(-3.12004082878083,3.80432753147657,46.3935891831376));
#33040=CARTESIAN_POINT('Ctrl Pts',(-3.22371628748125,3.71688252225012,46.4013526723324));
#33041=CARTESIAN_POINT('Ctrl Pts',(-3.39813335670504,3.55697690137453,46.4148945207923));
#33042=CARTESIAN_POINT('Ctrl Pts',(-3.47049909523308,3.4864066567695,46.4206713908966));
#33043=CARTESIAN_POINT('Ctrl Pts',(-3.56896221032236,3.38428085408461,46.4287435889162));
#33044=CARTESIAN_POINT('Ctrl Pts',(-3.59691811318429,3.35455336935347,46.4310607812354));
#33045=CARTESIAN_POINT('Ctrl Pts',(-3.64708576399759,3.29985830680953,46.4352637811368));
#33046=CARTESIAN_POINT('Ctrl Pts',(-3.66941909082484,3.27500579829361,46.4371516928107));
#33047=CARTESIAN_POINT('Ctrl Pts',(-3.7225833251807,3.21461809975419,46.4416900609624));
#33048=CARTESIAN_POINT('Ctrl Pts',(-3.75316107328171,3.17886428675401,46.4443371644146));
#33049=CARTESIAN_POINT('Ctrl Pts',(-3.84643118164115,3.06658375184157,46.4525385286616));
#33050=CARTESIAN_POINT('Ctrl Pts',(-3.90733120635388,2.98860030472879,46.4580780285142));
#33051=CARTESIAN_POINT('Ctrl Pts',(-4.05574806752662,2.78625206504129,46.4721360378995));
#33052=CARTESIAN_POINT('Ctrl Pts',(-4.13992539438346,2.65956950794021,46.4806517584734));
#33053=CARTESIAN_POINT('Ctrl Pts',(-4.25514462496286,2.46741092487962,46.4932727921975));
#33054=CARTESIAN_POINT('Ctrl Pts',(-4.2908274658301,2.40482264480861,46.4973392684591));
#33055=CARTESIAN_POINT('Ctrl Pts',(-4.35554409044418,2.2852794172165,46.5050333304892));
#33056=CARTESIAN_POINT('Ctrl Pts',(-4.38486748948721,2.22849799730318,46.5086578548998));
#33057=CARTESIAN_POINT('Ctrl Pts',(-4.44541123581498,2.10543754354329,46.5164543251374));
#33058=CARTESIAN_POINT('Ctrl Pts',(-4.476273967928,2.03899963735559,46.5206278535098));
#33059=CARTESIAN_POINT('Ctrl Pts',(-4.5597712063157,1.84821459636023,46.5325168921725));
#33060=CARTESIAN_POINT('Ctrl Pts',(-4.60878526973432,1.72235554743886,46.5402480220065));
#33061=CARTESIAN_POINT('Ctrl Pts',(-4.68552732309619,1.49845122849291,46.5537938975573));
#33062=CARTESIAN_POINT('Ctrl Pts',(-4.7155051100487,1.40126168137821,46.5596069261676));
#33063=CARTESIAN_POINT('Ctrl Pts',(-4.74987553743386,1.27618611588959,46.5669880081433));
#33064=CARTESIAN_POINT('Ctrl Pts',(-4.75707104127008,1.24909716417162,46.5685806726222));
#33065=CARTESIAN_POINT('Ctrl Pts',(-4.7640345870679,1.22194824592564,46.5701705954582));
#33066=CARTESIAN_POINT('Origin',(0.,0.,-3.23514056400928));
#33067=CARTESIAN_POINT('',(-4.76403458580012,1.22194825086837,48.6654127926075));
#33068=CARTESIAN_POINT('',(-4.76366299354682,1.22185269443844,48.3199247396258));
#33069=CARTESIAN_POINT('',(-4.76403458704967,1.22194824599672,-3.23514056400928));
#33070=CARTESIAN_POINT('Ctrl Pts',(-4.76403458580012,1.22194825086837,48.6654127926075));
#33071=CARTESIAN_POINT('Ctrl Pts',(-4.75303754389474,1.26482264259609,48.6628924344214));
#33072=CARTESIAN_POINT('Ctrl Pts',(-4.74146170699504,1.30754864644256,48.6603686712803));
#33073=CARTESIAN_POINT('Ctrl Pts',(-4.6642949204399,1.5778558275802,48.6443229989067));
#33074=CARTESIAN_POINT('Ctrl Pts',(-4.58291454291531,1.80060275079479,48.6307254558902));
#33075=CARTESIAN_POINT('Ctrl Pts',(-4.46932232969459,2.05327950110843,48.6149576556254));
#33076=CARTESIAN_POINT('Ctrl Pts',(-4.45239183251398,2.08973821655184,48.6126743042949));
#33077=CARTESIAN_POINT('Ctrl Pts',(-4.41707807004089,2.16340621913512,48.608045903262));
#33078=CARTESIAN_POINT('Ctrl Pts',(-4.39866693276733,2.20059864818217,48.6057014917757));
#33079=CARTESIAN_POINT('Ctrl Pts',(-4.31628671382158,2.36184966075428,48.5954922648057));
#33080=CARTESIAN_POINT('Ctrl Pts',(-4.24752314980106,2.4833873582621,48.587678779137));
#33081=CARTESIAN_POINT('Ctrl Pts',(-4.1146351352696,2.69655694146925,48.5736062541915));
#33082=CARTESIAN_POINT('Ctrl Pts',(-4.05238031777689,2.7892391736651,48.5673538816942));
#33083=CARTESIAN_POINT('Ctrl Pts',(-3.93628663267689,2.94997292719581,48.5562110966866));
#33084=CARTESIAN_POINT('Ctrl Pts',(-3.88369927891628,3.01886938925748,48.5513309266917));
#33085=CARTESIAN_POINT('Ctrl Pts',(-3.81163004673214,3.10828796741809,48.5448426748559));
#33086=CARTESIAN_POINT('Ctrl Pts',(-3.79375213020502,3.13008345995897,48.5432486240844));
#33087=CARTESIAN_POINT('Ctrl Pts',(-3.73546804546558,3.1999063612482,48.538100321165));
#33088=CARTESIAN_POINT('Ctrl Pts',(-3.69432988336773,3.24731409694626,48.5345401929561));
#33089=CARTESIAN_POINT('Ctrl Pts',(-3.56936625662945,3.385873621345,48.5239332958891));
#33090=CARTESIAN_POINT('Ctrl Pts',(-3.48299441442204,3.47466040436883,48.5168669703973));
#33091=CARTESIAN_POINT('Ctrl Pts',(-3.30086857688185,3.64825689531583,48.502475260776));
#33092=CARTESIAN_POINT('Ctrl Pts',(-3.20497104389534,3.73278346399049,48.4951541685068));
#33093=CARTESIAN_POINT('Ctrl Pts',(-3.0652842607331,3.84655145807064,48.4848591277372));
#33094=CARTESIAN_POINT('Ctrl Pts',(-3.02415178075368,3.87897303298115,48.4818703976402));
#33095=CARTESIAN_POINT('Ctrl Pts',(-2.97239359215439,3.91844627820362,48.4781643582133));
#33096=CARTESIAN_POINT('Ctrl Pts',(-2.96224812801155,3.92612161442486,48.4774404833506));
#33097=CARTESIAN_POINT('Ctrl Pts',(-2.92272183294512,3.95578396832812,48.474630372241));
#33098=CARTESIAN_POINT('Ctrl Pts',(-2.89312481939677,3.97748143284406,48.4725477342435));
#33099=CARTESIAN_POINT('Ctrl Pts',(-2.82621348676924,4.02539185159751,48.4678888505519));
#33100=CARTESIAN_POINT('Ctrl Pts',(-2.78877184680265,4.05142121789256,48.4653152037406));
#33101=CARTESIAN_POINT('Ctrl Pts',(-2.58817034026317,4.18678039714364,48.4516838354521));
#33102=CARTESIAN_POINT('Ctrl Pts',(-2.41893191871587,4.28678499770639,48.4407220192644));
#33103=CARTESIAN_POINT('Ctrl Pts',(-2.17135187563102,4.41374107318464,48.4251157639514));
#33104=CARTESIAN_POINT('Ctrl Pts',(-2.09761701939299,4.44925633162107,48.4205199426548));
#33105=CARTESIAN_POINT('Ctrl Pts',(-1.96386414320659,4.50961576188982,48.4122563520596));
#33106=CARTESIAN_POINT('Ctrl Pts',(-1.90417495083866,4.53514215172833,48.408594016453));
#33107=CARTESIAN_POINT('Ctrl Pts',(-1.78176302313206,4.58464942672549,48.4011264682826));
#33108=CARTESIAN_POINT('Ctrl Pts',(-1.71901927760205,4.6085423321158,48.3973214322091));
#33109=CARTESIAN_POINT('Ctrl Pts',(-1.54639272399786,4.67026277032317,48.3869057516458));
#33110=CARTESIAN_POINT('Ctrl Pts',(-1.43562806269652,4.70549214286965,48.3802796869801));
#33111=CARTESIAN_POINT('Ctrl Pts',(-1.1891168777845,4.77438136079565,48.3656467942903));
#33112=CARTESIAN_POINT('Ctrl Pts',(-1.05297062617578,4.80624272507219,48.3576384230074));
#33113=CARTESIAN_POINT('Ctrl Pts',(-0.862331998949356,4.8423663412981,48.3465481135928));
#33114=CARTESIAN_POINT('Ctrl Pts',(-0.808847239355958,4.85158679943994,
48.343450234862));
#33115=CARTESIAN_POINT('Ctrl Pts',(-0.750515640683471,4.86065139734147,
48.3400885263398));
#33116=CARTESIAN_POINT('Ctrl Pts',(-0.745809651932119,4.86137569999868,
48.3398174351423));
#33117=CARTESIAN_POINT('Ctrl Pts',(-0.737053794662226,4.86271030805719,
48.3393132743604));
#33118=CARTESIAN_POINT('Ctrl Pts',(-0.733004201968457,4.86332239073774,
48.3390801891424));
#33119=CARTESIAN_POINT('Ctrl Pts',(-0.725392381982326,4.86446316910591,
48.3386422406758));
#33120=CARTESIAN_POINT('Ctrl Pts',(-0.721830329842567,4.86499301195546,
48.3384373669482));
#33121=CARTESIAN_POINT('Ctrl Pts',(-0.686263474119796,4.87024353586656,
48.336392422659));
#33122=CARTESIAN_POINT('Ctrl Pts',(-0.654213216469832,4.87465226937502,
48.3345553714382));
#33123=CARTESIAN_POINT('Ctrl Pts',(-0.58211396174379,4.88384613156159,48.330436817779));
#33124=CARTESIAN_POINT('Ctrl Pts',(-0.542044820161591,4.8884554979055,48.3281577666747));
#33125=CARTESIAN_POINT('Ctrl Pts',(-0.399496136925092,4.9030794032398,48.3200765610388));
#33126=CARTESIAN_POINT('Ctrl Pts',(-0.296763194101059,4.91036829958464,
48.3143009176158));
#33127=CARTESIAN_POINT('Ctrl Pts',(-0.0600540263897964,4.91970658415861,
48.3010241931034));
#33128=CARTESIAN_POINT('Ctrl Pts',(0.0739277198397528,4.91951764794321,
48.2935313154881));
#33129=CARTESIAN_POINT('Ctrl Pts',(0.280398341796046,4.91078907786969,48.2819269053482));
#33130=CARTESIAN_POINT('Ctrl Pts',(0.352985059510516,4.90610578889122,48.2778365879361));
#33131=CARTESIAN_POINT('Ctrl Pts',(0.481394691086985,4.89495624746205,48.2705695095219));
#33132=CARTESIAN_POINT('Ctrl Pts',(0.537260985603083,4.88913980890141,48.2673974260488));
#33133=CARTESIAN_POINT('Ctrl Pts',(0.6067623182586,4.88069813929903,48.2634351632392));
#33134=CARTESIAN_POINT('Ctrl Pts',(0.620502446742907,4.87897033709223,48.262651062411));
#33135=CARTESIAN_POINT('Ctrl Pts',(0.64136944592651,4.87625676686008,48.2614590300712));
#33136=CARTESIAN_POINT('Ctrl Pts',(0.648501768587642,4.87531335182571,48.2610513765754));
#33137=CARTESIAN_POINT('Ctrl Pts',(0.661435319590417,4.87357370606498,48.2603117472468));
#33138=CARTESIAN_POINT('Ctrl Pts',(0.667237246958959,4.87278275799693,48.2599798062885));
#33139=CARTESIAN_POINT('Ctrl Pts',(0.754304513682832,4.8607548885599,48.2549962632995));
#33140=CARTESIAN_POINT('Ctrl Pts',(0.835276931303859,4.84749683903627,48.2503320819304));
#33141=CARTESIAN_POINT('Ctrl Pts',(1.04662543163158,4.80743871304497,48.2380710341535));
#33142=CARTESIAN_POINT('Ctrl Pts',(1.1763111593641,4.77736154029793,48.230458737242));
#33143=CARTESIAN_POINT('Ctrl Pts',(1.42998068659116,4.70757305959692,48.2153979006798));
#33144=CARTESIAN_POINT('Ctrl Pts',(1.5539292727806,4.66812523867936,48.2079555835195));
#33145=CARTESIAN_POINT('Ctrl Pts',(1.71546723190841,4.60956640886055,48.1981751634847));
#33146=CARTESIAN_POINT('Ctrl Pts',(1.75458190978384,4.59482020077466,48.1958006552776));
#33147=CARTESIAN_POINT('Ctrl Pts',(1.82704982883147,4.56643952044413,48.1913918016926));
#33148=CARTESIAN_POINT('Ctrl Pts',(1.8604503941377,4.55293370666031,48.1893559053022));
#33149=CARTESIAN_POINT('Ctrl Pts',(2.04489923213447,4.47598152621719,48.1780823379656));
#33150=CARTESIAN_POINT('Ctrl Pts',(2.19285423533883,4.40538478572691,48.1689211344716));
#33151=CARTESIAN_POINT('Ctrl Pts',(2.45843468403153,4.2619626263181,48.1520098539088));
#33152=CARTESIAN_POINT('Ctrl Pts',(2.57704349331808,4.19130919054859,48.1442732035657));
#33153=CARTESIAN_POINT('Ctrl Pts',(2.75253858464446,4.07650067528572,48.132456942591));
#33154=CARTESIAN_POINT('Ctrl Pts',(2.8116875800779,4.03593102166855,48.1284074160317));
#33155=CARTESIAN_POINT('Ctrl Pts',(2.9213405831657,3.95714041618647,48.1207629412454));
#33156=CARTESIAN_POINT('Ctrl Pts',(2.9720348988324,3.91920904338425,48.1171710961738));
#33157=CARTESIAN_POINT('Ctrl Pts',(3.17553927009412,3.76071999014652,48.102504903297));
#33158=CARTESIAN_POINT('Ctrl Pts',(3.32186002951284,3.632121765171,48.0913699268091));
#33159=CARTESIAN_POINT('Ctrl Pts',(3.51668074889294,3.43925313872698,48.0756785460131));
#33160=CARTESIAN_POINT('Ctrl Pts',(3.57182382760129,3.38194918804823,48.0711298591407));
#33161=CARTESIAN_POINT('Ctrl Pts',(3.64373552795213,3.30349791769414,48.065057587666));
#33162=CARTESIAN_POINT('Ctrl Pts',(3.66175447186355,3.28351355835378,48.0635237535942));
#33163=CARTESIAN_POINT('Ctrl Pts',(3.70793661102508,3.23144114360145,48.0595611483295));
#33164=CARTESIAN_POINT('Ctrl Pts',(3.73584777409445,3.19913226373311,48.0571353877461));
#33165=CARTESIAN_POINT('Ctrl Pts',(3.78981022463852,3.13499801644038,48.0523864005284));
#33166=CARTESIAN_POINT('Ctrl Pts',(3.8158900242568,3.10320116501748,48.0500629835909));
#33167=CARTESIAN_POINT('Ctrl Pts',(3.9753005955451,2.90379691050782,48.0356679482412));
#33168=CARTESIAN_POINT('Ctrl Pts',(4.09796491273494,2.7279547252578,48.0237231670548));
#33169=CARTESIAN_POINT('Ctrl Pts',(4.24985461810598,2.47673615945525,48.0072528160032));
#33170=CARTESIAN_POINT('Ctrl Pts',(4.28928064730019,2.4078117972733,48.0027924499705));
#33171=CARTESIAN_POINT('Ctrl Pts',(4.36163080785308,2.27390867707941,47.9942191983198));
#33172=CARTESIAN_POINT('Ctrl Pts',(4.39481397379133,2.20909346782165,47.9901092684121));
#33173=CARTESIAN_POINT('Ctrl Pts',(4.45754972226028,2.07954175005782,47.9819618793521));
#33174=CARTESIAN_POINT('Ctrl Pts',(4.4871607051686,2.01485286459132,47.9779258890107));
#33175=CARTESIAN_POINT('Ctrl Pts',(4.58985476581203,1.77700227111699,47.9631910844896));
#33176=CARTESIAN_POINT('Ctrl Pts',(4.65439960562896,1.60033322789052,47.9524392017229));
#33177=CARTESIAN_POINT('Ctrl Pts',(4.73202577667529,1.34300116146957,47.9370539730218));
#33178=CARTESIAN_POINT('Ctrl Pts',(4.7534638685057,1.26503021618401,47.9324284489329));
#33179=CARTESIAN_POINT('Ctrl Pts',(4.77952911296729,1.16018258193309,47.9262635610203));
#33180=CARTESIAN_POINT('Ctrl Pts',(4.78586920606005,1.13374517334062,47.9247137333008));
#33181=CARTESIAN_POINT('Ctrl Pts',(4.80166596832494,1.06537987070928,47.9207186763261));
#33182=CARTESIAN_POINT('Ctrl Pts',(4.81079287292074,1.02337790240683,47.9182764657055));
#33183=CARTESIAN_POINT('Ctrl Pts',(4.82641953903688,0.94662908029733,47.9138384416466));
#33184=CARTESIAN_POINT('Ctrl Pts',(4.83309748216093,0.911921563760926,47.9118406586812));
#33185=CARTESIAN_POINT('Ctrl Pts',(4.85347192577036,0.799511289832573,47.9053948598819));
#33186=CARTESIAN_POINT('Ctrl Pts',(4.86567307431019,0.721549583718809,47.9009620806211));
#33187=CARTESIAN_POINT('Ctrl Pts',(4.89593234926585,0.492204455999454,47.8879847305294));
#33188=CARTESIAN_POINT('Ctrl Pts',(4.90883470072782,0.34023624816981,47.879463315341));
#33189=CARTESIAN_POINT('Ctrl Pts',(4.91852211739972,0.0868748200415349,
47.8652321187964));
#33190=CARTESIAN_POINT('Ctrl Pts',(4.91926858074732,-0.0142592399419988,
47.8595457113945));
#33191=CARTESIAN_POINT('Ctrl Pts',(4.91531335454737,-0.182863935874622,
47.8500258182428));
#33192=CARTESIAN_POINT('Ctrl Pts',(4.91233877781006,-0.250344142856869,
47.846205177139));
#33193=CARTESIAN_POINT('Ctrl Pts',(4.90256575788774,-0.401302687876723,
47.837626502624));
#33194=CARTESIAN_POINT('Ctrl Pts',(4.89502290207981,-0.484711670499982,
47.8328647172573));
#33195=CARTESIAN_POINT('Ctrl Pts',(4.86452766185561,-0.747052866051986,
47.8178073628029));
#33196=CARTESIAN_POINT('Ctrl Pts',(4.83386061011668,-0.924936762342858,
47.8074740292203));
#33197=CARTESIAN_POINT('Ctrl Pts',(4.78353618054063,-1.1440908347425,47.794612060784));
#33198=CARTESIAN_POINT('Ctrl Pts',(4.77299167587137,-1.18731323513527,47.7920692481349));
#33199=CARTESIAN_POINT('Ctrl Pts',(4.74721779457032,-1.28706371613804,47.7861888479533));
#33200=CARTESIAN_POINT('Ctrl Pts',(4.73156256312988,-1.34347520497131,47.7828543092827));
#33201=CARTESIAN_POINT('Ctrl Pts',(4.70444145324473,-1.43483984963031,47.7774435781429));
#33202=CARTESIAN_POINT('Ctrl Pts',(4.69358409291108,-1.46996706811822,47.7753612148406));
#33203=CARTESIAN_POINT('Ctrl Pts',(4.66327426867004,-1.56426844229901,47.7697636854469));
#33204=CARTESIAN_POINT('Ctrl Pts',(4.64308987378551,-1.62320030460303,47.7662568963771));
#33205=CARTESIAN_POINT('Ctrl Pts',(4.56235645420327,-1.84507437534824,47.7529897459448));
#33206=CARTESIAN_POINT('Ctrl Pts',(4.49430402249567,-2.00515029816352,47.7432806749226));
#33207=CARTESIAN_POINT('Ctrl Pts',(4.38328656983293,-2.2320827424771,47.7291059923235));
#33208=CARTESIAN_POINT('Ctrl Pts',(4.34695641970232,-2.30203480719245,47.7246778532811));
#33209=CARTESIAN_POINT('Ctrl Pts',(4.27399531316522,-2.43462677535857,47.7161523846378));
#33210=CARTESIAN_POINT('Ctrl Pts',(4.23762827201911,-2.49738862415717,47.7120579047293));
#33211=CARTESIAN_POINT('Ctrl Pts',(4.16721354162531,-2.61294024875061,47.7043983415211));
#33212=CARTESIAN_POINT('Ctrl Pts',(4.133516656118,-2.66592674138782,47.7008367356476));
#33213=CARTESIAN_POINT('Ctrl Pts',(4.03007693956113,-2.82190199976728,47.690197289983));
#33214=CARTESIAN_POINT('Ctrl Pts',(3.95743303831563,-2.9229050853989,47.683099666067));
#33215=CARTESIAN_POINT('Ctrl Pts',(3.78670043297433,-3.14223981312442,47.6672006945333));
#33216=CARTESIAN_POINT('Ctrl Pts',(3.68673563025272,-3.25894950128983,47.65839839722));
#33217=CARTESIAN_POINT('Ctrl Pts',(3.56316523770292,-3.39024338074211,47.6481114343637));
#33218=CARTESIAN_POINT('Ctrl Pts',(3.54469828562453,-3.40954700302093,47.6465887288417));
#33219=CARTESIAN_POINT('Ctrl Pts',(3.49645136405402,-3.45916414534776,47.6426487413427));
#33220=CARTESIAN_POINT('Ctrl Pts',(3.46643400080861,-3.48924405841904,47.64023446429));
#33221=CARTESIAN_POINT('Ctrl Pts',(3.40648358352317,-3.54778212904583,47.6354871483765));
#33222=CARTESIAN_POINT('Ctrl Pts',(3.37657437468378,-3.57625977524213,47.6331540119713));
#33223=CARTESIAN_POINT('Ctrl Pts',(3.24135203266903,-3.70180110992867,47.622750328646));
#33224=CARTESIAN_POINT('Ctrl Pts',(3.13218679708534,-3.79461476924618,47.6147343540386));
#33225=CARTESIAN_POINT('Ctrl Pts',(2.89679303577249,-3.97766111285555,47.5980292700516));
#33226=CARTESIAN_POINT('Ctrl Pts',(2.77003357136678,-4.0669535342024,47.5893475961262));
#33227=CARTESIAN_POINT('Ctrl Pts',(2.57886482687568,-4.18852766879431,47.576582091614));
#33228=CARTESIAN_POINT('Ctrl Pts',(2.51762692349932,-4.22561975885131,47.5725397445375));
#33229=CARTESIAN_POINT('Ctrl Pts',(2.39297341365977,-4.29745111162775,47.5643943211198));
#33230=CARTESIAN_POINT('Ctrl Pts',(2.32955763837787,-4.33215522126321,47.5602920254007));
#33231=CARTESIAN_POINT('Ctrl Pts',(2.11722984382941,-4.4423403438575,47.5466822876123));
#33232=CARTESIAN_POINT('Ctrl Pts',(1.96524204965621,-4.51163743901042,47.5371363871577));
#33233=CARTESIAN_POINT('Ctrl Pts',(1.72599907859158,-4.60633012185658,47.5224071868318));
#33234=CARTESIAN_POINT('Ctrl Pts',(1.64106937830969,-4.63726659179377,47.5172346760096));
#33235=CARTESIAN_POINT('Ctrl Pts',(1.49836072064465,-4.68483777982797,47.508647291654));
#33236=CARTESIAN_POINT('Ctrl Pts',(1.4410425100728,-4.7027849706762,47.5052256583635));
#33237=CARTESIAN_POINT('Ctrl Pts',(1.34814514675965,-4.73001460341539,47.4997290512453));
#33238=CARTESIAN_POINT('Ctrl Pts',(1.31276596276615,-4.73995559599478,47.4976473721149));
#33239=CARTESIAN_POINT('Ctrl Pts',(1.21873704019795,-4.76524270245113,47.4921442587624));
#33240=CARTESIAN_POINT('Ctrl Pts',(1.15990925898567,-4.77990257526431,47.4887305535973));
#33241=CARTESIAN_POINT('Ctrl Pts',(0.929494315149827,-4.83281757634785,
47.4754437350207));
#33242=CARTESIAN_POINT('Ctrl Pts',(0.756176683350233,-4.86295000914482,
47.465625189658));
#33243=CARTESIAN_POINT('Ctrl Pts',(0.503103990241899,-4.89308913848179,
47.4513258755639));
#33244=CARTESIAN_POINT('Ctrl Pts',(0.42437644322709,-4.90054480863743,47.4468835114652));
#33245=CARTESIAN_POINT('Ctrl Pts',(0.273031839978224,-4.91120300227536,
47.4383369583662));
#33246=CARTESIAN_POINT('Ctrl Pts',(0.200456141789944,-4.91470024410186,
47.434235665806));
#33247=CARTESIAN_POINT('Ctrl Pts',(0.0651328152686634,-4.91821862052928,
47.426573296535));
#33248=CARTESIAN_POINT('Ctrl Pts',(0.00241042781142184,-4.9186492825689,
47.4230157519239));
#33249=CARTESIAN_POINT('Ctrl Pts',(-0.186097200726497,-4.91633782000799,
47.4122990793651));
#33250=CARTESIAN_POINT('Ctrl Pts',(-0.311784935807075,-4.90996937023799,
47.4051194869341));
#33251=CARTESIAN_POINT('Ctrl Pts',(-0.589663021321053,-4.88517603174792,
47.3891611670502));
#33252=CARTESIAN_POINT('Ctrl Pts',(-0.741518491739819,-4.86444220063292,
47.3803821241481));
#33253=CARTESIAN_POINT('Ctrl Pts',(-0.94629052197749,-4.82667041349628,
47.3685022456834));
#33254=CARTESIAN_POINT('Ctrl Pts',(-1.00025149998599,-4.81577720316449,
47.3653680582164));
#33255=CARTESIAN_POINT('Ctrl Pts',(-1.09009215122276,-4.79606569015607,
47.3601478672556));
#33256=CARTESIAN_POINT('Ctrl Pts',(-1.12607529254975,-4.78774492534716,
47.3580569241787));
#33257=CARTESIAN_POINT('Ctrl Pts',(-1.22530216223133,-4.7636190918068,47.3522880574088));
#33258=CARTESIAN_POINT('Ctrl Pts',(-1.28833070625862,-4.7469607526224,47.3486195796319));
#33259=CARTESIAN_POINT('Ctrl Pts',(-1.44937972124869,-4.70095180164654,
47.3392113475052));
#33260=CARTESIAN_POINT('Ctrl Pts',(-1.54684908956789,-4.66978666546042,
47.333483619902));
#33261=CARTESIAN_POINT('Ctrl Pts',(-1.78061095577791,-4.58692039981277,
47.3195889336479));
#33262=CARTESIAN_POINT('Ctrl Pts',(-1.91571347933162,-4.53215790936684,
47.3114236486186));
#33263=CARTESIAN_POINT('Ctrl Pts',(-2.11388373748844,-4.44138499816671,
47.2991438858045));
#33264=CARTESIAN_POINT('Ctrl Pts',(-2.17891160660056,-4.40984684646401,
47.2950640704293));
#33265=CARTESIAN_POINT('Ctrl Pts',(-2.30694319855285,-4.34422873869995,
47.2869199893593));
#33266=CARTESIAN_POINT('Ctrl Pts',(-2.36994462660249,-4.3101824280194,47.2828568972153));
#33267=CARTESIAN_POINT('Ctrl Pts',(-2.58484756171685,-4.18791100942648,
47.2687925096789));
#33268=CARTESIAN_POINT('Ctrl Pts',(-2.73275081375529,-4.0929337997907,47.2587468117316));
#33269=CARTESIAN_POINT('Ctrl Pts',(-2.94571173711156,-3.93948058655288,
47.2437208855272));
#33270=CARTESIAN_POINT('Ctrl Pts',(-3.01481278215812,-3.88685334847058,
47.2387510416746));
#33271=CARTESIAN_POINT('Ctrl Pts',(-3.12823159189639,-3.79562865324191,
47.2304431938363));
#33272=CARTESIAN_POINT('Ctrl Pts',(-3.1733167350476,-3.75801686829642,47.2270988870086));
#33273=CARTESIAN_POINT('Ctrl Pts',(-3.24552095616936,-3.69555520318063,
47.2216785996092));
#33274=CARTESIAN_POINT('Ctrl Pts',(-3.27305333608773,-3.67119278076716,
47.2195963883072));
#33275=CARTESIAN_POINT('Ctrl Pts',(-3.34634430804191,-3.60486030139422,
47.2140101632542));
#33276=CARTESIAN_POINT('Ctrl Pts',(-3.39158562006607,-3.56232861226026,
47.2105144490869));
#33277=CARTESIAN_POINT('Ctrl Pts',(-3.5588455171225,-3.39901102313036,47.1973782663349));
#33278=CARTESIAN_POINT('Ctrl Pts',(-3.67531719541145,-3.27272078917271,
47.1877879220347));
#33279=CARTESIAN_POINT('Ctrl Pts',(-3.83581011916303,-3.07929999369034,
47.1736872977697));
#33280=CARTESIAN_POINT('Ctrl Pts',(-3.88517660059196,-3.01677482529704,
47.1692124523823));
#33281=CARTESIAN_POINT('Ctrl Pts',(-3.97679368312251,-2.89475633526866,
47.1606177250242));
#33282=CARTESIAN_POINT('Ctrl Pts',(-4.01928179313411,-2.83546749998651,
47.1565008465802));
#33283=CARTESIAN_POINT('Ctrl Pts',(-4.10051938974657,-2.71661000251498,
47.1483522454192));
#33284=CARTESIAN_POINT('Ctrl Pts',(-4.13932776346384,-2.65710268562874,
47.1443220575799));
#33285=CARTESIAN_POINT('Ctrl Pts',(-4.28959196379171,-2.4154074170201,47.1281360324337));
#33286=CARTESIAN_POINT('Ctrl Pts',(-4.39041649763644,-2.22688861774463,
47.1159074473785));
#33287=CARTESIAN_POINT('Ctrl Pts',(-4.49839469111282,-1.98894626880638,
47.1009579096944));
#33288=CARTESIAN_POINT('Ctrl Pts',(-4.51748837025478,-1.94518917148043,
47.0982285042523));
#33289=CARTESIAN_POINT('Ctrl Pts',(-4.55952006317209,-1.84490659050137,
47.0920206470637));
#33290=CARTESIAN_POINT('Ctrl Pts',(-4.58204975855493,-1.78821801594125,
47.0885451537726));
#33291=CARTESIAN_POINT('Ctrl Pts',(-4.6164545839381,-1.69672646292976,47.0829947330628));
#33292=CARTESIAN_POINT('Ctrl Pts',(-4.62900386931649,-1.66218435635961,
47.0809127692859));
#33293=CARTESIAN_POINT('Ctrl Pts',(-4.66091941758763,-1.57117057610563,
47.0754613878824));
#33294=CARTESIAN_POINT('Ctrl Pts',(-4.67964671979863,-1.51448126474898,
47.0720993421993));
#33295=CARTESIAN_POINT('Ctrl Pts',(-4.74976254563909,-1.28850137310328,
47.0588001798797));
#33296=CARTESIAN_POINT('Ctrl Pts',(-4.79303317872285,-1.11683193531472,
47.0489195370147));
#33297=CARTESIAN_POINT('Ctrl Pts',(-4.84215167289235,-0.865462227076943,
47.034549605177));
#33298=CARTESIAN_POINT('Ctrl Pts',(-4.85546229926689,-0.787364842118274,
47.030099255353));
#33299=CARTESIAN_POINT('Ctrl Pts',(-4.87736378605435,-0.637019507328562,
47.0215408617709));
#33300=CARTESIAN_POINT('Ctrl Pts',(-4.88624930102355,-0.564835339769297,
47.0174357407346));
#33301=CARTESIAN_POINT('Ctrl Pts',(-4.89980735586483,-0.430115987474027,
47.0097717378524));
#33302=CARTESIAN_POINT('Ctrl Pts',(-4.90489091934934,-0.367636843723732,
47.0062164186091));
#33303=CARTESIAN_POINT('Ctrl Pts',(-4.91509408357548,-0.203465495901944,
46.9968661112378));
#33304=CARTESIAN_POINT('Ctrl Pts',(-4.91825257506775,-0.101682306156651,
46.9910603738107));
#33305=CARTESIAN_POINT('Ctrl Pts',(-4.91824501973881,0.196839665486888,
46.9739978707272));
#33306=CARTESIAN_POINT('Ctrl Pts',(-4.90643805323138,0.393377564105095,
46.9627139993045));
#33307=CARTESIAN_POINT('Ctrl Pts',(-4.87745889323441,0.633749680902723,
46.9489218794627));
#33308=CARTESIAN_POINT('Ctrl Pts',(-4.87140144799517,0.678742889758802,
46.9463410435686));
#33309=CARTESIAN_POINT('Ctrl Pts',(-4.85893885155642,0.762522882634252,
46.9415395638995));
#33310=CARTESIAN_POINT('Ctrl Pts',(-4.85268996844676,0.801328902813746,
46.9393175718323));
#33311=CARTESIAN_POINT('Ctrl Pts',(-4.82751650861538,0.946545363256888,
46.9310025349431));
#33312=CARTESIAN_POINT('Ctrl Pts',(-4.80555118266694,1.05239826538985,46.9249403681993));
#33313=CARTESIAN_POINT('Ctrl Pts',(-4.77490049252517,1.17898241002546,46.9176411071331));
#33314=CARTESIAN_POINT('Ctrl Pts',(-4.76953983018175,1.20048484241867,46.9163994793669));
#33315=CARTESIAN_POINT('Ctrl Pts',(-4.76403458328184,1.22194826068645,46.9151580697526));
#33316=CARTESIAN_POINT('',(-4.91785582195738,6.53930245273875E-6,46.6398437988878));
#33317=CARTESIAN_POINT('Ctrl Pts',(-4.7640345870679,1.22194824592564,46.5701705954582));
#33318=CARTESIAN_POINT('Ctrl Pts',(-4.76723354040696,1.2094764211978,46.5709009832683));
#33319=CARTESIAN_POINT('Ctrl Pts',(-4.77038354248472,1.19699194120722,46.5716307886145));
#33320=CARTESIAN_POINT('Ctrl Pts',(-4.78152228235782,1.15210310833962,46.5742500147955));
#33321=CARTESIAN_POINT('Ctrl Pts',(-4.78923018167354,1.11962994056537,46.576135852302));
#33322=CARTESIAN_POINT('Ctrl Pts',(-4.80697392655666,1.0413378914593,46.5806642795432));
#33323=CARTESIAN_POINT('Ctrl Pts',(-4.81668604876316,0.995448892470532,
46.5833035425673));
#33324=CARTESIAN_POINT('Ctrl Pts',(-4.8745292050673,0.701444363990078,46.6001397299728));
#33325=CARTESIAN_POINT('Ctrl Pts',(-4.90413055987128,0.450069787444037,
46.614223605967));
#33326=CARTESIAN_POINT('Ctrl Pts',(-4.91692699994307,0.131721368016909,
46.6321721991386));
#33327=CARTESIAN_POINT('Ctrl Pts',(-4.91825008432671,0.0658606293943527,
46.6358900870717));
#33328=CARTESIAN_POINT('Ctrl Pts',(-4.91824999999597,-6.29693351562663E-6,
46.6396169269188));
#33329=CARTESIAN_POINT('Ctrl Pts',(-4.91782865331878,7.42403732347657E-6,
46.6398594359907));
#33330=CARTESIAN_POINT('Ctrl Pts',(-4.91780676097348,-0.417173566090727,
46.6634791213957));
#33331=CARTESIAN_POINT('Ctrl Pts',(-4.76226060784274,-1.65284746667128,
46.7334388053049));
#33332=CARTESIAN_POINT('Ctrl Pts',(-3.7390810765516,-3.50817654536093,46.8497384877184));
#33333=CARTESIAN_POINT('Ctrl Pts',(-1.60365005368828,-4.86994214271806,
46.9887584832308));
#33334=CARTESIAN_POINT('Ctrl Pts',(0.923083286691152,-5.04340631076602,
47.1277784787434));
#33335=CARTESIAN_POINT('Ctrl Pts',(3.22457756921184,-3.98624252566559,47.2667984742559));
#33336=CARTESIAN_POINT('Ctrl Pts',(4.73925138433377,-1.95640646877516,47.4058184697685));
#33337=CARTESIAN_POINT('Ctrl Pts',(5.09751327602456,0.550807048437444,47.5448384652809));
#33338=CARTESIAN_POINT('Ctrl Pts',(4.21194470665123,2.92361962201063,47.6838584607935));
#33339=CARTESIAN_POINT('Ctrl Pts',(2.29863091214187,4.58304767427664,47.8228784563059));
#33340=CARTESIAN_POINT('Ctrl Pts',(-0.175565656096785,5.12417862858086,
47.9618984518186));
#33341=CARTESIAN_POINT('Ctrl Pts',(-2.60692281934329,4.41497262009648,48.1009184473309));
#33342=CARTESIAN_POINT('Ctrl Pts',(-4.14805938556448,2.881354010624,48.2202605432668));
#33343=CARTESIAN_POINT('Ctrl Pts',(-4.64647847283068,1.67794619770932,48.2932626406984));
#33344=CARTESIAN_POINT('Ctrl Pts',(-4.76366299354682,1.22185269443844,48.3199247396258));
#33345=CARTESIAN_POINT('Origin',(0.,0.,-3.23514056400928));
#33346=CARTESIAN_POINT('',(-4.91825415174279,6.46578250284212E-5,48.3898594374466));
#33347=CARTESIAN_POINT('Ctrl Pts',(-4.76366299354682,1.22185269443844,48.3199247396258));
#33348=CARTESIAN_POINT('Ctrl Pts',(-4.85015075420195,0.885233954128829,
48.3396026392026));
#33349=CARTESIAN_POINT('Ctrl Pts',(-4.9107614377059,0.475756808800476,48.3629142046575));
#33350=CARTESIAN_POINT('Ctrl Pts',(-4.91864568349125,0.0642149472873671,
48.3862257701125));
#33351=CARTESIAN_POINT('Ctrl Pts',(-4.91860392675717,6.46881271033038E-5,
48.3898594359907));
#33352=CARTESIAN_POINT('',(-4.31106608169009,2.36725416924362,50.));
#33353=CARTESIAN_POINT('Ctrl Pts',(-4.91824999957499,6.4657465313589E-5,
48.3898594374639));
#33354=CARTESIAN_POINT('Ctrl Pts',(-4.91825188690336,-0.143497307078023,
48.3979918092232));
#33355=CARTESIAN_POINT('Ctrl Pts',(-4.9119636472632,-0.287087752773969,
48.4061241809826));
#33356=CARTESIAN_POINT('Ctrl Pts',(-4.89940385679968,-0.430145220217989,
48.4142565527419));
#33357=CARTESIAN_POINT('Ctrl Pts',(-4.88684656678358,-0.573174207276529,
48.4223873054799));
#33358=CARTESIAN_POINT('Ctrl Pts',(-4.86802024625112,-0.715670090689004,
48.430518058218));
#33359=CARTESIAN_POINT('Ctrl Pts',(-4.84299541970709,-0.857075508456625,
48.438648810956));
#33360=CARTESIAN_POINT('Ctrl Pts',(-4.81796978997819,-0.99848546470493,
48.4467798246548));
#33361=CARTESIAN_POINT('Ctrl Pts',(-4.78674531227144,-1.13880455141727,
48.4549108383536));
#33362=CARTESIAN_POINT('Ctrl Pts',(-4.74944389329373,-1.27748415526571,
48.4630418520524));
#33363=CARTESIAN_POINT('Ctrl Pts',(-4.71214345251239,-1.41616012236545,
48.4711726525226));
#33364=CARTESIAN_POINT('Ctrl Pts',(-4.66876647949925,-1.55319636631919,
48.4793034529928));
#33365=CARTESIAN_POINT('Ctrl Pts',(-4.61948514488079,-1.68805807326814,
48.487434253463));
#33366=CARTESIAN_POINT('Ctrl Pts',(-4.57019270843371,-1.82295016112231,
48.4955668855954));
#33367=CARTESIAN_POINT('Ctrl Pts',(-4.51499337112636,-1.95566641597054,
48.5036995177277));
#33368=CARTESIAN_POINT('Ctrl Pts',(-4.45410813183877,-2.08569024842802,
48.51183214986));
#33369=CARTESIAN_POINT('Ctrl Pts',(-4.4387700073343,-2.11844567082787,48.5138809111962));
#33370=CARTESIAN_POINT('Ctrl Pts',(-4.42307127439285,-2.15103032930286,
48.5159296725323));
#33371=CARTESIAN_POINT('Ctrl Pts',(-4.40701593818226,-2.18343618709307,
48.5179784338685));
#33372=CARTESIAN_POINT('Ctrl Pts',(-4.34309859665993,-2.31244602236111,
48.5261346864877));
#33373=CARTESIAN_POINT('Ctrl Pts',(-4.27350049521726,-2.43867143502133,
48.534290939107));
#33374=CARTESIAN_POINT('Ctrl Pts',(-4.19848925582428,-2.56161492641421,
48.5424471917262));
#33375=CARTESIAN_POINT('Ctrl Pts',(-4.12349330707571,-2.68453335642663,
48.5506017817365));
#33376=CARTESIAN_POINT('Ctrl Pts',(-4.04308659586943,-2.80417091427926,
48.5587563717468));
#33377=CARTESIAN_POINT('Ctrl Pts',(-3.9575814689975,-2.92005684512264,48.5669109617571));
#33378=CARTESIAN_POINT('Ctrl Pts',(-3.87207330801335,-3.03594688812785,
48.5750658411294));
#33379=CARTESIAN_POINT('Ctrl Pts',(-3.78146656500964,-3.14808476622646,
48.5832207205018));
#33380=CARTESIAN_POINT('Ctrl Pts',(-3.68611578484381,-3.25603032590688,
48.5913755998741));
#33381=CARTESIAN_POINT('Ctrl Pts',(-3.59077060912433,-3.36396954085581,
48.599529999926));
#33382=CARTESIAN_POINT('Ctrl Pts',(-3.49068217637334,-3.46771668016612,
48.6076843999778));
#33383=CARTESIAN_POINT('Ctrl Pts',(-3.38624399038185,-3.56686622963391,
48.6158388000297));
#33384=CARTESIAN_POINT('Ctrl Pts',(-3.28178005384405,-3.66604022566825,
48.6239952106513));
#33385=CARTESIAN_POINT('Ctrl Pts',(-3.17296446365347,-3.76061413599753,
48.6321516212729));
#33386=CARTESIAN_POINT('Ctrl Pts',(-3.0602265519251,-3.8502203201106,48.6403080318945));
#33387=CARTESIAN_POINT('Ctrl Pts',(-2.98332832443053,-3.91134045818315,
48.6458714977234));
#33388=CARTESIAN_POINT('Ctrl Pts',(-2.90460594879125,-3.97015012395728,
48.6514349635522));
#33389=CARTESIAN_POINT('Ctrl Pts',(-2.82420423355466,-4.02654361825027,
48.6569984293811));
#33390=CARTESIAN_POINT('Ctrl Pts',(-2.70632998692356,-4.10922022079686,
48.6651548392451));
#33391=CARTESIAN_POINT('Ctrl Pts',(-2.58480074625422,-4.18673270427483,
48.673311249109));
#33392=CARTESIAN_POINT('Ctrl Pts',(-2.4600896394939,-4.25877236162662,48.681467658973));
#33393=CARTESIAN_POINT('Ctrl Pts',(-2.3354039429029,-4.33079734073573,48.6896224069501));
#33394=CARTESIAN_POINT('Ctrl Pts',(-2.20753796315363,-4.39735155099705,
48.6977771549271));
#33395=CARTESIAN_POINT('Ctrl Pts',(-2.07699129460226,-4.45817117489295,
48.7059319029042));
#33396=CARTESIAN_POINT('Ctrl Pts',(-1.94644000136145,-4.51899295335837,
48.7140869397678));
#33397=CARTESIAN_POINT('Ctrl Pts',(-1.81320813102232,-4.57407959423216,
48.7222419766314));
#33398=CARTESIAN_POINT('Ctrl Pts',(-1.67781767950347,-4.62321434684199,
48.730397013495));
#33399=CARTESIAN_POINT('Ctrl Pts',(-1.54243519621796,-4.67234620768826,
48.7385515704042));
#33400=CARTESIAN_POINT('Ctrl Pts',(-1.40489470080638,-4.71552676779961,
48.7467061273135));
#33401=CARTESIAN_POINT('Ctrl Pts',(-1.26573581428016,-4.75258833804786,
48.7548606842228));
#33402=CARTESIAN_POINT('Ctrl Pts',(-1.12654265863381,-4.78965903503918,
48.7630172492646));
#33403=CARTESIAN_POINT('Ctrl Pts',(-0.985730638942556,-4.82060764474622,
48.7711738143064));
#33404=CARTESIAN_POINT('Ctrl Pts',(-0.843852704477646,-4.84531688082893,
48.7793303793482));
#33405=CARTESIAN_POINT('Ctrl Pts',(-0.747093614504557,-4.86216829050239,
48.7848930611967));
#33406=CARTESIAN_POINT('Ctrl Pts',(-0.649839026362427,-4.87611876961641,
48.7904557430452));
#33407=CARTESIAN_POINT('Ctrl Pts',(-0.552266597345409,-4.88714483803749,
48.7960184248937));
#33408=CARTESIAN_POINT('Ctrl Pts',(-0.409205056356983,-4.90331135510851,
48.8041744772262));
#33409=CARTESIAN_POINT('Ctrl Pts',(-0.265406350851102,-4.91319481873329,
48.8123305295588));
#33410=CARTESIAN_POINT('Ctrl Pts',(-0.121433605261592,-4.91675064875301,
48.8204865818913));
#33411=CARTESIAN_POINT('Ctrl Pts',(0.0225097812274147,-4.92030575366348,
48.8286409710316));
#33412=CARTESIAN_POINT('Ctrl Pts',(0.166626802610623,-4.91753579085466,
48.8367953601718));
#33413=CARTESIAN_POINT('Ctrl Pts',(0.310352583167036,-4.90844826158141,
48.8449497493121));
#33414=CARTESIAN_POINT('Ctrl Pts',(0.454083483381406,-4.89936040860115,
48.8531044289199));
#33415=CARTESIAN_POINT('Ctrl Pts',(0.597422780632983,-4.88395455621873,
48.8612591085278));
#33416=CARTESIAN_POINT('Ctrl Pts',(0.739808459343981,-4.86229025316086,
48.8694137881357));
#33417=CARTESIAN_POINT('Ctrl Pts',(0.882185787764231,-4.84062722061861,
48.8775679895076));
#33418=CARTESIAN_POINT('Ctrl Pts',(1.02360927877759,-4.81270652298323,48.8857221908795));
#33419=CARTESIAN_POINT('Ctrl Pts',(1.16352492632272,-4.77863922140244,48.8938763922515));
#33420=CARTESIAN_POINT('Ctrl Pts',(1.30347513317182,-4.7445635051643,48.9020326077193));
#33421=CARTESIAN_POINT('Ctrl Pts',(1.44191642694179,-4.70433823023442,48.910188823187));
#33422=CARTESIAN_POINT('Ctrl Pts',(1.57830722573228,-4.65812509103193,48.9183450386548));
#33423=CARTESIAN_POINT('Ctrl Pts',(1.67135788468709,-4.62659684210829,48.9239094992386));
#33424=CARTESIAN_POINT('Ctrl Pts',(1.76345441903967,-4.59228262112032,48.9294739598223));
#33425=CARTESIAN_POINT('Ctrl Pts',(1.85442944131458,-4.555246920825,48.9350384204061));
#33426=CARTESIAN_POINT('Ctrl Pts',(1.98778541037635,-4.50095804483178,48.9431950991833));
#33427=CARTESIAN_POINT('Ctrl Pts',(2.11878067919415,-4.44079895903165,48.9513517779606));
#33428=CARTESIAN_POINT('Ctrl Pts',(2.24689941917647,-4.3750001214405,48.9595084567379));
#33429=CARTESIAN_POINT('Ctrl Pts',(2.37499206212136,-4.30921468668744,48.9676634740474));
#33430=CARTESIAN_POINT('Ctrl Pts',(2.50020904767986,-4.23779194466744,48.9758184913569));
#33431=CARTESIAN_POINT('Ctrl Pts',(2.6220579407557,-4.16100891825768,48.9839735086665));
#33432=CARTESIAN_POINT('Ctrl Pts',(2.74391111994757,-4.0842231909538,48.9921288128342));
#33433=CARTESIAN_POINT('Ctrl Pts',(2.86239568451947,-4.00207697715491,49.0002841170019));
#33434=CARTESIAN_POINT('Ctrl Pts',(2.97704662494939,-3.91489162753932,49.0084394211696));
#33435=CARTESIAN_POINT('Ctrl Pts',(3.09169079322723,-3.82771142775019,49.0165942436234));
#33436=CARTESIAN_POINT('Ctrl Pts',(3.20250152461738,-3.73549289091029,49.0247490660771));
#33437=CARTESIAN_POINT('Ctrl Pts',(3.30904549887002,-3.63859876173618,49.0329038885308));
#33438=CARTESIAN_POINT('Ctrl Pts',(3.41561564176688,-3.5416808340506,49.0410607139195));
#33439=CARTESIAN_POINT('Ctrl Pts',(3.51791668563332,-3.44008524433254,49.0492175393082));
#33440=CARTESIAN_POINT('Ctrl Pts',(3.61555045472144,-3.33421324630918,49.0573743646968));
#33441=CARTESIAN_POINT('Ctrl Pts',(3.68211747995647,-3.26202936946075,49.0629357151041));
#33442=CARTESIAN_POINT('Ctrl Pts',(3.7465156353158,-3.18785837437165,49.0684970655114));
#33443=CARTESIAN_POINT('Ctrl Pts',(3.80862902171563,-3.11183676266051,49.0740584159187));
#33444=CARTESIAN_POINT('Ctrl Pts',(3.89972024128471,-3.00034869662916,49.0822143098478));
#33445=CARTESIAN_POINT('Ctrl Pts',(3.98592987250361,-2.88483728265233,49.0903702037769));
#33446=CARTESIAN_POINT('Ctrl Pts',(4.06691538033361,-2.76575167932805,49.098526097706));
#33447=CARTESIAN_POINT('Ctrl Pts',(4.14788438100405,-2.64669034905097,49.1066803292309));
#33448=CARTESIAN_POINT('Ctrl Pts',(4.22363119443135,-2.52405655939287,49.1148345607558));
#33449=CARTESIAN_POINT('Ctrl Pts',(4.29385611314292,-2.39832915633471,49.1229887922808));
#33450=CARTESIAN_POINT('Ctrl Pts',(4.36408355692555,-2.27259723250767,49.1311433170067));
#33451=CARTESIAN_POINT('Ctrl Pts',(4.42878854219891,-2.14377176307623,49.1392978417326));
#33452=CARTESIAN_POINT('Ctrl Pts',(4.48771665879655,-2.01235738696186,49.1474523664585));
#33453=CARTESIAN_POINT('Ctrl Pts',(4.54664133311361,-1.88095068740634,49.1556064148386));
#33454=CARTESIAN_POINT('Ctrl Pts',(4.59978967780052,-1.74695568954819,49.1637604632187));
#33455=CARTESIAN_POINT('Ctrl Pts',(4.64695492019639,-1.61089820664204,49.1719145115987));
#33456=CARTESIAN_POINT('Ctrl Pts',(4.69413183789641,-1.47480704400874,49.1800705784354));
#33457=CARTESIAN_POINT('Ctrl Pts',(4.73532258392123,-1.33665269246272,49.1882266452721));
#33458=CARTESIAN_POINT('Ctrl Pts',(4.7703696757342,-1.19697795273578,49.1963827121088));
#33459=CARTESIAN_POINT('Ctrl Pts',(4.79428380488269,-1.10167190616176,49.2019479452162));
#33460=CARTESIAN_POINT('Ctrl Pts',(4.81533852993245,-1.00565832347219,49.2075131783236));
#33461=CARTESIAN_POINT('Ctrl Pts',(4.83349736403111,-0.909112916201438,
49.2130784114311));
#33462=CARTESIAN_POINT('Ctrl Pts',(4.86011027114623,-0.767619583417664,
49.2212346086272));
#33463=CARTESIAN_POINT('Ctrl Pts',(4.88051089537211,-0.624930332658238,
49.2293908058235));
#33464=CARTESIAN_POINT('Ctrl Pts',(4.89461347930164,-0.481603520272367,
49.2375470030197));
#33465=CARTESIAN_POINT('Ctrl Pts',(4.90871318301751,-0.338305979957791,
49.2457015344509));
#33466=CARTESIAN_POINT('Ctrl Pts',(4.91651737970788,-0.194371470640131,
49.2538560658821));
#33467=CARTESIAN_POINT('Ctrl Pts',(4.91799212469945,-0.050363914603593,
49.2620105973133));
#33468=CARTESIAN_POINT('Ctrl Pts',(4.91946692127142,0.0936486782139966,
49.2701654139559));
#33469=CARTESIAN_POINT('Ctrl Pts',(4.91461181596314,0.237733988262807,49.2783202305984));
#33470=CARTESIAN_POINT('Ctrl Pts',(4.9034449811488,0.381327129046287,49.286475047241));
#33471=CARTESIAN_POINT('Ctrl Pts',(4.89227880567297,0.524911791465909,49.2946293823877));
#33472=CARTESIAN_POINT('Ctrl Pts',(4.87480167315109,0.668004009156202,49.3027837175344));
#33473=CARTESIAN_POINT('Ctrl Pts',(4.85108371705545,0.810043105408263,49.3109380526811));
#33474=CARTESIAN_POINT('Ctrl Pts',(4.82735992108153,0.952117174784864,49.319094395603));
#33475=CARTESIAN_POINT('Ctrl Pts',(4.79739228592106,1.09313727429167,49.3272507385249));
#33476=CARTESIAN_POINT('Ctrl Pts',(4.7613023531058,1.23255140453011,49.3354070814469));
#33477=CARTESIAN_POINT('Ctrl Pts',(4.73668393357037,1.32765148590034,49.3409708566125));
#33478=CARTESIAN_POINT('Ctrl Pts',(4.70921777841567,1.42200447474435,49.3465346317781));
#33479=CARTESIAN_POINT('Ctrl Pts',(4.67895590890541,1.51543876980205,49.3520984069438));
#33480=CARTESIAN_POINT('Ctrl Pts',(4.63458299103438,1.6524412870962,49.360256559182));
#33481=CARTESIAN_POINT('Ctrl Pts',(4.5841804662064,1.78751890601388,49.3684147114202));
#33482=CARTESIAN_POINT('Ctrl Pts',(4.5279404776491,1.92014012336779,49.3765728636584));
#33483=CARTESIAN_POINT('Ctrl Pts',(4.47171186823887,2.05273450721095,49.3847293652417));
#33484=CARTESIAN_POINT('Ctrl Pts',(4.40964828181284,2.18287317337993,49.3928858668249));
#33485=CARTESIAN_POINT('Ctrl Pts',(4.34199001409317,2.31004454069942,49.4010423684082));
#33486=CARTESIAN_POINT('Ctrl Pts',(4.27432935420594,2.43722040436842,49.4091991583778));
#33487=CARTESIAN_POINT('Ctrl Pts',(4.20107377094131,2.56142846234591,49.4173559483474));
#33488=CARTESIAN_POINT('Ctrl Pts',(4.12250977738952,2.68218123881064,49.425512738317));
#33489=CARTESIAN_POINT('Ctrl Pts',(4.0439504489463,2.80292684500836,49.4336690439386));
#33490=CARTESIAN_POINT('Ctrl Pts',(3.96008352394967,2.9202173004152,49.4418253495602));
#33491=CARTESIAN_POINT('Ctrl Pts',(3.87123912075788,3.03359369929688,49.4499816551819));
#33492=CARTESIAN_POINT('Ctrl Pts',(3.78237309431381,3.14699769211119,49.4581399459128));
#33493=CARTESIAN_POINT('Ctrl Pts',(3.68852737507418,3.25648546142182,49.4662982366438));
#33494=CARTESIAN_POINT('Ctrl Pts',(3.59007306298733,3.36163032841399,49.4744565273747));
#33495=CARTESIAN_POINT('Ctrl Pts',(3.52304785295607,3.43321029931098,49.4800104857352));
#33496=CARTESIAN_POINT('Ctrl Pts',(3.45388761708271,3.50277821283592,49.4855644440957));
#33497=CARTESIAN_POINT('Ctrl Pts',(3.38271944840214,3.57020898490578,49.4911184024561));
#33498=CARTESIAN_POINT('Ctrl Pts',(3.27828225345075,3.66916166022317,49.4992686730448));
#33499=CARTESIAN_POINT('Ctrl Pts',(3.16947995222353,3.76354777596328,49.5074189436334));
#33500=CARTESIAN_POINT('Ctrl Pts',(3.05673468831527,3.85299313621892,49.515569214222));
#33501=CARTESIAN_POINT('Ctrl Pts',(2.94401279067063,3.94241995907624,49.523717795681));
#33502=CARTESIAN_POINT('Ctrl Pts',(2.82734982328878,4.02690786064281,49.5318663771399));
#33503=CARTESIAN_POINT('Ctrl Pts',(2.70720069172927,4.10612316878105,49.5400149585989));
#33504=CARTESIAN_POINT('Ctrl Pts',(2.58704701179802,4.1853414756981,49.548163848531));
#33505=CARTESIAN_POINT('Ctrl Pts',(2.46340718173827,4.25928660186803,49.556312738463));
#33506=CARTESIAN_POINT('Ctrl Pts',(2.33676516282422,4.32766815228607,49.5644616283951));
#33507=CARTESIAN_POINT('Ctrl Pts',(2.21013021263356,4.39604588588035,49.5726100634841));
#33508=CARTESIAN_POINT('Ctrl Pts',(2.08049370471521,4.45886050647418,49.580758498573));
#33509=CARTESIAN_POINT('Ctrl Pts',(1.94836421109051,4.51586757594171,49.588906933662));
#33510=CARTESIAN_POINT('Ctrl Pts',(1.81620060637184,4.57288936258896,49.5970574723845));
#33511=CARTESIAN_POINT('Ctrl Pts',(1.68154303816524,4.62410046898825,49.605208011107));
#33512=CARTESIAN_POINT('Ctrl Pts',(1.5449206338762,4.66930436976682,49.6133585498296));
#33513=CARTESIAN_POINT('Ctrl Pts',(1.45116391936385,4.70032541087788,49.6189518325426));
#33514=CARTESIAN_POINT('Ctrl Pts',(1.35648231503136,4.72851845203959,49.6245451152557));
#33515=CARTESIAN_POINT('Ctrl Pts',(1.26105114876189,4.75383351230418,49.6301383979688));
#33516=CARTESIAN_POINT('Ctrl Pts',(1.12165256809271,4.79081182461438,49.6383086394314));
#33517=CARTESIAN_POINT('Ctrl Pts',(0.98060213796819,4.82166090769783,49.6464788808941));
#33518=CARTESIAN_POINT('Ctrl Pts',(0.838452342310928,4.8462542991648,49.6546491223567));
#33519=CARTESIAN_POINT('Ctrl Pts',(0.696330650913473,4.87084282830284,49.6628177484911));
#33520=CARTESIAN_POINT('Ctrl Pts',(0.55311035489733,4.88917807673463,49.6709863746254));
#33521=CARTESIAN_POINT('Ctrl Pts',(0.409353248986643,4.90118485471055,49.6791550007598));
#33522=CARTESIAN_POINT('Ctrl Pts',(0.265592281209922,4.91319195523448,49.6873238463347));
#33523=CARTESIAN_POINT('Ctrl Pts',(0.121294805525717,4.9188702137094,49.6954926919096));
#33524=CARTESIAN_POINT('Ctrl Pts',(-0.0229726286740002,4.9181963483407,
49.7036615374845));
#33525=CARTESIAN_POINT('Ctrl Pts',(-0.167230310106315,4.91752252852665,
49.7118298308291));
#33526=CARTESIAN_POINT('Ctrl Pts',(-0.311457621791795,4.91049744605797,
49.7199981241736));
#33527=CARTESIAN_POINT('Ctrl Pts',(-0.455088397425796,4.89714994798285,
49.7281664175182));
#33528=CARTESIAN_POINT('Ctrl Pts',(-0.598750248365985,4.8837995621033,49.7363364781179));
#33529=CARTESIAN_POINT('Ctrl Pts',(-0.741814974285452,4.86412405760869,
49.7445065387176));
#33530=CARTESIAN_POINT('Ctrl Pts',(-0.883721287240841,4.83820418636682,
49.7526765993172));
#33531=CARTESIAN_POINT('Ctrl Pts',(-0.979145738184204,4.8207744509994,49.7581705307052));
#33532=CARTESIAN_POINT('Ctrl Pts',(-1.07404648628848,4.80052218270611,49.7636644620932));
#33533=CARTESIAN_POINT('Ctrl Pts',(-1.16825532506712,4.77748496156213,49.7691583934811));
#33534=CARTESIAN_POINT('Ctrl Pts',(-1.30767583788311,4.74339196957339,49.7772889122458));
#33535=CARTESIAN_POINT('Ctrl Pts',(-1.44563187930691,4.70318465095805,49.7854194310104));
#33536=CARTESIAN_POINT('Ctrl Pts',(-1.5815826097383,4.6570140123338,49.7935499497751));
#33537=CARTESIAN_POINT('Ctrl Pts',(-1.71750497273023,4.61085300766144,49.8016787720281));
#33538=CARTESIAN_POINT('Ctrl Pts',(-1.85142253869643,4.55873127390083,49.8098075942811));
#33539=CARTESIAN_POINT('Ctrl Pts',(-1.98281074732252,4.50084932016195,49.8179364165341));
#33540=CARTESIAN_POINT('Ctrl Pts',(-2.11420682945525,4.44296389781694,49.826065725911));
#33541=CARTESIAN_POINT('Ctrl Pts',(-2.24307293941015,4.37931769817334,49.8341950352879));
#33542=CARTESIAN_POINT('Ctrl Pts',(-2.36890512983529,4.31015910939956,49.8423243446648));
#33543=CARTESIAN_POINT('Ctrl Pts',(-2.49473248588189,4.24100317764699,49.8504533417197));
#33544=CARTESIAN_POINT('Ctrl Pts',(-2.61752585952728,4.1663354454027,49.8585823387746));
#33545=CARTESIAN_POINT('Ctrl Pts',(-2.73680662682732,4.08644987120288,49.8667113358296));
#33546=CARTESIAN_POINT('Ctrl Pts',(-2.85612413052588,4.00653969363778,49.874842836474));
#33547=CARTESIAN_POINT('Ctrl Pts',(-2.97192658454216,3.92140865181147,49.8829743371184));
#33548=CARTESIAN_POINT('Ctrl Pts',(-3.08376452537185,3.83139392578708,49.8911058377628));
#33549=CARTESIAN_POINT('Ctrl Pts',(-3.16203457899332,3.76839690187567,49.8967966881731));
#33550=CARTESIAN_POINT('Ctrl Pts',(-3.23836345535582,3.70300878338029,49.9024875385834));
#33551=CARTESIAN_POINT('Ctrl Pts',(-3.31260678046568,3.63535684362798,49.9081783889938));
#33552=CARTESIAN_POINT('Ctrl Pts',(-3.41989988008897,3.53758931636796,49.9164025489315));
#33553=CARTESIAN_POINT('Ctrl Pts',(-3.52287846090169,3.43505347941445,49.9246267088693));
#33554=CARTESIAN_POINT('Ctrl Pts',(-3.62113200122419,3.32815055131377,49.9328508688071));
#33555=CARTESIAN_POINT('Ctrl Pts',(-3.71936169908124,3.22127356456196,49.9410730330484));
#33556=CARTESIAN_POINT('Ctrl Pts',(-3.81286842630019,3.11003183946856,49.9492951972896));
#33557=CARTESIAN_POINT('Ctrl Pts',(-3.90127974942257,2.99486216364716,49.9575173615309));
#33558=CARTESIAN_POINT('Ctrl Pts',(-3.98968144240252,2.87970503260333,49.9657386301785));
#33559=CARTESIAN_POINT('Ctrl Pts',(-4.07298864057679,2.76062105963968,49.9739598988262));
#33560=CARTESIAN_POINT('Ctrl Pts',(-4.15086999848057,2.63807909627705,49.9821811674739));
#33561=CARTESIAN_POINT('Ctrl Pts',(-4.20713685675021,2.54954633991283,49.988120778316));
#33562=CARTESIAN_POINT('Ctrl Pts',(-4.26057248301015,2.45920933123667,49.994060389158));
#33563=CARTESIAN_POINT('Ctrl Pts',(-4.31106608169009,2.36725416924362,50.));
#33564=CARTESIAN_POINT('',(0.837162017642341,4.84647736182859,50.));
#33565=CARTESIAN_POINT('Origin',(0.,0.,50.));
#33566=CARTESIAN_POINT('',(-4.91824999932842,-8.12775897282569E-5,48.7351405640092));
#33567=CARTESIAN_POINT('Ctrl Pts',(-4.91824999932841,-8.12775897283124E-5,
48.7351405640092));
#33568=CARTESIAN_POINT('Ctrl Pts',(-4.91824860461297,-0.0844779637138754,
48.7399212201507));
#33569=CARTESIAN_POINT('Ctrl Pts',(-4.91607448844467,-0.168867401146295,
48.7447018762922));
#33570=CARTESIAN_POINT('Ctrl Pts',(-4.91173094479186,-0.253144599930679,
48.7494825324338));
#33571=CARTESIAN_POINT('Ctrl Pts',(-4.90432050159678,-0.396928441915993,
48.7576387255341));
#33572=CARTESIAN_POINT('Ctrl Pts',(-4.89059073704431,-0.540413569487469,
48.7657949186345));
#33573=CARTESIAN_POINT('Ctrl Pts',(-4.87058963142793,-0.683037118117827,
48.7739511117348));
#33574=CARTESIAN_POINT('Ctrl Pts',(-4.85059259870388,-0.825631623835872,
48.7821056439622));
#33575=CARTESIAN_POINT('Ctrl Pts',(-4.82432681901249,-0.967364569392464,
48.7902601761895));
#33576=CARTESIAN_POINT('Ctrl Pts',(-4.7918919408917,-1.1076798677042,48.7984147084169));
#33577=CARTESIAN_POINT('Ctrl Pts',(-4.75945590785336,-1.248000162261,48.8065695310049));
#33578=CARTESIAN_POINT('Ctrl Pts',(-4.72085040855073,-1.38690238166367,
48.8147243535928));
#33579=CARTESIAN_POINT('Ctrl Pts',(-4.67622597313651,-1.52384176037524,
48.8228791761808));
#33580=CARTESIAN_POINT('Ctrl Pts',(-4.63160414837477,-1.66077312775566,
48.8310335216892));
#33581=CARTESIAN_POINT('Ctrl Pts',(-4.58096419657989,-1.7957415662676,48.8391878671976));
#33582=CARTESIAN_POINT('Ctrl Pts',(-4.5245061608825,-1.92821862418044,48.847342212706));
#33583=CARTESIAN_POINT('Ctrl Pts',(-4.46803421536716,-2.06072832105663,
48.8554985672369));
#33584=CARTESIAN_POINT('Ctrl Pts',(-4.40574145271102,-2.19074510270008,
48.8636549217677));
#33585=CARTESIAN_POINT('Ctrl Pts',(-4.3378758403449,-2.31776104382053,48.8718112762986));
#33586=CARTESIAN_POINT('Ctrl Pts',(-4.29178636058946,-2.40402120478847,
48.8773504901054));
#33587=CARTESIAN_POINT('Ctrl Pts',(-4.24312758724043,-2.48889776854284,
48.8828897039122));
#33588=CARTESIAN_POINT('Ctrl Pts',(-4.1919892239971,-2.57223820988496,48.888428917719));
#33589=CARTESIAN_POINT('Ctrl Pts',(-4.11668498514456,-2.69496189720833,
48.8965857348933));
#33590=CARTESIAN_POINT('Ctrl Pts',(-4.03597375155277,-2.81439932341442,
48.9047425520675));
#33591=CARTESIAN_POINT('Ctrl Pts',(-3.95016701024448,-2.93007912071947,
48.9128993692417));
#33592=CARTESIAN_POINT('Ctrl Pts',(-3.86437772267667,-3.0457353878784,48.9210545272576));
#33593=CARTESIAN_POINT('Ctrl Pts',(-3.77349519428314,-3.15763528238476,
48.9292096852735));
#33594=CARTESIAN_POINT('Ctrl Pts',(-3.67787303964822,-3.26533810909816,
48.9373648432894));
#33595=CARTESIAN_POINT('Ctrl Pts',(-3.58224752263747,-3.37304472298183,
48.9455202880663));
#33596=CARTESIAN_POINT('Ctrl Pts',(-3.48188226520706,-3.47655372109064,
48.9536757328432));
#33597=CARTESIAN_POINT('Ctrl Pts',(-3.37717014484713,-3.57545869438499,
48.9618311776201));
#33598=CARTESIAN_POINT('Ctrl Pts',(-3.27246419451462,-3.67435783983061,
48.9699861418478));
#33599=CARTESIAN_POINT('Ctrl Pts',(-3.16341213755547,-3.76865327414801,
48.9781411060756));
#33600=CARTESIAN_POINT('Ctrl Pts',(-3.05044252510817,-3.85797660225042,
48.9862960703034));
#33601=CARTESIAN_POINT('Ctrl Pts',(-2.9374452359176,-3.94732181392635,48.9944530324388));
#33602=CARTESIAN_POINT('Ctrl Pts',(-2.82052873581696,-4.03169227751469,
49.0026099945742));
#33603=CARTESIAN_POINT('Ctrl Pts',(-2.70015383907519,-4.11076055102064,
49.0107669567096));
#33604=CARTESIAN_POINT('Ctrl Pts',(-2.61845561461897,-4.16442404508047,
49.0163030721411));
#33605=CARTESIAN_POINT('Ctrl Pts',(-2.53516500631167,-4.21564604350739,
49.0218391875726));
#33606=CARTESIAN_POINT('Ctrl Pts',(-2.45043348771288,-4.26433567918794,
49.0273753030041));
#33607=CARTESIAN_POINT('Ctrl Pts',(-2.32560348256834,-4.33606728004911,
49.035531339025));
#33608=CARTESIAN_POINT('Ctrl Pts',(-2.19759824966692,-4.40232731187191,
49.0436873750459));
#33609=CARTESIAN_POINT('Ctrl Pts',(-2.06691673278157,-4.46285091418564,
49.0518434110668));
#33610=CARTESIAN_POINT('Ctrl Pts',(-1.93626181488615,-4.52336219749108,
49.0599977870035));
#33611=CARTESIAN_POINT('Ctrl Pts',(-1.8029320032343,-4.57813923999919,49.0681521629402));
#33612=CARTESIAN_POINT('Ctrl Pts',(-1.66744856132577,-4.62696427021353,
49.0763065388769));
#33613=CARTESIAN_POINT('Ctrl Pts',(-1.53196024992732,-4.67579105527694,
49.0844612078949));
#33614=CARTESIAN_POINT('Ctrl Pts',(-1.3943184669733,-4.71866528299151,49.0926158769128));
#33615=CARTESIAN_POINT('Ctrl Pts',(-1.2550625510186,-4.75541807368508,49.1007705459307));
#33616=CARTESIAN_POINT('Ctrl Pts',(-1.11581474995482,-4.7921687226751,49.1089247397498));
#33617=CARTESIAN_POINT('Ctrl Pts',(-0.974953327942705,-4.82279856382775,
49.1170789335689));
#33618=CARTESIAN_POINT('Ctrl Pts',(-0.833030761240178,-4.84718916624136,
49.125233127388));
#33619=CARTESIAN_POINT('Ctrl Pts',(-0.691073152419967,-4.87158579094149,
49.13338933456));
#33620=CARTESIAN_POINT('Ctrl Pts',(-0.548054205331753,-4.88974004165502,
49.1415455417321));
#33621=CARTESIAN_POINT('Ctrl Pts',(-0.40453513299909,-4.90158488538854,
49.1497017489041));
#33622=CARTESIAN_POINT('Ctrl Pts',(-0.307051983766232,-4.9096303155223,
49.1552417286991));
#33623=CARTESIAN_POINT('Ctrl Pts',(-0.209338267113324,-4.91476590902321,
49.1607817084942));
#33624=CARTESIAN_POINT('Ctrl Pts',(-0.111570856204851,-4.91698434068543,
49.1663216882892));
#33625=CARTESIAN_POINT('Ctrl Pts',(0.032368985038175,-4.92025046687513,
49.1744780238695));
#33626=CARTESIAN_POINT('Ctrl Pts',(0.17647929533059,-4.91719231805076,49.1826343594499));
#33627=CARTESIAN_POINT('Ctrl Pts',(0.320195185024482,-4.90781602201907,
49.1907906950302));
#33628=CARTESIAN_POINT('Ctrl Pts',(0.463881764555866,-4.89844163823774,
49.1989453671652));
#33629=CARTESIAN_POINT('Ctrl Pts',(0.607173750227318,-4.88275169961299,
49.2071000393002));
#33630=CARTESIAN_POINT('Ctrl Pts',(0.74950918126488,-4.86080436241777,49.2152547114352));
#33631=CARTESIAN_POINT('Ctrl Pts',(0.891849589093414,-4.83885625782888,
49.2234096687002));
#33632=CARTESIAN_POINT('Ctrl Pts',(1.03323304406454,-4.81065036414039,49.2315646259652));
#33633=CARTESIAN_POINT('Ctrl Pts',(1.17310510440446,-4.77629641841042,49.2397195832302));
#33634=CARTESIAN_POINT('Ctrl Pts',(1.31296892638229,-4.74194449610273,49.2478740601742));
#33635=CARTESIAN_POINT('Ctrl Pts',(1.45132120705093,-4.70144532694967,49.2560285371182));
#33636=CARTESIAN_POINT('Ctrl Pts',(1.5876201028899,-4.65495923412868,49.2641830140622));
#33637=CARTESIAN_POINT('Ctrl Pts',(1.72395247403347,-4.60846172422241,49.2723394937634));
#33638=CARTESIAN_POINT('Ctrl Pts',(1.8582301356656,-4.5559744603208,49.2804959734646));
#33639=CARTESIAN_POINT('Ctrl Pts',(1.98992816161218,-4.49770707962655,49.2886524531658));
#33640=CARTESIAN_POINT('Ctrl Pts',(2.0793558104611,-4.45814145347065,49.294190993302));
#33641=CARTESIAN_POINT('Ctrl Pts',(2.16759437950105,-4.41591169874794,49.2997295334382));
#33642=CARTESIAN_POINT('Ctrl Pts',(2.25448517276978,-4.37109593446097,49.3052680735744));
#33643=CARTESIAN_POINT('Ctrl Pts',(2.38247563376097,-4.30508214732678,49.313426363752));
#33644=CARTESIAN_POINT('Ctrl Pts',(2.50758830220511,-4.23343076051948,49.3215846539296));
#33645=CARTESIAN_POINT('Ctrl Pts',(2.62932987891126,-4.15641762222764,49.3297429441072));
#33646=CARTESIAN_POINT('Ctrl Pts',(2.75104685793632,-4.07942004431104,49.337899585916));
#33647=CARTESIAN_POINT('Ctrl Pts',(2.86939382167824,-3.99706305474322,49.3460562277248));
#33648=CARTESIAN_POINT('Ctrl Pts',(2.98390494230295,-3.90966678347401,49.3542128695336));
#33649=CARTESIAN_POINT('Ctrl Pts',(3.09842010979685,-3.82226742358532,49.3623697996014));
#33650=CARTESIAN_POINT('Ctrl Pts',(3.20909889490924,-3.72982862549775,49.3705267296692));
#33651=CARTESIAN_POINT('Ctrl Pts',(3.31550675515293,-3.63271221252597,49.378683659737));
#33652=CARTESIAN_POINT('Ctrl Pts',(3.42190831197147,-3.53560155256941,49.3868401066018));
#33653=CARTESIAN_POINT('Ctrl Pts',(3.52403920376839,-3.43381405815351,49.3949965534665));
#33654=CARTESIAN_POINT('Ctrl Pts',(3.62150015463472,-3.32774994440398,49.4031530003313));
#33655=CARTESIAN_POINT('Ctrl Pts',(3.71898476532931,-3.22166008230402,49.4113114272725));
#33656=CARTESIAN_POINT('Ctrl Pts',(3.81179694326111,-3.11129177243436,49.4194698542138));
#33657=CARTESIAN_POINT('Ctrl Pts',(3.89957586233266,-2.99708043876244,49.427628281155));
#33658=CARTESIAN_POINT('Ctrl Pts',(3.95906105316276,-2.91968277825017,49.4331570070564));
#33659=CARTESIAN_POINT('Ctrl Pts',(4.01623559033989,-2.84052098032081,49.4386857329579));
#33660=CARTESIAN_POINT('Ctrl Pts',(4.07099804335122,-2.75973875457996,49.4442144588593));
#33661=CARTESIAN_POINT('Ctrl Pts',(4.15172859067097,-2.64064998227064,49.4523648802423));
#33662=CARTESIAN_POINT('Ctrl Pts',(4.22724559219509,-2.51799334936182,49.4605153016252));
#33663=CARTESIAN_POINT('Ctrl Pts',(4.2972481714216,-2.39224606086283,49.4686657230081));
#33664=CARTESIAN_POINT('Ctrl Pts',(4.36723626350179,-2.26652479596736,49.4768144576482));
#33665=CARTESIAN_POINT('Ctrl Pts',(4.43171204672463,-2.13771444450357,49.4849631922884));
#33666=CARTESIAN_POINT('Ctrl Pts',(4.49041994060349,-2.00631797567847,49.4931119269285));
#33667=CARTESIAN_POINT('Ctrl Pts',(4.54913005609664,-1.8749165345702,49.5012609699316));
#33668=CARTESIAN_POINT('Ctrl Pts',(4.60207170512697,-1.74092908514969,49.5094100129348));
#33669=CARTESIAN_POINT('Ctrl Pts',(4.64903671980356,-1.60488025734576,49.517559055938));
#33670=CARTESIAN_POINT('Ctrl Pts',(4.69599911974273,-1.46883900394509,49.5257076452501));
#33671=CARTESIAN_POINT('Ctrl Pts',(4.73698544253774,-1.33073691938958,49.5338562345622));
#33672=CARTESIAN_POINT('Ctrl Pts',(4.77183685689096,-1.19111547455192,49.5420048238743));
#33673=CARTESIAN_POINT('Ctrl Pts',(4.80669724594076,-1.05145807535979,49.5501555115551));
#33674=CARTESIAN_POINT('Ctrl Pts',(4.83541948825201,-0.910280859824225,
49.5583061992359));
#33675=CARTESIAN_POINT('Ctrl Pts',(4.8578953623635,-0.768137820203664,49.5664568869167));
#33676=CARTESIAN_POINT('Ctrl Pts',(4.87324932407909,-0.671035532762169,
49.5720248726594));
#33677=CARTESIAN_POINT('Ctrl Pts',(4.88568936452691,-0.573482777099811,
49.577592858402));
#33678=CARTESIAN_POINT('Ctrl Pts',(4.89519482048859,-0.475658209181462,
49.5831608441447));
#33679=CARTESIAN_POINT('Ctrl Pts',(4.90914294322574,-0.33211232505609,49.5913311990283));
#33680=CARTESIAN_POINT('Ctrl Pts',(4.91677519099054,-0.187927578512104,
49.5995015539119));
#33681=CARTESIAN_POINT('Ctrl Pts',(4.91805612251975,-0.0436696490248933,
49.6076719087955));
#33682=CARTESIAN_POINT('Ctrl Pts',(4.91933680114459,0.100559798486057,49.6158406505418));
#33683=CARTESIAN_POINT('Ctrl Pts',(4.91426866240652,0.244862068010121,49.624009392288));
#33684=CARTESIAN_POINT('Ctrl Pts',(4.90286836852894,0.388670584657962,49.6321781340343));
#33685=CARTESIAN_POINT('Ctrl Pts',(4.89146776839561,0.532482964555806,49.6403470952244));
#33686=CARTESIAN_POINT('Ctrl Pts',(4.87373469525807,0.675801233489329,49.6485160564145));
#33687=CARTESIAN_POINT('Ctrl Pts',(4.84973780482396,0.818062520203257,49.6566850176046));
#33688=CARTESIAN_POINT('Ctrl Pts',(4.82574253298665,0.960314211354579,49.664853427796));
#33689=CARTESIAN_POINT('Ctrl Pts',(4.7954843449171,1.10150873532644,49.6730218379874));
#33690=CARTESIAN_POINT('Ctrl Pts',(4.75908327686338,1.24109202977835,49.6811902481789));
#33691=CARTESIAN_POINT('Ctrl Pts',(4.72267435320067,1.38070544729643,49.6893604211712));
#33692=CARTESIAN_POINT('Ctrl Pts',(4.68011998404698,1.51870661870121,49.6975305941636));
#33693=CARTESIAN_POINT('Ctrl Pts',(4.63159063780015,1.6545546912514,49.7057007671559));
#33694=CARTESIAN_POINT('Ctrl Pts',(4.59910683404554,1.74548651849501,49.7111695879139));
#33695=CARTESIAN_POINT('Ctrl Pts',(4.56394699150573,1.83545393997024,49.7166384086718));
#33696=CARTESIAN_POINT('Ctrl Pts',(4.52617449794241,1.92429921703351,49.7221072294298));
#33697=CARTESIAN_POINT('Ctrl Pts',(4.47001670612233,2.05638884371259,49.7302379316592));
#33698=CARTESIAN_POINT('Ctrl Pts',(4.40806101688729,2.18604583523466,49.7383686338887));
#33699=CARTESIAN_POINT('Ctrl Pts',(4.34054380093662,2.31276081224381,49.7464993361181));
#33700=CARTESIAN_POINT('Ctrl Pts',(4.2730406525832,2.4394493874644,49.7546283442693));
#33701=CARTESIAN_POINT('Ctrl Pts',(4.1999784481678,2.5631968720442,49.7627573524206));
#33702=CARTESIAN_POINT('Ctrl Pts',(4.12163978233728,2.68351794612123,49.7708863605718));
#33703=CARTESIAN_POINT('Ctrl Pts',(4.04329642595676,2.80384622445695,49.7790158554497));
#33704=CARTESIAN_POINT('Ctrl Pts',(3.95967615792387,2.92074739588798,49.7871453503276));
#33705=CARTESIAN_POINT('Ctrl Pts',(3.87110549478319,3.03376421476018,49.7952748452055));
#33706=CARTESIAN_POINT('Ctrl Pts',(3.78253822332834,3.14677670581624,49.8034040287762));
#33707=CARTESIAN_POINT('Ctrl Pts',(3.68902114658794,3.2559048763766,49.8115332123468));
#33708=CARTESIAN_POINT('Ctrl Pts',(3.59092166438334,3.36072383018337,49.8196623959174));
#33709=CARTESIAN_POINT('Ctrl Pts',(3.49279204407795,3.46557498644548,49.827794076934));
#33710=CARTESIAN_POINT('Ctrl Pts',(3.39007743703124,3.5661140331609,49.8359257579506));
#33711=CARTESIAN_POINT('Ctrl Pts',(3.28318318799768,3.66195183154413,49.8440574389671));
#33712=CARTESIAN_POINT('Ctrl Pts',(3.20870931069034,3.72872261203726,49.849722830883));
#33713=CARTESIAN_POINT('Ctrl Pts',(3.13220742683228,3.79321216257162,49.8553882227989));
#33714=CARTESIAN_POINT('Ctrl Pts',(3.05382444009089,3.85530016361937,49.8610536147148));
#33715=CARTESIAN_POINT('Ctrl Pts',(2.94028011452916,3.94523983672345,49.8692604097207));
#33716=CARTESIAN_POINT('Ctrl Pts',(2.82274158545749,4.03017446421762,49.8774672047265));
#33717=CARTESIAN_POINT('Ctrl Pts',(2.70166900979517,4.10976491103961,49.8856739997324));
#33718=CARTESIAN_POINT('Ctrl Pts',(2.58062228977396,4.18933836093213,49.893879042137));
#33719=CARTESIAN_POINT('Ctrl Pts',(2.45604330140261,4.26356972828012,49.9020840845417));
#33720=CARTESIAN_POINT('Ctrl Pts',(2.32842119384962,4.33216317865936,49.9102891269463));
#33721=CARTESIAN_POINT('Ctrl Pts',(2.20080501859814,4.40075344058608,49.9184937879532));
#33722=CARTESIAN_POINT('Ctrl Pts',(2.07014629201985,4.46370615109296,49.92669844896));
#33723=CARTESIAN_POINT('Ctrl Pts',(1.93695922718213,4.52077117478136,49.9349031099669));
#33724=CARTESIAN_POINT('Ctrl Pts',(1.80378819378023,4.57782932967761,49.9431067833967));
#33725=CARTESIAN_POINT('Ctrl Pts',(1.66808972996679,4.62900108541544,49.9513104568264));
#33726=CARTESIAN_POINT('Ctrl Pts',(1.53039860575751,4.67408420655806,49.9595141302562));
#33727=CARTESIAN_POINT('Ctrl Pts',(1.39269508346662,4.71917138710696,49.9677185423669));
#33728=CARTESIAN_POINT('Ctrl Pts',(1.25299885180337,4.75816873474349,49.9759229544776));
#33729=CARTESIAN_POINT('Ctrl Pts',(1.11186100265542,4.79092351987319,49.9841273665884));
#33730=CARTESIAN_POINT('Ctrl Pts',(1.02084374227571,4.8120464916687,49.9894182443922));
#33731=CARTESIAN_POINT('Ctrl Pts',(0.929227268209053,4.8305743615327,49.9947091221961));
#33732=CARTESIAN_POINT('Ctrl Pts',(0.837162017642339,4.84647736182859,50.));
#33733=CARTESIAN_POINT('Ctrl Pts',(-4.91824999915337,-9.12569049791451E-5,
48.7349629410195));
#33734=CARTESIAN_POINT('Ctrl Pts',(-4.91825434592466,0.234176033562846,
48.7218012036652));
#33735=CARTESIAN_POINT('Ctrl Pts',(-4.9015207571834,0.468144306462426,48.7087390737667));
#33736=CARTESIAN_POINT('Ctrl Pts',(-4.85907259687595,0.763339949708897,
48.6919547342511));
#33737=CARTESIAN_POINT('Ctrl Pts',(-4.84873434829882,0.826468084567931,
48.6883485203186));
#33738=CARTESIAN_POINT('Ctrl Pts',(-4.82568931602746,0.951806148915575,
48.6811469871145));
#33739=CARTESIAN_POINT('Ctrl Pts',(-4.81300330664162,1.01400758264125,48.6775524728086));
#33740=CARTESIAN_POINT('Ctrl Pts',(-4.78816591077663,1.12479159538779,48.6711086002473));
#33741=CARTESIAN_POINT('Ctrl Pts',(-4.7764703200144,1.17346480007204,48.6682628776392));
#33742=CARTESIAN_POINT('Ctrl Pts',(-4.76403458580012,1.22194825086837,48.6654127926075));
#33743=CARTESIAN_POINT('Origin',(0.,0.,0.));
#33744=CARTESIAN_POINT('',(-4.03656765912811,4.32587940999471,49.0832499999999));
#33745=CARTESIAN_POINT('Ctrl Pts',(-5.91653912833173,0.000142916515667024,
47.5616248077951));
#33746=CARTESIAN_POINT('Ctrl Pts',(-5.91592149880519,-0.686681391260685,
47.5939532561295));
#33747=CARTESIAN_POINT('Ctrl Pts',(-5.62516687896037,-2.35799619906392,
47.6725971662253));
#33748=CARTESIAN_POINT('Ctrl Pts',(-4.08414406137617,-4.62189440864751,
47.7975565380834));
#33749=CARTESIAN_POINT('Ctrl Pts',(-1.37510285831354,-6.01258952044505,
47.9365029233684));
#33750=CARTESIAN_POINT('Ctrl Pts',(1.66912564744111,-5.93768980797298,48.0754493086537));
#33751=CARTESIAN_POINT('Ctrl Pts',(4.30649751429276,-4.41545237791594,48.2143956939387));
#33752=CARTESIAN_POINT('Ctrl Pts',(5.8941419046702,-1.81692926751613,48.3533420792238));
#33753=CARTESIAN_POINT('Ctrl Pts',(6.04506355860129,1.22447831006187,48.492288464509));
#33754=CARTESIAN_POINT('Ctrl Pts',(4.72247474170802,3.96741385956337,48.631234849794));
#33755=CARTESIAN_POINT('Ctrl Pts',(2.24876208132675,5.74327526323482,48.7701812350792));
#33756=CARTESIAN_POINT('Ctrl Pts',(-0.7730959231624,6.11918790880795,48.9091276203643));
#33757=CARTESIAN_POINT('Ctrl Pts',(-2.90114233776988,5.28126301364285,49.0134838753379));
#33758=CARTESIAN_POINT('Ctrl Pts',(-3.8546249267777,4.4960048839609,49.0715246685497));
#33759=CARTESIAN_POINT('Ctrl Pts',(-4.03656765912811,4.32587940999471,49.0832499999999));
#33760=CARTESIAN_POINT('',(0.902187534995306,5.84756258745463,49.0832469945976));
#33761=CARTESIAN_POINT('Origin',(0.,0.,49.08325));
#33762=CARTESIAN_POINT('Ctrl Pts',(0.902187534995306,5.84756258745463,49.0832469945976));
#33763=CARTESIAN_POINT('Ctrl Pts',(1.0757113845097,5.82079056890589,49.0749812014674));
#33764=CARTESIAN_POINT('Ctrl Pts',(1.24800634179856,5.786296037608,49.0667154083371));
#33765=CARTESIAN_POINT('Ctrl Pts',(1.41841873069125,5.74421612292959,49.0584496152068));
#33766=CARTESIAN_POINT('Ctrl Pts',(1.45137406665876,5.7360784650121,49.0568511281988));
#33767=CARTESIAN_POINT('Ctrl Pts',(1.48425903291376,5.7276572809102,49.0552526411908));
#33768=CARTESIAN_POINT('Ctrl Pts',(1.51706895429147,5.71895378110586,49.0536541541828));
#33769=CARTESIAN_POINT('Ctrl Pts',(1.67680621552835,5.67658021958721,49.0458718149983));
#33770=CARTESIAN_POINT('Ctrl Pts',(1.83479720312141,5.62750197905755,49.0380894758137));
#33771=CARTESIAN_POINT('Ctrl Pts',(1.99047581665468,5.5718880629292,49.0303071366292));
#33772=CARTESIAN_POINT('Ctrl Pts',(2.1461224191251,5.51628558228658,49.0225263976705));
#33773=CARTESIAN_POINT('Ctrl Pts',(2.29945729458024,5.45415021512252,49.0147456587119));
#33774=CARTESIAN_POINT('Ctrl Pts',(2.44993138878728,5.38570021006877,49.0069649197533));
#33775=CARTESIAN_POINT('Ctrl Pts',(2.60041021113751,5.31724805420344,48.9991839363111));
#33776=CARTESIAN_POINT('Ctrl Pts',(2.74802777889052,5.24248099225811,48.9914029528689));
#33777=CARTESIAN_POINT('Ctrl Pts',(2.89225616972135,5.1616649262819,48.9836219694266));
#33778=CARTESIAN_POINT('Ctrl Pts',(3.03647469212574,5.08085438992021,48.9758415183766));
#33779=CARTESIAN_POINT('Ctrl Pts',(3.17730422203144,4.99399583444173,48.9680610673265));
#33780=CARTESIAN_POINT('Ctrl Pts',(3.31424242478615,4.90140058679635,48.9602806162765));
#33781=CARTESIAN_POINT('Ctrl Pts',(3.45121716393948,4.80878063386925,48.952498089329));
#33782=CARTESIAN_POINT('Ctrl Pts',(3.58429823450697,4.7104211082961,48.9447155623815));
#33783=CARTESIAN_POINT('Ctrl Pts',(3.71301247910061,4.60667655610236,48.9369330354341));
#33784=CARTESIAN_POINT('Ctrl Pts',(3.83594526161443,4.50759190147001,48.9295000765128));
#33785=CARTESIAN_POINT('Ctrl Pts',(3.9548947117549,4.40359555872854,48.9220671175916));
#33786=CARTESIAN_POINT('Ctrl Pts',(4.06947700835253,4.29503055181102,48.9146341586704));
#33787=CARTESIAN_POINT('Ctrl Pts',(4.18955912618769,4.18125454678624,48.9068444260891));
#33788=CARTESIAN_POINT('Ctrl Pts',(4.3048878997653,4.06241941215262,48.8990546935078));
#33789=CARTESIAN_POINT('Ctrl Pts',(4.41504675538643,3.93894563433563,48.8912649609265));
#33790=CARTESIAN_POINT('Ctrl Pts',(4.52518422084792,3.81549583211103,48.883476740921));
#33791=CARTESIAN_POINT('Ctrl Pts',(4.63015355899246,3.68740942199132,48.8756885209156));
#33792=CARTESIAN_POINT('Ctrl Pts',(4.72957676690374,3.55514193365952,48.8679003009101));
#33793=CARTESIAN_POINT('Ctrl Pts',(4.82900391645889,3.42286920156877,48.8601117721399));
#33794=CARTESIAN_POINT('Ctrl Pts',(4.92288430087925,3.28641531243443,48.8523232433696));
#33795=CARTESIAN_POINT('Ctrl Pts',(5.01088130159669,3.14626749400121,48.8445347145993));
#33796=CARTESIAN_POINT('Ctrl Pts',(5.09887251503693,3.00612889263526,48.8367466980553));
#33797=CARTESIAN_POINT('Ctrl Pts',(5.18098094941818,2.86229711859535,48.8289586815112));
#33798=CARTESIAN_POINT('Ctrl Pts',(5.25691420862224,2.71528701350071,48.8211706649672));
#33799=CARTESIAN_POINT('Ctrl Pts',(5.33286733050105,2.56823845340056,48.8133806112284));
#33800=CARTESIAN_POINT('Ctrl Pts',(5.4026419011453,2.41801018389847,48.8055905574896));
#33801=CARTESIAN_POINT('Ctrl Pts',(5.46599183768833,2.26514100947922,48.7978005037508));
#33802=CARTESIAN_POINT('Ctrl Pts',(5.52613276935194,2.12001545649662,48.7904050568865));
#33803=CARTESIAN_POINT('Ctrl Pts',(5.58048372723525,1.97251016469156,48.7830096100221));
#33804=CARTESIAN_POINT('Ctrl Pts',(5.62887457408974,1.82310218903551,48.7756141631578));
#33805=CARTESIAN_POINT('Ctrl Pts',(5.67983320173127,1.66576612461353,48.7678262890557));
#33806=CARTESIAN_POINT('Ctrl Pts',(5.72420011388111,1.50626403321614,48.7600384149535));
#33807=CARTESIAN_POINT('Ctrl Pts',(5.76181081107359,1.34516420555095,48.7522505408513));
#33808=CARTESIAN_POINT('Ctrl Pts',(5.79941412039692,1.18409602272447,48.7444641965212));
#33809=CARTESIAN_POINT('Ctrl Pts',(5.83026379015604,1.02143104084788,48.7366778521911));
#33810=CARTESIAN_POINT('Ctrl Pts',(5.85424595748507,0.857749865502559,48.7288915078611));
#33811=CARTESIAN_POINT('Ctrl Pts',(5.87822904954059,0.694062378787835,48.7211048632979));
#33812=CARTESIAN_POINT('Ctrl Pts',(5.89534405906009,0.529358935806454,48.7133182187348));
#33813=CARTESIAN_POINT('Ctrl Pts',(5.90552863021208,0.36422817058195,48.7055315741717));
#33814=CARTESIAN_POINT('Ctrl Pts',(5.91571253028362,0.19910828613257,48.6977454426852));
#33815=CARTESIAN_POINT('Ctrl Pts',(5.91896688628404,0.0335614547822753,
48.6899593111986));
#33816=CARTESIAN_POINT('Ctrl Pts',(5.91528138719896,-0.131820608243138,
48.6821731797121));
#33817=CARTESIAN_POINT('Ctrl Pts',(5.91159491591334,-0.297246297525582,
48.6743849943162));
#33818=CARTESIAN_POINT('Ctrl Pts',(5.90096493665034,-0.462506811887508,
48.6665968089203));
#33819=CARTESIAN_POINT('Ctrl Pts',(5.8834332717793,-0.627011562110531,48.6588086235243));
#33820=CARTESIAN_POINT('Ctrl Pts',(5.86676458812731,-0.783418706605302,
48.651403804898));
#33821=CARTESIAN_POINT('Ctrl Pts',(5.84385736427122,-0.939142439080653,
48.6439989862717));
#33822=CARTESIAN_POINT('Ctrl Pts',(5.81479093755537,-1.09368044465644,48.6365941676453));
#33823=CARTESIAN_POINT('Ctrl Pts',(5.78422191898618,-1.25620730797797,48.6288065561751));
#33824=CARTESIAN_POINT('Ctrl Pts',(5.74682905763876,-1.41748092584339,48.6210189447049));
#33825=CARTESIAN_POINT('Ctrl Pts',(5.70273990443529,-1.57692363317358,48.6132313332347));
#33826=CARTESIAN_POINT('Ctrl Pts',(5.6586594545948,-1.73633486591978,48.605445259068));
#33827=CARTESIAN_POINT('Ctrl Pts',(5.60788543554517,-1.89391560142245,48.5976591849012));
#33828=CARTESIAN_POINT('Ctrl Pts',(5.55059575249572,-2.04910159701183,48.5898731107345));
#33829=CARTESIAN_POINT('Ctrl Pts',(5.49330392747658,-2.2042933947576,48.5820867454589));
#33830=CARTESIAN_POINT('Ctrl Pts',(5.42949605793907,-2.35708997222679,48.5743003801833));
#33831=CARTESIAN_POINT('Ctrl Pts',(5.35939911575957,-2.50694469035429,48.5665140149077));
#33832=CARTESIAN_POINT('Ctrl Pts',(5.2893068326131,-2.65678944830293,48.5587281671573));
#33833=CARTESIAN_POINT('Ctrl Pts',(5.21292644883726,-2.80369244871058,48.5509423194069));
#33834=CARTESIAN_POINT('Ctrl Pts',(5.13053210744219,-2.94712925692185,48.5431564716565));
#33835=CARTESIAN_POINT('Ctrl Pts',(5.04811608039854,-3.09060381675739,48.5353685747222));
#33836=CARTESIAN_POINT('Ctrl Pts',(4.95968309050393,-3.23061008316695,48.5275806777879));
#33837=CARTESIAN_POINT('Ctrl Pts',(4.865552515652,-3.36664956298283,48.5197927808536));
#33838=CARTESIAN_POINT('Ctrl Pts',(4.77603539145568,-3.49602158721023,48.5123865779467));
#33839=CARTESIAN_POINT('Ctrl Pts',(4.68136595057938,-3.62180613137823,48.5049803750398));
#33840=CARTESIAN_POINT('Ctrl Pts',(4.58185447348852,-3.74359989131761,48.4975741721329));
#33841=CARTESIAN_POINT('Ctrl Pts',(4.47720858649184,-3.87167774135172,48.4897858376098));
#33842=CARTESIAN_POINT('Ctrl Pts',(4.36717040269952,-3.99538786321501,48.4819975030867));
#33843=CARTESIAN_POINT('Ctrl Pts',(4.2521285355429,-4.1142840786365,48.4742091685636));
#33844=CARTESIAN_POINT('Ctrl Pts',(4.1371092096297,-4.23315699759559,48.4664223600827));
#33845=CARTESIAN_POINT('Ctrl Pts',(4.017088378608,-4.34721766268525,48.4586355516018));
#33846=CARTESIAN_POINT('Ctrl Pts',(3.89249243811587,-4.45605578754472,48.4508487431209));
#33847=CARTESIAN_POINT('Ctrl Pts',(3.76789167283227,-4.56489812699781,48.4430616331075));
#33848=CARTESIAN_POINT('Ctrl Pts',(3.63871568159011,-4.66851730840554,48.4352745230942));
#33849=CARTESIAN_POINT('Ctrl Pts',(3.5054255112133,-4.76654199056664,48.4274874130808));
#33850=CARTESIAN_POINT('Ctrl Pts',(3.37214412699704,-4.86456021118153,48.4197008163745));
#33851=CARTESIAN_POINT('Ctrl Pts',(3.23474936382851,-4.95698448132655,48.4119142196683));
#33852=CARTESIAN_POINT('Ctrl Pts',(3.09373305327206,-5.04348553657011,48.4041276229621));
#33853=CARTESIAN_POINT('Ctrl Pts',(2.9526796341123,-5.13000935466524,48.396338977204));
#33854=CARTESIAN_POINT('Ctrl Pts',(2.8080030347374,-5.21060667441763,48.3885503314459));
#33855=CARTESIAN_POINT('Ctrl Pts',(2.66022238318807,-5.28499266172482,48.3807616856879));
#33856=CARTESIAN_POINT('Ctrl Pts',(2.51976834871897,-5.35569076675905,48.3733591826653));
#33857=CARTESIAN_POINT('Ctrl Pts',(2.37651082322848,-5.42077838556117,48.3659566796428));
#33858=CARTESIAN_POINT('Ctrl Pts',(2.23091453197799,-5.48005026560062,48.3585541766202));
#33859=CARTESIAN_POINT('Ctrl Pts',(2.07774094308078,-5.54240684424937,48.3507664236146));
#33860=CARTESIAN_POINT('Ctrl Pts',(1.9219238572207,-5.59834851440998,48.342978670609));
#33861=CARTESIAN_POINT('Ctrl Pts',(1.76401794960577,-5.64766954025894,48.3351909176035));
#33862=CARTESIAN_POINT('Ctrl Pts',(1.60614314965164,-5.69698084980428,48.3274046987949));
#33863=CARTESIAN_POINT('Ctrl Pts',(1.44618065387223,-5.73967402222281,48.3196184799864));
#33864=CARTESIAN_POINT('Ctrl Pts',(1.28470113377979,-5.77559291842534,48.3118322611779));
#33865=CARTESIAN_POINT('Ctrl Pts',(1.123215504986,-5.81151317342439,48.30404574782));
#33866=CARTESIAN_POINT('Ctrl Pts',(0.960213048135258,-5.84065856614888,
48.2962592344622));
#33867=CARTESIAN_POINT('Ctrl Pts',(0.796276219423017,-5.862923736915,48.2884727211043));
#33868=CARTESIAN_POINT('Ctrl Pts',(0.632350253164033,-5.88518743239105,
48.2806867236808));
#33869=CARTESIAN_POINT('Ctrl Pts',(0.467490355659226,-5.90057177529173,
48.2729007262572));
#33870=CARTESIAN_POINT('Ctrl Pts',(0.302285873648315,-5.90902308449482,
48.2651147288337));
#33871=CARTESIAN_POINT('Ctrl Pts',(0.137037885705147,-5.91747661931602,
48.2573266809992));
#33872=CARTESIAN_POINT('Ctrl Pts',(-0.0285545487879778,-5.91899345383947,
48.2495386331648));
#33873=CARTESIAN_POINT('Ctrl Pts',(-0.193899382391169,-5.91357198248303,
48.2417505853303));
#33874=CARTESIAN_POINT('Ctrl Pts',(-0.351121822789253,-5.90841683527564,
48.2343451172562));
#33875=CARTESIAN_POINT('Ctrl Pts',(-0.508120141164401,-5.89698870428187,
48.226939649182));
#33876=CARTESIAN_POINT('Ctrl Pts',(-0.664387412158191,-5.87932988775641,
48.2195341811079));
#33877=CARTESIAN_POINT('Ctrl Pts',(-0.828728543247588,-5.86075869326994,
48.2117460947619));
#33878=CARTESIAN_POINT('Ctrl Pts',(-0.992319878645803,-5.83528928235357,
48.2039580084159));
#33879=CARTESIAN_POINT('Ctrl Pts',(-1.15457589028596,-5.80300655488777,
48.1961699220699));
#33880=CARTESIAN_POINT('Ctrl Pts',(-1.31680002986572,-5.77073016874041,
48.1883833655431));
#33881=CARTESIAN_POINT('Ctrl Pts',(-1.47768905585395,-5.73164319875144,
48.1805968090163));
#33882=CARTESIAN_POINT('Ctrl Pts',(-1.63666713806711,-5.68588174707065,
48.1728102524895));
#33883=CARTESIAN_POINT('Ctrl Pts',(-1.79565130644826,-5.64011854350132,
48.1650233978695));
#33884=CARTESIAN_POINT('Ctrl Pts',(-1.95272407652092,-5.58768043153087,
48.1572365432494));
#33885=CARTESIAN_POINT('Ctrl Pts',(-2.10732357918337,-5.52875373797005,
48.1494496886294));
#33886=CARTESIAN_POINT('Ctrl Pts',(-2.26191286346188,-5.46983093921852,
48.141663348688));
#33887=CARTESIAN_POINT('Ctrl Pts',(-2.41402890890177,-5.40442053102927,
48.1338770087467));
#33888=CARTESIAN_POINT('Ctrl Pts',(-2.5631285345683,-5.33275751162396,48.1260906688053));
#33889=CARTESIAN_POINT('Ctrl Pts',(-2.71226740054379,-5.26107563181568,
48.118302279641));
#33890=CARTESIAN_POINT('Ctrl Pts',(-2.85838797140062,-5.18313798933969,
48.1105138904766));
#33891=CARTESIAN_POINT('Ctrl Pts',(-3.0009696227234,-5.09922659684695,48.1027255013122));
#33892=CARTESIAN_POINT('Ctrl Pts',(-3.13651010510691,-5.01945903552036,
48.0953217294065));
#33893=CARTESIAN_POINT('Ctrl Pts',(-3.26885253438473,-4.9342936286528,48.0879179575009));
#33894=CARTESIAN_POINT('Ctrl Pts',(-3.39757238832685,-4.84400995339388,
48.0805141855952));
#33895=CARTESIAN_POINT('Ctrl Pts',(-3.53297126245669,-4.74904163570251,
48.0727262465194));
#33896=CARTESIAN_POINT('Ctrl Pts',(-3.66441005731167,-4.64837580729459,
48.0649383074436));
#33897=CARTESIAN_POINT('Ctrl Pts',(-3.79141533198079,-4.54236726200348,
48.0571503683679));
#33898=CARTESIAN_POINT('Ctrl Pts',(-3.91839562909804,-4.43637956493262,
48.0493639609108));
#33899=CARTESIAN_POINT('Ctrl Pts',(-4.04094390058947,-4.32505145213363,
48.0415775534537));
#33900=CARTESIAN_POINT('Ctrl Pts',(-4.15861972835657,-4.20877803137959,
48.0337911459966));
#33901=CARTESIAN_POINT('Ctrl Pts',(-4.27630004069902,-4.09250017949534,
48.0260044418029));
#33902=CARTESIAN_POINT('Ctrl Pts',(-4.38910730767105,-3.97127686431734,
48.0182177376092));
#33903=CARTESIAN_POINT('Ctrl Pts',(-4.49663740936991,-3.84554060843921,
48.0104310334154));
#33904=CARTESIAN_POINT('Ctrl Pts',(-4.60416039755778,-3.71981267047602,
48.0026448443408));
#33905=CARTESIAN_POINT('Ctrl Pts',(-4.70640671145677,-3.58957263220266,
47.9948586552661));
#33906=CARTESIAN_POINT('Ctrl Pts',(-4.80301193638849,-3.45528680450837,
47.9870724661915));
#33907=CARTESIAN_POINT('Ctrl Pts',(-4.89964259538731,-3.32096562225894,
47.9792842271816));
#33908=CARTESIAN_POINT('Ctrl Pts',(-4.99062900939446,-3.1825967805922,47.9714959881716));
#33909=CARTESIAN_POINT('Ctrl Pts',(-5.07564907232607,-3.04067707214947,
47.9637077491617));
#33910=CARTESIAN_POINT('Ctrl Pts',(-5.15648027556416,-2.90574961619296,
47.9563032294688));
#33911=CARTESIAN_POINT('Ctrl Pts',(-5.23191875230041,-2.76761299210775,
47.9488987097758));
#33912=CARTESIAN_POINT('Ctrl Pts',(-5.30172552274323,-2.62671601890899,
47.9414941900828));
#33913=CARTESIAN_POINT('Ctrl Pts',(-5.37493451551398,-2.47895204949891,
47.9337287910357));
#33914=CARTESIAN_POINT('Ctrl Pts',(-5.44197671386717,-2.32809613211981,
47.9259633919887));
#33915=CARTESIAN_POINT('Ctrl Pts',(-5.50260701658285,-2.17468309956951,
47.9181979929416));
#33916=CARTESIAN_POINT('Ctrl Pts',(-5.56322478575962,-2.0213017806694,47.9104341991633));
#33917=CARTESIAN_POINT('Ctrl Pts',(-5.61743318505499,-1.86536470170965,
47.902670405385));
#33918=CARTESIAN_POINT('Ctrl Pts',(-5.66503538115071,-1.70742633598366,
47.8949066116067));
#33919=CARTESIAN_POINT('Ctrl Pts',(-5.71263811119004,-1.549486198697,47.8871427307436));
#33920=CARTESIAN_POINT('Ctrl Pts',(-5.75363439281445,-1.38954503810943,
47.8793788498805));
#33921=CARTESIAN_POINT('Ctrl Pts',(-5.78787717610237,-1.22817277158113,
47.8716149690174));
#33922=CARTESIAN_POINT('Ctrl Pts',(-5.82211830257874,-1.06680831292969,
47.8638514638039));
#33923=CARTESIAN_POINT('Ctrl Pts',(-5.84960651834727,-0.904013203300888,
47.8560879585904));
#33924=CARTESIAN_POINT('Ctrl Pts',(-5.870245801473,-0.74036801172702,47.8483244533769));
#33925=CARTESIAN_POINT('Ctrl Pts',(-5.89088955153219,-0.576687402635144,
47.840559267918));
#33926=CARTESIAN_POINT('Ctrl Pts',(-5.90468136710913,-0.412156664851667,
47.832794082459));
#33927=CARTESIAN_POINT('Ctrl Pts',(-5.91157696882471,-0.247362697594452,
47.8250288970001));
#33928=CARTESIAN_POINT('Ctrl Pts',(-5.91502652397537,-0.16492378914296,
47.8211443287491));
#33929=CARTESIAN_POINT('Ctrl Pts',(-5.91675108445212,-0.0824190692800998,
47.8172597604981));
#33930=CARTESIAN_POINT('Ctrl Pts',(-5.91674999948831,7.78145712749811E-5,
47.8133751922472));
#33931=CARTESIAN_POINT('Origin',(0.,0.,49.5));
#33932=CARTESIAN_POINT('',(1.67563808492399,4.71079034076956,50.0000691378445));
#33933=CARTESIAN_POINT('Ctrl Pts',(1.67563808492399,4.71079034076956,50.0000691378444));
#33934=CARTESIAN_POINT('Ctrl Pts',(1.81473787532752,4.66673395805934,49.9949609527894));
#33935=CARTESIAN_POINT('Ctrl Pts',(1.95192304800988,4.61660905950312,49.9898325023651));
#33936=CARTESIAN_POINT('Ctrl Pts',(2.08679675191645,4.5605717909821,49.9846699266638));
#33937=CARTESIAN_POINT('Ctrl Pts',(2.18013465240617,4.52179180020974,49.9810972215098));
#33938=CARTESIAN_POINT('Ctrl Pts',(2.27236538682205,4.48017983818195,49.9775087411235));
#33939=CARTESIAN_POINT('Ctrl Pts',(2.36335535052691,4.43578180111657,49.9739072133534));
#33940=CARTESIAN_POINT('Ctrl Pts',(2.39724229344457,4.41924685938859,49.9725659141486));
#33941=CARTESIAN_POINT('Ctrl Pts',(2.43095712394704,4.40232543880356,49.9712228642745));
#33942=CARTESIAN_POINT('Ctrl Pts',(2.4644928777425,4.38501972948132,49.9698784137574));
#33943=CARTESIAN_POINT('Ctrl Pts',(2.48261127171451,4.37566995725381,49.9691520461828));
#33944=CARTESIAN_POINT('Ctrl Pts',(2.50067739438694,4.36620794637243,49.9684252705303));
#33945=CARTESIAN_POINT('Ctrl Pts',(2.51867750380479,4.35664094393442,49.9676986693424));
#33946=CARTESIAN_POINT('Ctrl Pts',(2.6509623677971,4.28633194819731,49.9623587940626));
#33947=CARTESIAN_POINT('Ctrl Pts',(2.77985412600453,4.2102669796089,49.9570193910659));
#33948=CARTESIAN_POINT('Ctrl Pts',(2.90498713229767,4.12869881484235,49.9517226559453));
#33949=CARTESIAN_POINT('Ctrl Pts',(2.98517938741253,4.0764253558088,49.9483282107334));
#33950=CARTESIAN_POINT('Ctrl Pts',(3.0638282861637,4.02189100982338,49.9449518083139));
#33951=CARTESIAN_POINT('Ctrl Pts',(3.14084006697321,3.96515302750838,49.941609459733));
#33952=CARTESIAN_POINT('Ctrl Pts',(3.26052055661263,3.87697912173403,49.9364152685259));
#33953=CARTESIAN_POINT('Ctrl Pts',(3.3762503040121,3.783482753799,49.9313021101912));
#33954=CARTESIAN_POINT('Ctrl Pts',(3.48774777220362,3.68497444840038,49.9262024865122));
#33955=CARTESIAN_POINT('Ctrl Pts',(3.59964773861427,3.58611053477017,49.9210844535412));
#33956=CARTESIAN_POINT('Ctrl Pts',(3.70728451516587,3.48219804431622,49.9159798531581));
#33957=CARTESIAN_POINT('Ctrl Pts',(3.81034263019071,3.37354157002801,49.9108454843505));
#33958=CARTESIAN_POINT('Ctrl Pts',(3.82681372888809,3.35617572249937,49.910024892053));
#33959=CARTESIAN_POINT('Ctrl Pts',(3.84316781368502,3.33868868374835,49.9092035945216));
#33960=CARTESIAN_POINT('Ctrl Pts',(3.85940353090415,3.32108168337155,49.9083814791383));
#33961=CARTESIAN_POINT('Ctrl Pts',(3.87395088755691,3.30530564400049,49.9076448559557));
#33962=CARTESIAN_POINT('Ctrl Pts',(3.88839828689456,3.28943859217021,49.9069078245672));
#33963=CARTESIAN_POINT('Ctrl Pts',(3.90273991934431,3.2734873277252,49.9061705797287));
#33964=CARTESIAN_POINT('Ctrl Pts',(4.00336138882482,3.16157261549479,49.900998040321));
#33965=CARTESIAN_POINT('Ctrl Pts',(4.09885594019099,3.04542909728232,49.8958086469949));
#33966=CARTESIAN_POINT('Ctrl Pts',(4.18899320504064,2.92546460240762,49.8905961980074));
#33967=CARTESIAN_POINT('Ctrl Pts',(4.27967435974525,2.8047762396429,49.8853522970102));
#33968=CARTESIAN_POINT('Ctrl Pts',(4.36493356340819,2.68022087265818,49.8800851496014));
#33969=CARTESIAN_POINT('Ctrl Pts',(4.44453028409552,2.55218579792693,49.8748169014774));
#33970=CARTESIAN_POINT('Ctrl Pts',(4.52372110061123,2.42480363917638,49.8695755188306));
#33971=CARTESIAN_POINT('Ctrl Pts',(4.59730749734601,2.29397740000137,49.8643332430544));
#33972=CARTESIAN_POINT('Ctrl Pts',(4.66504193211966,2.16005750620798,49.8591377514506));
#33973=CARTESIAN_POINT('Ctrl Pts',(4.68953272611782,2.11163598261943,49.8572592133775));
#33974=CARTESIAN_POINT('Ctrl Pts',(4.71325833516671,2.06280970337978,49.8553870226302));
#33975=CARTESIAN_POINT('Ctrl Pts',(4.73620649163542,2.0135941395332,49.8535241873519));
#33976=CARTESIAN_POINT('Ctrl Pts',(4.78178682276434,1.91584067947285,49.8498241668757));
#33977=CARTESIAN_POINT('Ctrl Pts',(4.82430078597844,1.81655097495366,49.8461607180028));
#33978=CARTESIAN_POINT('Ctrl Pts',(4.8636946286286,1.71586513965779,49.8425084955917));
#33979=CARTESIAN_POINT('Ctrl Pts',(4.87286993785393,1.69241417343309,49.8416578481878));
#33980=CARTESIAN_POINT('Ctrl Pts',(4.88187594172209,1.66888748460883,49.8408078339904));
#33981=CARTESIAN_POINT('Ctrl Pts',(4.89071188208244,1.64528687215975,49.839958177956));
#33982=CARTESIAN_POINT('Ctrl Pts',(4.89798164868161,1.6258694771678,49.839259123774));
#33983=CARTESIAN_POINT('Ctrl Pts',(4.90513662158331,1.60640097331495,49.8385602749155));
#33984=CARTESIAN_POINT('Ctrl Pts',(4.91217064536634,1.58689872257296,49.8378620703334));
#33985=CARTESIAN_POINT('Ctrl Pts',(4.96311473550224,1.44565319223368,49.8328053064864));
#33986=CARTESIAN_POINT('Ctrl Pts',(5.00779051564247,1.30244333780008,49.8277731701466));
#33987=CARTESIAN_POINT('Ctrl Pts',(5.04617351021521,1.15771482827818,49.8227255511406));
#33988=CARTESIAN_POINT('Ctrl Pts',(5.08523210610634,1.01043886843539,49.8175890860689));
#33989=CARTESIAN_POINT('Ctrl Pts',(5.11777433764025,0.861590382504143,49.8124364914983));
#33990=CARTESIAN_POINT('Ctrl Pts',(5.14375382774835,0.711627275063704,49.8072534416659));
#33991=CARTESIAN_POINT('Ctrl Pts',(5.16973623733982,0.561647315298723,49.8020698093807));
#33992=CARTESIAN_POINT('Ctrl Pts',(5.18915456037088,0.410552554862994,49.7968557639674));
#33993=CARTESIAN_POINT('Ctrl Pts',(5.20194190393592,0.258788407666574,49.7916249163614));
#33994=CARTESIAN_POINT('Ctrl Pts',(5.21263748941908,0.131849892144523,49.7872497326155));
#33995=CARTESIAN_POINT('Ctrl Pts',(5.21869385085329,0.00444285787804401,
49.7828633223158));
#33996=CARTESIAN_POINT('Ctrl Pts',(5.22005878849942,-0.123179295803443,
49.7784880643338));
#33997=CARTESIAN_POINT('Ctrl Pts',(5.22077192299229,-0.189857623640299,
49.7762021376535));
#33998=CARTESIAN_POINT('Ctrl Pts',(5.22020421945982,-0.256594784247294,
49.7739194680061));
#33999=CARTESIAN_POINT('Ctrl Pts',(5.21834663224238,-0.323355354262235,
49.771644593243));
#34000=CARTESIAN_POINT('Ctrl Pts',(5.21760990549823,-0.349832871400289,
49.7707423685388));
#34001=CARTESIAN_POINT('Ctrl Pts',(5.21666999205992,-0.376318760520563,
49.7698412213317));
#34002=CARTESIAN_POINT('Ctrl Pts',(5.21552778162834,-0.40278134925187,49.7689424724782));
#34003=CARTESIAN_POINT('Ctrl Pts',(5.21403770096407,-0.437303352120437,
49.7677700017568));
#34004=CARTESIAN_POINT('Ctrl Pts',(5.21220321919947,-0.471794424074401,
49.7666013129027));
#34005=CARTESIAN_POINT('Ctrl Pts',(5.21002489504197,-0.506249741277439,
49.7654371522064));
#34006=CARTESIAN_POINT('Ctrl Pts',(5.20048560553725,-0.657136029089896,
49.76033907446));
#34007=CARTESIAN_POINT('Ctrl Pts',(5.18435463935589,-0.807337611433697,
49.7553259977829));
#34008=CARTESIAN_POINT('Ctrl Pts',(5.16180066510662,-0.956461402467586,
49.7503329133453));
#34009=CARTESIAN_POINT('Ctrl Pts',(5.13892017184147,-1.1077440925476,49.7452675428885));
#34010=CARTESIAN_POINT('Ctrl Pts',(5.1094289591262,-1.25791749088514,49.7402225599689));
#34011=CARTESIAN_POINT('Ctrl Pts',(5.0734771776897,-1.40656178859565,49.7351555827664));
#34012=CARTESIAN_POINT('Ctrl Pts',(5.03735518795703,-1.55590982035319,49.7300646167233));
#34013=CARTESIAN_POINT('Ctrl Pts',(4.99471115982055,-1.70371415190665,49.7249513647013));
#34014=CARTESIAN_POINT('Ctrl Pts',(4.94567556523468,-1.8495408292695,49.7198003753935));
#34015=CARTESIAN_POINT('Ctrl Pts',(4.91220116110093,-1.94909017037065,49.7162840257044));
#34016=CARTESIAN_POINT('Ctrl Pts',(4.87574775360055,-2.04771773028405,49.7127506702632));
#34017=CARTESIAN_POINT('Ctrl Pts',(4.8363511645014,-2.14528350432509,49.7092029050148));
#34018=CARTESIAN_POINT('Ctrl Pts',(4.81834271520086,-2.18988148439041,49.7075811973476));
#34019=CARTESIAN_POINT('Ctrl Pts',(4.79971923269632,-2.23425758647001,49.7059565627866));
#34020=CARTESIAN_POINT('Ctrl Pts',(4.78048379291373,-2.27839832664545,49.704329671404));
#34021=CARTESIAN_POINT('Ctrl Pts',(4.77194664210255,-2.29798904877367,49.7036076178798));
#34022=CARTESIAN_POINT('Ctrl Pts',(4.7632889450894,-2.31753340840308,49.7028851232796));
#34023=CARTESIAN_POINT('Ctrl Pts',(4.75451095611775,-2.33703022197421,49.7021622627468));
#34024=CARTESIAN_POINT('Ctrl Pts',(4.74667071160333,-2.35444420895271,49.7015166247373));
#34025=CARTESIAN_POINT('Ctrl Pts',(4.73873635227771,-2.37181609008569,49.7008708493076));
#34026=CARTESIAN_POINT('Ctrl Pts',(4.73071159737849,-2.3891379247781,49.7002252650528));
#34027=CARTESIAN_POINT('Ctrl Pts',(4.66523858368199,-2.53046469853094,49.6949580204724));
#34028=CARTESIAN_POINT('Ctrl Pts',(4.59368613047665,-2.6686038217097,49.6896960901462));
#34029=CARTESIAN_POINT('Ctrl Pts',(4.51629355623815,-2.80317176969319,49.6844869056202));
#34030=CARTESIAN_POINT('Ctrl Pts',(4.48067498182562,-2.86510430670922,49.6820894698391));
#34031=CARTESIAN_POINT('Ctrl Pts',(4.44381883724951,-2.92628069281049,49.6797035477704));
#34032=CARTESIAN_POINT('Ctrl Pts',(4.40574537996631,-2.98666472899764,49.6773353894376));
#34033=CARTESIAN_POINT('Ctrl Pts',(4.32349081779372,-3.11711945555011,49.6722191788092));
#34034=CARTESIAN_POINT('Ctrl Pts',(4.23555519682983,-3.24387869280854,49.6671843479792));
#34035=CARTESIAN_POINT('Ctrl Pts',(4.14224309128914,-3.36664706312078,49.6621642705163));
#34036=CARTESIAN_POINT('Ctrl Pts',(4.04832514101874,-3.49021252797609,49.6571115993459));
#34037=CARTESIAN_POINT('Ctrl Pts',(3.94896027663346,-3.60973488258529,49.6520736777843));
#34038=CARTESIAN_POINT('Ctrl Pts',(3.84444539643511,-3.72488498895488,49.6470075110166));
#34039=CARTESIAN_POINT('Ctrl Pts',(3.79544021921852,-3.7788768354598,49.6446320750999));
#34040=CARTESIAN_POINT('Ctrl Pts',(3.74530265014764,-3.83190706666856,49.6422508029622));
#34041=CARTESIAN_POINT('Ctrl Pts',(3.69406254468819,-3.88393986178611,49.6398612952612));
#34042=CARTESIAN_POINT('Ctrl Pts',(3.65781405006707,-3.92074912431648,49.6381708995004));
#34043=CARTESIAN_POINT('Ctrl Pts',(3.62101378289051,-3.95705919634303,49.6364764096212));
#34044=CARTESIAN_POINT('Ctrl Pts',(3.58367218371391,-3.99285705051874,49.6347773814871));
#34045=CARTESIAN_POINT('Ctrl Pts',(3.5629338467586,-4.01273804058193,49.6338337952799));
#34046=CARTESIAN_POINT('Ctrl Pts',(3.5420240329473,-4.03246511448107,49.6328886149264));
#34047=CARTESIAN_POINT('Ctrl Pts',(3.52096943456868,-4.05201320692815,49.6319429224079));
#34048=CARTESIAN_POINT('Ctrl Pts',(3.40614714622976,-4.15861969103541,49.6267855417209));
#34049=CARTESIAN_POINT('Ctrl Pts',(3.2869131976001,-4.26001078709387,49.621605694337));
#34050=CARTESIAN_POINT('Ctrl Pts',(3.16366579501986,-4.35593771903587,49.6164161867119));
#34051=CARTESIAN_POINT('Ctrl Pts',(3.03981531919331,-4.45233403990652,49.6112012858278));
#34052=CARTESIAN_POINT('Ctrl Pts',(2.91191230951189,-4.54321295118199,49.6059767851582));
#34053=CARTESIAN_POINT('Ctrl Pts',(2.78032667834594,-4.62831864044268,49.6007824755997));
#34054=CARTESIAN_POINT('Ctrl Pts',(2.68229691010553,-4.6917213913376,49.5969127752557));
#34055=CARTESIAN_POINT('Ctrl Pts',(2.5822225803561,-4.75191998217825,49.5930604106771));
#34056=CARTESIAN_POINT('Ctrl Pts',(2.48024286974118,-4.80880497922347,49.5892505120726));
#34057=CARTESIAN_POINT('Ctrl Pts',(2.34350335530138,-4.88507923836746,49.5841420088017));
#34058=CARTESIAN_POINT('Ctrl Pts',(2.20333578698035,-4.95539857695016,49.5791090270458));
#34059=CARTESIAN_POINT('Ctrl Pts',(2.06013087428636,-5.01960377050101,49.5740842955298));
#34060=CARTESIAN_POINT('Ctrl Pts',(2.01243378737825,-5.04098851659063,49.5724107142867));
#34061=CARTESIAN_POINT('Ctrl Pts',(1.96439981353058,-5.06169468099203,49.5707382348701));
#34062=CARTESIAN_POINT('Ctrl Pts',(1.91604359986973,-5.08171549901325,49.5690649525599));
#34063=CARTESIAN_POINT('Ctrl Pts',(1.87554041937874,-5.09848494278274,49.5676634107457));
#34064=CARTESIAN_POINT('Ctrl Pts',(1.83481116554692,-5.11477355733233,49.5662613106286));
#34065=CARTESIAN_POINT('Ctrl Pts',(1.79386451568791,-5.13057715241704,49.5648577003405));
#34066=CARTESIAN_POINT('Ctrl Pts',(1.77567815094702,-5.1375962845174,49.5642342899091));
#34067=CARTESIAN_POINT('Ctrl Pts',(1.75745120137326,-5.14451880655941,49.563610662824));
#34068=CARTESIAN_POINT('Ctrl Pts',(1.7391946641175,-5.15134072548734,49.5629870931035));
#34069=CARTESIAN_POINT('Ctrl Pts',(1.59001261215237,-5.20708557182655,49.5578916355613));
#34070=CARTESIAN_POINT('Ctrl Pts',(1.43866498273231,-5.25618865327407,49.5527910414675));
#34071=CARTESIAN_POINT('Ctrl Pts',(1.28563400442455,-5.29859710524125,49.5476623291469));
#34072=CARTESIAN_POINT('Ctrl Pts',(1.13288844745672,-5.34092646030062,49.5425431824971));
#34073=CARTESIAN_POINT('Ctrl Pts',(0.978465894027958,-5.37658617453509,
49.5373960864726));
#34074=CARTESIAN_POINT('Ctrl Pts',(0.822827740101826,-5.40550619246802,
49.5322268987557));
#34075=CARTESIAN_POINT('Ctrl Pts',(0.666753346477603,-5.434507270601,49.5270432222721));
#34076=CARTESIAN_POINT('Ctrl Pts',(0.509456618531798,-5.45673116976558,
49.5218374346355));
#34077=CARTESIAN_POINT('Ctrl Pts',(0.351383211732529,-5.47208668410592,
49.5166431048256));
#34078=CARTESIAN_POINT('Ctrl Pts',(0.19330980493326,-5.48744219844627,49.5114487750157));
#34079=CARTESIAN_POINT('Ctrl Pts',(0.0344597161104908,-5.49592995853461,
49.5062660817186));
#34080=CARTESIAN_POINT('Ctrl Pts',(-0.124741716672891,-5.49743085582899,
49.5011540746717));
#34081=CARTESIAN_POINT('Ctrl Pts',(-0.180692942040016,-5.49795834506889,
49.4993574635901));
#34082=CARTESIAN_POINT('Ctrl Pts',(-0.236687812261172,-5.49762253264645,
49.4975698016442));
#34083=CARTESIAN_POINT('Ctrl Pts',(-0.292708187959222,-5.49642372103878,
49.4957878125479));
#34084=CARTESIAN_POINT('Ctrl Pts',(-0.310662081935003,-5.49603951553797,
49.4952167052873));
#34085=CARTESIAN_POINT('Ctrl Pts',(-0.328616265529814,-5.49556668586931,
49.4946462573012));
#34086=CARTESIAN_POINT('Ctrl Pts',(-0.346561355889629,-5.49500566096314,
49.4940766453379));
#34087=CARTESIAN_POINT('Ctrl Pts',(-0.503655794107246,-5.49009435147994,
49.4890901632658));
#34088=CARTESIAN_POINT('Ctrl Pts',(-0.660246401114815,-5.47842251008643,
49.4841595921883));
#34089=CARTESIAN_POINT('Ctrl Pts',(-0.815916987885523,-5.46014480646224,
49.4792299596291));
#34090=CARTESIAN_POINT('Ctrl Pts',(-0.973868778975,-5.44159926048382,49.4742280879957));
#34091=CARTESIAN_POINT('Ctrl Pts',(-1.13087330605085,-5.41625257091423,
49.4692270433391));
#34092=CARTESIAN_POINT('Ctrl Pts',(-1.28649294986338,-5.38424187213397,
49.4641961154961));
#34093=CARTESIAN_POINT('Ctrl Pts',(-1.44300002932614,-5.35204862933427,
49.459136498314));
#34094=CARTESIAN_POINT('Ctrl Pts',(-1.59810631725191,-5.3131151399391,49.4540466189856));
#34095=CARTESIAN_POINT('Ctrl Pts',(-1.75136501543228,-5.26755851017518,
49.4489233408825));
#34096=CARTESIAN_POINT('Ctrl Pts',(-1.90361219626974,-5.22230255712089,
49.4438338767471));
#34097=CARTESIAN_POINT('Ctrl Pts',(-2.05403612331965,-5.17051080101936,
49.4387115327372));
#34098=CARTESIAN_POINT('Ctrl Pts',(-2.20219753609186,-5.11227467177507,
49.4335804768557));
#34099=CARTESIAN_POINT('Ctrl Pts',(-2.25665635950895,-5.09086915856033,
49.4316944846735));
#34100=CARTESIAN_POINT('Ctrl Pts',(-2.3108094940984,-5.06859274266779,49.4298075756852));
#34101=CARTESIAN_POINT('Ctrl Pts',(-2.36463504949088,-5.04544904547062,
49.4279218429996));
#34102=CARTESIAN_POINT('Ctrl Pts',(-2.38837021496942,-5.03524349387428,
49.427090301606));
#34103=CARTESIAN_POINT('Ctrl Pts',(-2.41204483876381,-5.02486780300145,
49.4262588832171));
#34104=CARTESIAN_POINT('Ctrl Pts',(-2.43563327483403,-5.0143331018827,49.4254286347634));
#34105=CARTESIAN_POINT('Ctrl Pts',(-2.55373048104147,-4.96159036104766,
49.421271936009));
#34106=CARTESIAN_POINT('Ctrl Pts',(-2.66978375591747,-4.90481436355621,
49.4171397528067));
#34107=CARTESIAN_POINT('Ctrl Pts',(-2.78359497648946,-4.84411571837135,
49.413063622511));
#34108=CARTESIAN_POINT('Ctrl Pts',(-2.924248586175,-4.76910129092416,49.4080261364287));
#34109=CARTESIAN_POINT('Ctrl Pts',(-3.0614810489766,-4.68809507551227,49.403073459607));
#34110=CARTESIAN_POINT('Ctrl Pts',(-3.19498666686176,-4.60140279590078,
49.3981389260757));
#34111=CARTESIAN_POINT('Ctrl Pts',(-3.3299447733608,-4.51376733838381,49.3931507067604));
#34112=CARTESIAN_POINT('Ctrl Pts',(-3.46109428099897,-4.42032105177208,
49.3881808356728));
#34113=CARTESIAN_POINT('Ctrl Pts',(-3.58809628381318,-4.32136180668214,
49.3831857066336));
#34114=CARTESIAN_POINT('Ctrl Pts',(-3.70950179427866,-4.22676331690086,
49.3784106938195));
#34115=CARTESIAN_POINT('Ctrl Pts',(-3.82711700729642,-4.12712681810338,
49.3736127057868));
#34116=CARTESIAN_POINT('Ctrl Pts',(-3.94062874722527,-4.02270054491346,
49.3687768116061));
#34117=CARTESIAN_POINT('Ctrl Pts',(-3.98572004581248,-3.98121834873086,
49.3668558054743));
#34118=CARTESIAN_POINT('Ctrl Pts',(-4.03016364557377,-3.93898021007131,
49.3649290738369));
#34119=CARTESIAN_POINT('Ctrl Pts',(-4.07393922780361,-3.89600120334253,
49.3629966996388));
#34120=CARTESIAN_POINT('Ctrl Pts',(-4.10700497887908,-3.8635371431159,49.3615370867458));
#34121=CARTESIAN_POINT('Ctrl Pts',(-4.13968958544803,-3.83065037589362,
49.3600742663872));
#34122=CARTESIAN_POINT('Ctrl Pts',(-4.17198414223093,-3.79734728864012,
49.3586084949218));
#34123=CARTESIAN_POINT('Ctrl Pts',(-4.18608658919232,-3.78280443472203,
49.3579684191193));
#34124=CARTESIAN_POINT('Ctrl Pts',(-4.20011079548223,-3.76818613348426,
49.3573279572478));
#34125=CARTESIAN_POINT('Ctrl Pts',(-4.21405108877795,-3.75349847141212,
49.3566873776368));
#34126=CARTESIAN_POINT('Ctrl Pts',(-4.32957559830332,-3.6317804471952,49.3513788347101));
#34127=CARTESIAN_POINT('Ctrl Pts',(-4.43944604389779,-3.50519034747474,
49.3460548328354));
#34128=CARTESIAN_POINT('Ctrl Pts',(-4.54337101560959,-3.37414716019543,
49.3407518834976));
#34129=CARTESIAN_POINT('Ctrl Pts',(-4.64729598732139,-3.24310397291613,
49.3354489341598));
#34130=CARTESIAN_POINT('Ctrl Pts',(-4.74527612649365,-3.10760807449447,
49.3301673120086));
#34131=CARTESIAN_POINT('Ctrl Pts',(-4.8370174576042,-2.96803270750451,49.3249708337327));
#34132=CARTESIAN_POINT('Ctrl Pts',(-4.92609830595216,-2.83250500205884,
49.3199250524297));
#34133=CARTESIAN_POINT('Ctrl Pts',(-5.00929931953407,-2.69312714851096,
49.3149596075419));
#34134=CARTESIAN_POINT('Ctrl Pts',(-5.08645441034632,-2.55029552791752,
49.3100065247623));
#34135=CARTESIAN_POINT('Ctrl Pts',(-5.16378621091767,-2.40713677737061,
49.3050420978439));
#34136=CARTESIAN_POINT('Ctrl Pts',(-5.23504395172591,-2.26050815104089,
49.3000898940267));
#34137=CARTESIAN_POINT('Ctrl Pts',(-5.3000273093003,-2.1108115805684,49.2951060476122));
#34138=CARTESIAN_POINT('Ctrl Pts',(-5.31786155570052,-2.06972836137618,
49.2937382644091));
#34139=CARTESIAN_POINT('Ctrl Pts',(-5.33522304787959,-2.02841409497743,
49.2923682492653));
#34140=CARTESIAN_POINT('Ctrl Pts',(-5.35210726416258,-1.98687715762331,
49.2909954452123));
#34141=CARTESIAN_POINT('Ctrl Pts',(-5.36297878413954,-1.96013208182836,
49.2901115151301));
#34142=CARTESIAN_POINT('Ctrl Pts',(-5.37365434333545,-1.93328954670697,
49.2892262632332));
#34143=CARTESIAN_POINT('Ctrl Pts',(-5.38412129062111,-1.90638177843231,
49.2883405601123));
#34144=CARTESIAN_POINT('Ctrl Pts',(-5.44359691541729,-1.75348559138468,
49.283307789328));
#34145=CARTESIAN_POINT('Ctrl Pts',(-5.49640364515274,-1.59833076538052,
49.2782530325609));
#34146=CARTESIAN_POINT('Ctrl Pts',(-5.54246661452835,-1.44139155837415,
49.27317314757));
#34147=CARTESIAN_POINT('Ctrl Pts',(-5.58879486804785,-1.28354851291058,
49.2680640066939));
#34148=CARTESIAN_POINT('Ctrl Pts',(-5.62830171747107,-1.12390060961607,
49.2629295393757));
#34149=CARTESIAN_POINT('Ctrl Pts',(-5.66089528402405,-0.962905702878125,
49.2577946040462));
#34150=CARTESIAN_POINT('Ctrl Pts',(-5.69333557172059,-0.802667912277112,
49.252683816949));
#34151=CARTESIAN_POINT('Ctrl Pts',(-5.71892794727571,-0.641095804455549,
49.2475727597972));
#34152=CARTESIAN_POINT('Ctrl Pts',(-5.73756064484128,-0.478615090618444,
49.2425114365551));
#34153=CARTESIAN_POINT('Ctrl Pts',(-5.74450339795431,-0.418072945401361,
49.2406255304713));
#34154=CARTESIAN_POINT('Ctrl Pts',(-5.75047962292998,-0.357404389991355,
49.2387467691439));
#34155=CARTESIAN_POINT('Ctrl Pts',(-5.75548252324649,-0.296630523360118,
49.2368785590806));
#34156=CARTESIAN_POINT('Ctrl Pts',(-5.76537892967853,-0.17641168097307,
49.2331829895276));
#34157=CARTESIAN_POINT('Ctrl Pts',(-5.77146731689194,-0.0557799619614495,
49.2295283245924));
#34158=CARTESIAN_POINT('Ctrl Pts',(-5.77374672853297,0.065096445717814,
49.2258863162828));
#34159=CARTESIAN_POINT('Ctrl Pts',(-5.77459391555212,0.110022479112958,
49.2245326940989));
#34160=CARTESIAN_POINT('Ctrl Pts',(-5.77491484307218,0.154982237612365,
49.2231808830343));
#34161=CARTESIAN_POINT('Ctrl Pts',(-5.77470914469647,0.199966813322252,
49.2218296639618));
#34162=CARTESIAN_POINT('Ctrl Pts',(-5.77458352980315,0.227437777343764,
49.221004508007));
#34163=CARTESIAN_POINT('Ctrl Pts',(-5.77426136385812,0.254922353169247,
49.2201794445654));
#34164=CARTESIAN_POINT('Ctrl Pts',(-5.77374329813058,0.282389833044242,
49.2193550800525));
#34165=CARTESIAN_POINT('Ctrl Pts',(-5.77065780153438,0.445980688713763,
49.2144453287152));
#34166=CARTESIAN_POINT('Ctrl Pts',(-5.76062670170217,0.609147527714891,
49.2095527300581));
#34167=CARTESIAN_POINT('Ctrl Pts',(-5.74378571552021,0.771448622323782,
49.2046391550914));
#34168=CARTESIAN_POINT('Ctrl Pts',(-5.72666463659201,0.936449045749695,
49.1996438594528));
#34169=CARTESIAN_POINT('Ctrl Pts',(-5.70250521466273,1.10055459203251,49.1946267993558));
#34170=CARTESIAN_POINT('Ctrl Pts',(-5.67142703313475,1.26330529042377,49.1895761902436));
#34171=CARTESIAN_POINT('Ctrl Pts',(-5.64034926925677,1.42605380165904,49.1845256490049));
#34172=CARTESIAN_POINT('Ctrl Pts',(-5.60235308985842,1.58744747929261,49.1794416145631));
#34173=CARTESIAN_POINT('Ctrl Pts',(-5.55753454842355,1.74703145364951,49.1743404530506));
#34174=CARTESIAN_POINT('Ctrl Pts',(-5.5200120235029,1.88063673090842,49.1700697103212));
#34175=CARTESIAN_POINT('Ctrl Pts',(-5.47770730015332,2.01297368705868,49.1657874941309));
#34176=CARTESIAN_POINT('Ctrl Pts',(-5.43066194318534,2.14377785630578,49.1615179508413));
#34177=CARTESIAN_POINT('Ctrl Pts',(-5.40713926470134,2.20917994092934,49.1593831791965));
#34178=CARTESIAN_POINT('Ctrl Pts',(-5.38243120004108,2.27419885983428,49.1572517781467));
#34179=CARTESIAN_POINT('Ctrl Pts',(-5.35654143278953,2.33880167648566,49.155127939542));
#34180=CARTESIAN_POINT('Ctrl Pts',(-5.34671655063384,2.36331773545052,49.1543219661314));
#34181=CARTESIAN_POINT('Ctrl Pts',(-5.33672147795149,2.38777387113981,49.1535170895802));
#34182=CARTESIAN_POINT('Ctrl Pts',(-5.3265563732068,2.41216828423402,49.1527135670967));
#34183=CARTESIAN_POINT('Ctrl Pts',(-5.31673784757985,2.43573097012222,49.1519374407022));
#34184=CARTESIAN_POINT('Ctrl Pts',(-5.306759648629,2.4592382882221,49.1511625043726));
#34185=CARTESIAN_POINT('Ctrl Pts',(-5.29663156396569,2.48266680522254,49.150389723225));
#34186=CARTESIAN_POINT('Ctrl Pts',(-5.28961442410136,2.49889901358878,49.1498543097113));
#34187=CARTESIAN_POINT('Ctrl Pts',(-5.28252441466418,2.51509565043687,49.1493198567731));
#34188=CARTESIAN_POINT('Ctrl Pts',(-5.27536177146622,2.53125625338851,49.1487864472261));
#34189=CARTESIAN_POINT('Ctrl Pts',(-5.20905723135039,2.68085484668549,49.1438486786215));
#34190=CARTESIAN_POINT('Ctrl Pts',(-5.1365305147677,2.82736721515206,49.1389984596951));
#34191=CARTESIAN_POINT('Ctrl Pts',(-5.05808337360841,2.97048046784585,49.1341699969887));
#34192=CARTESIAN_POINT('Ctrl Pts',(-4.97795812668693,3.11665513451141,49.129238245992));
#34193=CARTESIAN_POINT('Ctrl Pts',(-4.89165612942615,3.25928352807764,49.1243289773594));
#34194=CARTESIAN_POINT('Ctrl Pts',(-4.79947735049932,3.39801430845291,49.1193976432336));
#34195=CARTESIAN_POINT('Ctrl Pts',(-4.70691216791804,3.53732663353017,49.1144456374787));
#34196=CARTESIAN_POINT('Ctrl Pts',(-4.60842069933321,3.67270845509946,49.1094712986947));
#34197=CARTESIAN_POINT('Ctrl Pts',(-4.50428872136281,3.80378869777911,49.104457163013));
#34198=CARTESIAN_POINT('Ctrl Pts',(-4.4008671297137,3.93397471360161,49.0994772336671));
#34199=CARTESIAN_POINT('Ctrl Pts',(-4.291881788178,4.05991762763984,49.0944580775447));
#34200=CARTESIAN_POINT('Ctrl Pts',(-4.1775954660098,4.18124012170818,49.0894101112488));
#34201=CARTESIAN_POINT('Ctrl Pts',(-4.13145291568673,4.23022349243586,49.0873720192495));
#34202=CARTESIAN_POINT('Ctrl Pts',(-4.08444604836479,4.27845353024594,49.0853295426084));
#34203=CARTESIAN_POINT('Ctrl Pts',(-4.03659128039468,4.32590472425831,49.0832846233473));
#34204=CARTESIAN_POINT('',(-4.72583710973184,1.63293098821764,50.));
#34205=CARTESIAN_POINT('Origin',(0.,0.,50.));
#34206=CARTESIAN_POINT('Ctrl Pts',(0.902188245823411,5.84749488262084,49.083316804731));
#34207=CARTESIAN_POINT('Ctrl Pts',(0.570773072266766,5.86193985911904,49.1195756242143));
#34208=CARTESIAN_POINT('Ctrl Pts',(0.239586412830494,5.84829261175139,49.1560808085295));
#34209=CARTESIAN_POINT('Ctrl Pts',(-0.403141186164292,5.76508832621516,
49.229396259483));
#34210=CARTESIAN_POINT('Ctrl Pts',(-0.712291744810658,5.6984338729017,49.2658262564742));
#34211=CARTESIAN_POINT('Ctrl Pts',(-1.41949250323092,5.48319083688572,49.3516406277647));
#34212=CARTESIAN_POINT('Ctrl Pts',(-2.04693271827507,5.24616261480877,49.4260186478511));
#34213=CARTESIAN_POINT('Ctrl Pts',(-2.95875165016973,4.57432864164807,49.5617463576736));
#34214=CARTESIAN_POINT('Ctrl Pts',(-3.20150736272193,4.35877003192118,49.6014258895003));
#34215=CARTESIAN_POINT('Ctrl Pts',(-3.75505974601525,3.76967225965931,49.7008828051444));
#34216=CARTESIAN_POINT('Ctrl Pts',(-4.04010787119168,3.37408581464056,49.7592710513533));
#34217=CARTESIAN_POINT('Ctrl Pts',(-4.47964495834608,2.52220292271381,49.8796783199167));
#34218=CARTESIAN_POINT('Ctrl Pts',(-4.6331687113469,2.08624253568,49.9395418565637));
#34219=CARTESIAN_POINT('Ctrl Pts',(-4.72583710973167,1.63293098821788,50.0000000000001));
#34220=CARTESIAN_POINT('Ctrl Pts',(3.43704063106228,-4.81656042341828,-0.576723952463529));
#34221=CARTESIAN_POINT('Ctrl Pts',(4.23851061681899,-4.24464230409036,-0.530378404645798));
#34222=CARTESIAN_POINT('Ctrl Pts',(5.54954235425666,-2.69365781311748,-0.437692858323896));
#34223=CARTESIAN_POINT('Ctrl Pts',(6.16159033410026,0.291989391379818,-0.298667313497819));
#34224=CARTESIAN_POINT('Ctrl Pts',(5.27018942791115,3.20546788220774,-0.159647317985302));
#34225=CARTESIAN_POINT('Ctrl Pts',(3.09280338018427,5.33718340530576,-0.0206273224727845));
#34226=CARTESIAN_POINT('Ctrl Pts',(0.160760791193982,6.16638660286929,0.118392673039733));
#34227=CARTESIAN_POINT('Ctrl Pts',(-2.8105137177503,5.49104909633203,0.257412668552251));
#34228=CARTESIAN_POINT('Ctrl Pts',(-5.09599974900626,3.47580295946428,0.396432664064767));
#34229=CARTESIAN_POINT('Ctrl Pts',(-6.13802598467403,0.61246246229798,0.535452659577285));
#34230=CARTESIAN_POINT('Ctrl Pts',(-5.68232839089761,-2.40033714446484,
0.674472655089802));
#34231=CARTESIAN_POINT('Ctrl Pts',(-3.8401015449425,-4.82742989807141,0.813492650602319));
#34232=CARTESIAN_POINT('Ctrl Pts',(-1.06086171213873,-6.0765981420124,0.952512646114838));
#34233=CARTESIAN_POINT('Ctrl Pts',(1.97723602956149,-5.84303022933689,1.09153264162736));
#34234=CARTESIAN_POINT('Ctrl Pts',(4.53287379508907,-4.1837212419108,1.23055263713987));
#34235=CARTESIAN_POINT('Ctrl Pts',(5.98245724399727,-1.50355324653343,1.36957263265239));
#34236=CARTESIAN_POINT('Ctrl Pts',(5.97227747058842,1.54349246619894,1.50859262816491));
#34237=CARTESIAN_POINT('Ctrl Pts',(4.50481839510344,4.21391487875842,1.64761262367743));
#34238=CARTESIAN_POINT('Ctrl Pts',(1.93815075286798,5.85611123715929,1.78663261918994));
#34239=CARTESIAN_POINT('Ctrl Pts',(-1.10143982170116,6.06937374228201,1.92565261470246));
#34240=CARTESIAN_POINT('Ctrl Pts',(-3.87227103928215,4.80166473547632,2.06467261021498));
#34241=CARTESIAN_POINT('Ctrl Pts',(-5.69823985920696,2.3623144936764,2.20369260572749));
#34242=CARTESIAN_POINT('Ctrl Pts',(-6.13379656062603,-0.653457732117191,
2.34271260124001));
#34243=CARTESIAN_POINT('Ctrl Pts',(-5.0726621295139,-3.50978149923841,2.48173259675253));
#34244=CARTESIAN_POINT('Ctrl Pts',(-2.77376111232836,-5.5096929631069,2.62075259226505));
#34245=CARTESIAN_POINT('Ctrl Pts',(0.201957862492829,-6.16519912697854,
2.75977258777756));
#34246=CARTESIAN_POINT('Ctrl Pts',(3.12839764474893,-5.31635170311109,2.89879258329009));
#34247=CARTESIAN_POINT('Ctrl Pts',(5.29148556685501,-3.17027565837135,3.03781257880259));
#34248=CARTESIAN_POINT('Ctrl Pts',(6.16341238700176,-0.25062921257097,3.17683257431512));
#34249=CARTESIAN_POINT('Ctrl Pts',(5.53142159669249,2.73017259053316,3.31585256982763));
#34250=CARTESIAN_POINT('Ctrl Pts',(3.54972356179769,5.04479235342969,3.45487256534015));
#34251=CARTESIAN_POINT('Ctrl Pts',(0.701867067655108,6.12844595911452,3.59389256085267));
#34252=CARTESIAN_POINT('Ctrl Pts',(-2.31725011406836,5.7167140179715,3.73291255636519));
#34253=CARTESIAN_POINT('Ctrl Pts',(-4.77094135387005,3.91006212896485,3.8719325518777));
#34254=CARTESIAN_POINT('Ctrl Pts',(-6.06048807923677,1.14932654013476,4.01095254739023));
#34255=CARTESIAN_POINT('Ctrl Pts',(-5.87123147651013,-1.89185311366029,
4.14997254290273));
#34256=CARTESIAN_POINT('Ctrl Pts',(-4.24935153817855,-4.47140679869429,
4.28899253841526));
#34257=CARTESIAN_POINT('Ctrl Pts',(-1.59059880763312,-5.95990458712096,
4.42801253392777));
#34258=CARTESIAN_POINT('Ctrl Pts',(1.45627164208546,-5.99414215371037,4.56703252944029));
#34259=CARTESIAN_POINT('Ctrl Pts',(4.14780118150638,-4.56576528230742,4.7060525249528));
#34260=CARTESIAN_POINT('Ctrl Pts',(5.82723695697856,-2.0233083555536,4.84507252046533));
#34261=CARTESIAN_POINT('Ctrl Pts',(6.08478438073663,1.01285057850268,4.98409251597784));
#34262=CARTESIAN_POINT('Ctrl Pts',(4.8576000014916,3.80186657839784,5.12311251149037));
#34263=CARTESIAN_POINT('Ctrl Pts',(2.44512576525259,5.66319938255113,5.26213250700287));
#34264=CARTESIAN_POINT('Ctrl Pts',(-0.563977005188219,6.14267020049495,
5.4011525025154));
#34265=CARTESIAN_POINT('Ctrl Pts',(-3.43546526977796,5.123284652894,5.54017249802791));
#34266=CARTESIAN_POINT('Ctrl Pts',(-5.46867493236823,2.8537802540695,5.67919249354042));
#34267=CARTESIAN_POINT('Ctrl Pts',(-6.16748799446796,-0.112067357082,5.81821248905295));
#34268=CARTESIAN_POINT('Ctrl Pts',(-5.36138896814329,-3.05056971510259,
5.95723248456547));
#34269=CARTESIAN_POINT('Ctrl Pts',(-3.24707189970145,-5.24471079589703,
6.09625248007797));
#34270=CARTESIAN_POINT('Ctrl Pts',(-0.340445586681124,-6.15910416026057,
6.23527247559051));
#34271=CARTESIAN_POINT('Ctrl Pts',(2.64925193447237,-5.57063115294167,6.37429247110302));
#34272=CARTESIAN_POINT('Ctrl Pts',(4.99251264617518,-3.62288348311266,6.51331246661553));
#34273=CARTESIAN_POINT('Ctrl Pts',(6.11756383082583,-0.791125799226151,
6.65233246212806));
#34274=CARTESIAN_POINT('Ctrl Pts',(5.74988478738761,2.23367235426287,6.79135245764057));
#34275=CARTESIAN_POINT('Ctrl Pts',(3.97919188622503,4.7134381492739,6.93037245315309));
#34276=CARTESIAN_POINT('Ctrl Pts',(1.23754711987656,6.04309063149933,7.0693924486656));
#34277=CARTESIAN_POINT('Ctrl Pts',(-1.80606817683494,5.89818488986686,7.20841244417813));
#34278=CARTESIAN_POINT('Ctrl Pts',(-4.40898965553244,4.3140789830319,7.34743243969063));
#34279=CARTESIAN_POINT('Ctrl Pts',(-5.93608547614997,1.67730631497977,7.48645243520317));
#34280=CARTESIAN_POINT('Ctrl Pts',(-6.01473311186767,-1.36874133693413,
7.62547243071567));
#34281=CARTESIAN_POINT('Ctrl Pts',(-4.62574196550504,-4.08080611190917,
7.76449242622819));
#34282=CARTESIAN_POINT('Ctrl Pts',(-2.10803601530903,-5.79712440892808,
7.9035124217407));
#34283=CARTESIAN_POINT('Ctrl Pts',(0.924046109614526,-6.09890203575495,
8.04253241725323));
#34284=CARTESIAN_POINT('Ctrl Pts',(3.73065423898791,-4.91250304870655,8.18155241276573));
#34285=CARTESIAN_POINT('Ctrl Pts',(5.6269555032291,-2.527417460395,8.32057240827827));
#34286=CARTESIAN_POINT('Ctrl Pts',(6.15023855236694,0.474376436397263,8.45959240379077));
#34287=CARTESIAN_POINT('Ctrl Pts',(5.17281850286031,3.36041902013657,8.59861239930329));
#34288=CARTESIAN_POINT('Ctrl Pts',(2.93319298118051,5.42649483456707,8.73763239481581));
#34289=CARTESIAN_POINT('Ctrl Pts',(-0.0221530378913636,6.16846630025178,
8.87665239032833));
#34290=CARTESIAN_POINT('Ctrl Pts',(-2.97209355401811,5.40528696375999,9.01567238584084));
#34291=CARTESIAN_POINT('Ctrl Pts',(-5.1968215490371,3.32317815379998,9.15469238135336));
#34292=CARTESIAN_POINT('Ctrl Pts',(-6.15348715341253,0.430189617746093,
9.29371237686589));
#34293=CARTESIAN_POINT('Ctrl Pts',(-5.60865697677616,-2.56776832508109,
9.43273237237838));
#34294=CARTESIAN_POINT('Ctrl Pts',(-3.69527355905571,-4.93917205391485,
9.57175236789092));
#34295=CARTESIAN_POINT('Ctrl Pts',(-0.880216420357442,-6.10538174955201,
9.71077236340343));
#34296=CARTESIAN_POINT('Ctrl Pts',(2.14961994979028,-5.78183373385064,9.84979235891595));
#34297=CARTESIAN_POINT('Ctrl Pts',(4.65493336166727,-4.04747608428597,9.98881235442845));
#34298=CARTESIAN_POINT('Ctrl Pts',(6.02440905597324,-1.32550472678798,10.127832349941));
#34299=CARTESIAN_POINT('Ctrl Pts',(5.92388496721038,1.71989945918022,10.2668523454535));
#34300=CARTESIAN_POINT('Ctrl Pts',(4.37788970678303,4.34563562320553,10.405872340966));
#34301=CARTESIAN_POINT('Ctrl Pts',(1.76365740277551,5.91100497547285,10.5448923364785));
#34302=CARTESIAN_POINT('Ctrl Pts',(-1.28092018081044,6.03404596807335,10.6839123319911));
#34303=CARTESIAN_POINT('Ctrl Pts',(-4.01294389057655,4.68473570071077,10.8229323275036));
#34304=CARTESIAN_POINT('Ctrl Pts',(-5.7657799997321,2.19231572751711,10.9619523230161));
#34305=CARTESIAN_POINT('Ctrl Pts',(-6.1117237033288,-0.835045285357961,
11.1009723185286));
#34306=CARTESIAN_POINT('Ctrl Pts',(-4.9663622125742,-3.65864915343695,11.2399923140411));
#34307=CARTESIAN_POINT('Ctrl Pts',(-2.6091720914435,-5.58951592283822,11.3790123095536));
#34308=CARTESIAN_POINT('Ctrl Pts',(0.384675064887725,-6.15650000803081,
11.5180323050662));
#34309=CARTESIAN_POINT('Ctrl Pts',(3.28465869756325,-5.22125315369325,11.6570523005787));
#34310=CARTESIAN_POINT('Ctrl Pts',(5.38316163262817,-3.01198241884472,11.7960722960912));
#34311=CARTESIAN_POINT('Ctrl Pts',(6.1681338365184,-0.0677659887136258,
11.9350922916037));
#34312=CARTESIAN_POINT('Ctrl Pts',(5.44803636180983,2.89298583730161,12.0741122871163));
#34313=CARTESIAN_POINT('Ctrl Pts',(3.39857824847212,5.14782800251152,12.2131322826287));
#34314=CARTESIAN_POINT('Ctrl Pts',(0.519842235579626,6.14656256004421,12.3521522781413));
#34315=CARTESIAN_POINT('Ctrl Pts',(-2.48573907723061,5.64549098789099,12.4911722736538));
#34316=CARTESIAN_POINT('Ctrl Pts',(-4.88478191127144,3.76687840708258,12.6301922691663));
#34317=CARTESIAN_POINT('Ctrl Pts',(-6.0919023039256,0.969119999719169,12.7692122646788));
#34318=CARTESIAN_POINT('Ctrl Pts',(-5.81255406836334,-2.06511076138364,
12.9082322601914));
#34319=CARTESIAN_POINT('Ctrl Pts',(-4.11490021308256,-4.59543942303701,
13.0472522557038));
#34320=CARTESIAN_POINT('Ctrl Pts',(-1.41318067029944,-6.00444732240376,
13.1862722512164));
#34321=CARTESIAN_POINT('Ctrl Pts',(1.63336527113562,-5.94832624739747,13.3252922467289));
#34322=CARTESIAN_POINT('Ctrl Pts',(4.28135816414165,-4.44077014995906,13.4643122422414));
#34323=CARTESIAN_POINT('Ctrl Pts',(5.88466841457579,-1.84963372182813,13.6033322377539));
#34324=CARTESIAN_POINT('Ctrl Pts',(6.052076618438,1.19282683528906,13.7423522332665));
#34325=CARTESIAN_POINT('Ctrl Pts',(4.74273395203871,3.94422893790522,13.881372228779));
#34326=CARTESIAN_POINT('Ctrl Pts',(2.27612958314307,5.73321038992733,14.0203922242915));
#34327=CARTESIAN_POINT('Ctrl Pts',(-0.745867017981445,6.12324665891528,
14.159412219804));
#34328=CARTESIAN_POINT('Ctrl Pts',(-3.58586662248042,5.01916604828039,14.2984322153165));
#34329=CARTESIAN_POINT('Ctrl Pts',(-5.55088859710986,2.69037228593095,14.437452210829));
#34330=CARTESIAN_POINT('Ctrl Pts',(-6.16145323695721,-0.294891951771045,
14.5764722063416));
#34331=CARTESIAN_POINT('Ctrl Pts',(-5.26857831326169,-3.20820040076339,
14.7154922018541));
#34332=CARTESIAN_POINT('Ctrl Pts',(-3.09013182468434,-5.33868453464922,
14.8545121973666));
#34333=CARTESIAN_POINT('Ctrl Pts',(-0.157670615370865,-6.16649067391479,
14.9935321928791));
#34334=CARTESIAN_POINT('Ctrl Pts',(2.81326337496362,-5.48962807825065,15.1325521883917));
#34335=CARTESIAN_POINT('Ctrl Pts',(5.09774056721409,-3.47325616155927,15.2715721839041));
#34336=CARTESIAN_POINT('Ctrl Pts',(6.13833185159848,-0.609384389430206,
15.4105921794167));
#34337=CARTESIAN_POINT('Ctrl Pts',(5.68112535923535,2.40318162174289,15.5496121749292));
#34338=CARTESIAN_POINT('Ctrl Pts',(3.83768281150632,4.82935377588954,15.6886321704417));
#34339=CARTESIAN_POINT('Ctrl Pts',(1.05781764572689,6.07712835826415,15.8276521659542));
#34340=CARTESIAN_POINT('Ctrl Pts',(-1.98016274684031,5.84203926300189,15.9666721614667));
#34341=CARTESIAN_POINT('Ctrl Pts',(-4.53496897555987,4.18144994531072,16.1056921569792));
#34342=CARTESIAN_POINT('Ctrl Pts',(-5.98320967256359,1.50055631969322,16.2447121524918));
#34343=CARTESIAN_POINT('Ctrl Pts',(-5.97150353677324,-1.54648400080129,
16.3837321480043));
#34344=CARTESIAN_POINT('Ctrl Pts',(-4.50270695076721,-4.21617093699274,
16.5227521435168));
#34345=CARTESIAN_POINT('Ctrl Pts',(-1.93521700258198,-5.8570813898517,16.6617721390293));
#34346=CARTESIAN_POINT('Ctrl Pts',(1.10448001978357,-6.06882123153488,16.8007921345418));
#34347=CARTESIAN_POINT('Ctrl Pts',(3.8746758554932,-4.79972439513851,16.9398121300543));
#34348=CARTESIAN_POINT('Ctrl Pts',(5.69942250039969,-2.35945977214434,17.0788321255669));
#34349=CARTESIAN_POINT('Ctrl Pts',(6.13346845394157,0.656530257439375,17.2178521210794));
#34350=CARTESIAN_POINT('Ctrl Pts',(5.07090333526315,3.5123221120573,17.3568721165919));
#34351=CARTESIAN_POINT('Ctrl Pts',(2.77100078920524,5.51108173416558,17.4958921121044));
#34352=CARTESIAN_POINT('Ctrl Pts',(-0.20504617552828,6.16509718660872,17.6349121076169));
#34353=CARTESIAN_POINT('Ctrl Pts',(-3.13106037675837,5.31478392519616,17.7739321031294));
#34354=CARTESIAN_POINT('Ctrl Pts',(-5.29307299180025,3.16762459232536,17.912952098642));
#34355=CARTESIAN_POINT('Ctrl Pts',(-6.16353716160514,0.247541737778197,
18.0519720941545));
#34356=CARTESIAN_POINT('Ctrl Pts',(-5.53005327504208,-2.73294310764532,
18.190992089667));
#34357=CARTESIAN_POINT('Ctrl Pts',(-3.54719602436282,-5.0465698864847,18.3300120851795));
#34358=CARTESIAN_POINT('Ctrl Pts',(-0.698797052019465,-6.12879677706142,
18.469032080692));
#34359=CARTESIAN_POINT('Ctrl Pts',(2.3201135016813,-5.71555251867621,18.6080520762046));
#34360=CARTESIAN_POINT('Ctrl Pts',(4.77289942598214,-3.90767172673052,18.747072071717));
#34361=CARTESIAN_POINT('Ctrl Pts',(6.06106305196034,-1.14629051055608,18.8860920672296));
#34362=CARTESIAN_POINT('Ctrl Pts',(5.87028305230372,1.89479395720625,19.0251120627421));
#34363=CARTESIAN_POINT('Ctrl Pts',(4.24711113947134,4.47353486891608,19.1641320582546));
#34364=CARTESIAN_POINT('Ctrl Pts',(1.58761310806277,5.96070061935146,19.3031520537671));
#34365=CARTESIAN_POINT('Ctrl Pts',(-1.45927411003053,5.99341191027483,19.4421720492797));
#34366=CARTESIAN_POINT('Ctrl Pts',(-4.15008779373199,4.56368694793438,19.5811920447921));
#34367=CARTESIAN_POINT('Ctrl Pts',(-5.82824976341114,2.0203890590002,19.7202120403047));
#34368=CARTESIAN_POINT('Ctrl Pts',(-6.08427624921397,-1.01589850756883,
19.8592320358172));
#34369=CARTESIAN_POINT('Ctrl Pts',(-4.85569491981417,-3.8042994230371,19.9982520313297));
#34370=CARTESIAN_POINT('Ctrl Pts',(-2.44228858725531,-5.66442351091372,
20.1372720268422));
#34371=CARTESIAN_POINT('Ctrl Pts',(0.567053987364875,-6.14238691632522,
20.2762920223548));
#34372=CARTESIAN_POINT('Ctrl Pts',(3.43803125002338,-5.12156307959712,20.4153120178673));
#34373=CARTESIAN_POINT('Ctrl Pts',(5.47010379277291,-2.851040468096,20.5543320133798));
#34374=CARTESIAN_POINT('Ctrl Pts',(6.16743108266357,0.1151568279563,20.6933520088923));
#34375=CARTESIAN_POINT('Ctrl Pts',(5.35986017102552,3.05325501743365,20.8323720044048));
#34376=CARTESIAN_POINT('Ctrl Pts',(3.24444425492609,5.24633669631551,20.9713919999173));
#34377=CARTESIAN_POINT('Ctrl Pts',(0.337360258753054,6.1592739271966,21.1104119954299));
#34378=CARTESIAN_POINT('Ctrl Pts',(-2.65204210301827,5.56930336202366,21.2494319909424));
#34379=CARTESIAN_POINT('Ctrl Pts',(-4.99432683384769,3.62038212501645,21.3884519864549));
#34380=CARTESIAN_POINT('Ctrl Pts',(-6.1179593625907,0.78806122358511,21.5274719819674));
#34381=CARTESIAN_POINT('Ctrl Pts',(-5.74876515060713,-2.2365523686233,21.6664919774799));
#34382=CARTESIAN_POINT('Ctrl Pts',(-3.97683028044616,-4.71543085782797,
21.8055119729925));
#34383=CARTESIAN_POINT('Ctrl Pts',(-1.23451979414715,-6.04370979881467,
21.944531968505));
#34384=CARTESIAN_POINT('Ctrl Pts',(1.80902253293984,-5.89727943459912,22.0835519640175));
#34385=CARTESIAN_POINT('Ctrl Pts',(4.4111501575588,-4.31186984287546,22.22257195953));
#34386=CARTESIAN_POINT('Ctrl Pts',(5.93692494583333,-1.67433253625779,22.3615919550425));
#34387=CARTESIAN_POINT('Ctrl Pts',(6.01404671247788,1.37175413050724,22.5006119505551));
#34388=CARTESIAN_POINT('Ctrl Pts',(4.62369718350338,4.08312277671056,22.6396319460675));
#34389=CARTESIAN_POINT('Ctrl Pts',(2.10513179242921,5.79817966183642,22.7786519415801));
#34390=CARTESIAN_POINT('Ctrl Pts',(-0.927101121791352,6.09843838735811,
22.9176719370926));
#34391=CARTESIAN_POINT('Ctrl Pts',(-3.73311459519142,4.91063363259758,23.0566919326051));
#34392=CARTESIAN_POINT('Ctrl Pts',(-5.62822085858694,2.52459842774975,23.1957119281177));
#34393=CARTESIAN_POINT('Ctrl Pts',(-6.15000015093573,-0.477457221036609,
23.3347319236301));
#34394=CARTESIAN_POINT('Ctrl Pts',(-5.17113451632943,-3.36300982283073,
23.4737519191427));
#34395=CARTESIAN_POINT('Ctrl Pts',(-2.93047431455525,-5.4279634805479,23.6127719146552));
#34396=CARTESIAN_POINT('Ctrl Pts',(0.0252430101103464,-6.16845442917999,
23.7517919101677));
#34397=CARTESIAN_POINT('Ctrl Pts',(2.97480085605505,-5.40379747226373,23.8908119056802));
#34398=CARTESIAN_POINT('Ctrl Pts',(5.19848557943377,-3.32057448867644,24.0298319011927));
#34399=CARTESIAN_POINT('Ctrl Pts',(6.15370187660606,-0.427107092290141,
24.1688518967053));
#34400=CARTESIAN_POINT('Ctrl Pts',(5.60736999874005,2.57057755215821,24.3078718922178));
#34401=CARTESIAN_POINT('Ctrl Pts',(3.69279891182468,4.94102251070121,24.4468918877303));
#34402=CARTESIAN_POINT('Ctrl Pts',(0.8771579359188,6.10582191108489,24.5859118832428));
#34403=CARTESIAN_POINT('Ctrl Pts',(-2.152515978909,5.78075619750316,24.7249318787553));
#34404=CARTESIAN_POINT('Ctrl Pts',(-4.65696028322234,4.04514377679203,24.8639518742678));
#34405=CARTESIAN_POINT('Ctrl Pts',(-6.0250722863103,1.32248674820017,25.0029718697804));
#34406=CARTESIAN_POINT('Ctrl Pts',(-5.92302267328619,-1.72286670005763,
25.1419918652929));
#34407=CARTESIAN_POINT('Ctrl Pts',(-4.37571229460911,-4.34782809793997,
25.2810118608054));
#34408=CARTESIAN_POINT('Ctrl Pts',(-1.76069617681569,-5.91188770422582,
25.4200318563179));
#34409=CARTESIAN_POINT('Ctrl Pts',(1.28394265980739,-6.03340355858585,25.5590518518304));
#34410=CARTESIAN_POINT('Ctrl Pts',(4.01529011567363,-4.68272490558683,25.698071847343));
#34411=CARTESIAN_POINT('Ctrl Pts',(5.76687747488004,-2.18942719544423,25.8370918428554));
#34412=CARTESIAN_POINT('Ctrl Pts',(6.11130463658083,0.838106731470015,25.976111838368));
#34413=CARTESIAN_POINT('Ctrl Pts',(4.96452885927568,3.66113649839072,26.1151318338805));
#34414=CARTESIAN_POINT('Ctrl Pts',(2.60637180318128,5.59082223630937,26.254151829393));
#34415=CARTESIAN_POINT('Ctrl Pts',(-0.387758997337801,6.15630653999729,
26.3931718249055));
#34416=CARTESIAN_POINT('Ctrl Pts',(-3.28727377217307,5.21960711176738,26.532191820418));
#34417=CARTESIAN_POINT('Ctrl Pts',(-5.38466975210494,3.00928544927126,26.6712118159306));
#34418=CARTESIAN_POINT('Ctrl Pts',(-6.16816700870177,0.0646761717542413,
26.8102318114431));
#34419=CARTESIAN_POINT('Ctrl Pts',(-5.44658649244489,-2.89571456375564,
26.9492518069556));
#34420=CARTESIAN_POINT('Ctrl Pts',(-3.39599911626685,-5.14952980928789,
27.0882718024682));
#34421=CARTESIAN_POINT('Ctrl Pts',(-0.516763167617664,-6.14682219386762,
27.2272917979806));
#34422=CARTESIAN_POINT('Ctrl Pts',(2.48856676589174,-5.64424509621337,27.3663117934932));
#34423=CARTESIAN_POINT('Ctrl Pts',(4.88666824395851,-3.76443099656735,27.5053317890056));
#34424=CARTESIAN_POINT('Ctrl Pts',(6.09238700169426,-0.966068256396196,
27.6443517845182));
#34425=CARTESIAN_POINT('Ctrl Pts',(5.81151886142015,2.06802218986825,27.7833717800307));
#34426=CARTESIAN_POINT('Ctrl Pts',(4.11259769947784,4.59750012688192,27.9223917755432));
#34427=CARTESIAN_POINT('Ctrl Pts',(1.41017268015921,6.0051544748293,28.0614117710557));
#34428=CARTESIAN_POINT('Ctrl Pts',(-1.63634476626115,5.94750729805012,28.2004317665683));
#34429=CARTESIAN_POINT('Ctrl Pts',(-4.28358214569388,4.43862492845726,28.3394517620808));
#34430=CARTESIAN_POINT('Ctrl Pts',(-5.88559421482269,1.84668567787679,28.4784717575933));
#34431=CARTESIAN_POINT('Ctrl Pts',(-6.05147833536176,-1.19585835744747,
28.6174917531058));
#34432=CARTESIAN_POINT('Ctrl Pts',(-4.74075757107689,-3.94660422473637,
28.7565117486183));
#34433=CARTESIAN_POINT('Ctrl Pts',(-2.27325735567634,-5.73434985410667,
28.8955317441309));
#34434=CARTESIAN_POINT('Ctrl Pts',(0.748934247486209,-6.12287226286585,
29.0345517396433));
#34435=CARTESIAN_POINT('Ctrl Pts',(3.58838042763567,-5.01736914737103,29.1735717351559));
#34436=CARTESIAN_POINT('Ctrl Pts',(5.55223559110895,-2.68759133709957,29.3125917306684));
#34437=CARTESIAN_POINT('Ctrl Pts',(6.16130474343239,0.297978376710887,29.4516117261809));
#34438=CARTESIAN_POINT('Ctrl Pts',(5.26697056571692,3.21083919159792,29.5906317216934));
#34439=CARTESIAN_POINT('Ctrl Pts',(3.08745712525581,5.34023180715378,29.729651717206));
#34440=CARTESIAN_POINT('Ctrl Pts',(0.154581610242292,6.16656888230436,29.8686717127185));
#34441=CARTESIAN_POINT('Ctrl Pts',(-2.81601294599354,5.48821813910729,30.007691708231));
#34442=CARTESIAN_POINT('Ctrl Pts',(-5.09947978874435,3.47070211032544,30.1467117037435));
#34443=CARTESIAN_POINT('Ctrl Pts',(-6.1386363408808,0.606309433249525,30.285731699256));
#34444=CARTESIAN_POINT('Ctrl Pts',(-5.67992081866231,-2.40602717111763,
30.4247516947685));
#34445=CARTESIAN_POINT('Ctrl Pts',(-3.83526315776992,-4.83127558364066,
30.5637716902811));
#34446=CARTESIAN_POINT('Ctrl Pts',(-1.05477329200035,-6.07765748927269,
30.7027916857935));
#34447=CARTESIAN_POINT('Ctrl Pts',(1.98308895602633,-5.84104660543947,30.8418116813061));
#34448=CARTESIAN_POINT('Ctrl Pts',(4.53706302380495,-4.17917771486826,30.9808316768186));
#34449=CARTESIAN_POINT('Ctrl Pts',(5.98396059681105,-1.49755895718416,31.1198516723311));
#34450=CARTESIAN_POINT('Ctrl Pts',(5.97072810602557,1.5494751170464,31.2588716678436));
#34451=CARTESIAN_POINT('Ctrl Pts',(4.50059437578687,4.21842595277733,31.3978916633562));
#34452=CARTESIAN_POINT('Ctrl Pts',(1.93228276708425,5.8580500648645,31.5369116588686));
#34453=CARTESIAN_POINT('Ctrl Pts',(-1.10751994091965,6.06826720200214,31.6759316543812));
#34454=CARTESIAN_POINT('Ctrl Pts',(-3.87707969932138,4.79778284831023,31.8149516498937));
#34455=CARTESIAN_POINT('Ctrl Pts',(-5.70060371147976,2.35660445961832,31.9539716454062));
#34456=CARTESIAN_POINT('Ctrl Pts',(-6.13313880814805,-0.659602618565238,
32.0929916409187));
#34457=CARTESIAN_POINT('Ctrl Pts',(-5.06914326857582,-3.51486184324249,
32.2320116364313));
#34458=CARTESIAN_POINT('Ctrl Pts',(-2.76823977074293,-5.51246912246289,
32.3710316319438));
#34459=CARTESIAN_POINT('Ctrl Pts',(0.208134437107512,-6.16499369914678,
32.5100516274563));
#34460=CARTESIAN_POINT('Ctrl Pts',(3.13372232308735,-5.31321481367108,32.6490716229688));
#34461=CARTESIAN_POINT('Ctrl Pts',(5.29465908854464,-3.16497273140251,32.7880916184813));
#34462=CARTESIAN_POINT('Ctrl Pts',(6.16366038958201,-0.24445420087921,32.9271116139939));
#34463=CARTESIAN_POINT('Ctrl Pts',(5.5286835657256,2.73571293898048,33.0661316095063));
#34464=CARTESIAN_POINT('Ctrl Pts',(3.54466759682403,5.04834615319267,33.2051516050189));
#34465=CARTESIAN_POINT('Ctrl Pts',(0.695726861033372,6.12914605710014,33.3441716005314));
#34466=CARTESIAN_POINT('Ctrl Pts',(-2.32297630710416,5.71438958516676,33.4831915960439));
#34467=CARTESIAN_POINT('Ctrl Pts',(-4.7748563004224,3.90528034393773,33.6222115915565));
#34468=CARTESIAN_POINT('Ctrl Pts',(-6.06163650377092,1.14325419333651,33.761231587069));
#34469=CARTESIAN_POINT('Ctrl Pts',(-5.86933315505708,-1.89773432528826,
33.9002515825815));
#34470=CARTESIAN_POINT('Ctrl Pts',(-4.24486967502917,-4.47566181658616,
34.039271578094));
#34471=CARTESIAN_POINT('Ctrl Pts',(-1.5846270101099,-5.96149515585307,34.1782915736065));
#34472=CARTESIAN_POINT('Ctrl Pts',(1.46227621179747,-5.99268016290215,34.317311569119));
#34473=CARTESIAN_POINT('Ctrl Pts',(4.15237336456894,-4.56160746838747,34.4563315646316));
#34474=CARTESIAN_POINT('Ctrl Pts',(5.82926110735099,-2.01746925546705,34.595351560144));
#34475=CARTESIAN_POINT('Ctrl Pts',(6.08376659095337,1.01894618171386,34.7343715556566));
#34476=CARTESIAN_POINT('Ctrl Pts',(4.85378861968884,3.80673131305699,34.8733915511691));
#34477=CARTESIAN_POINT('Ctrl Pts',(2.43945079641032,5.66564621789277,35.0124115466816));
#34478=CARTESIAN_POINT('Ctrl Pts',(-0.570130827249739,6.14210209083577,
35.1514315421941));
#34479=CARTESIAN_POINT('Ctrl Pts',(-3.44059636755775,5.1198402211376,35.2904515377066));
#34480=CARTESIAN_POINT('Ctrl Pts',(-5.47153128055505,2.84829996670597,35.4294715332192));
#34481=CARTESIAN_POINT('Ctrl Pts',(-6.16737262325507,-0.118246269934136,
35.5684915287317));
#34482=CARTESIAN_POINT('Ctrl Pts',(-5.3583300289488,-3.05593955360628,35.7075115242442));
#34483=CARTESIAN_POINT('Ctrl Pts',(-3.24181579601662,-5.24796128026178,
35.8465315197567));
#34484=CARTESIAN_POINT('Ctrl Pts',(-0.334274846170438,-6.15944214857542,
35.9855515152693));
#34485=CARTESIAN_POINT('Ctrl Pts',(2.65483160608277,-5.56797417359075,36.1245715107817));
#34486=CARTESIAN_POINT('Ctrl Pts',(4.9961397682852,-3.61787985845148,36.2635915062943));
#34487=CARTESIAN_POINT('Ctrl Pts',(6.11835335916549,-0.784996450194473,
36.4026115018067));
#34488=CARTESIAN_POINT('Ctrl Pts',(5.74764407127912,2.23943182176189,36.5416314973193));
#34489=CARTESIAN_POINT('Ctrl Pts',(3.97446767675429,4.71742238313097,36.6806514928318));
#34490=CARTESIAN_POINT('Ctrl Pts',(1.23149215863742,6.04432744957155,36.8196714883444));
#34491=CARTESIAN_POINT('Ctrl Pts',(-1.81197643510369,5.89637249951686,36.9586914838568));
#34492=CARTESIAN_POINT('Ctrl Pts',(-4.41330955268765,4.30965962073406,37.0977114793694));
#34493=CARTESIAN_POINT('Ctrl Pts',(-5.93776292575391,1.67135833739262,37.2367314748819));
#34494=CARTESIAN_POINT('Ctrl Pts',(-6.01335880397298,-1.37476657986381,
37.3757514703944));
#34495=CARTESIAN_POINT('Ctrl Pts',(-4.62165124126933,-4.08543841692705,
37.5147714659069));
#34496=CARTESIAN_POINT('Ctrl Pts',(-2.10222704130489,-5.7992334597976,37.6537914614195));
#34497=CARTESIAN_POINT('Ctrl Pts',(0.930155901329192,-6.0979732086696,37.7928114569319));
#34498=CARTESIAN_POINT('Ctrl Pts',(3.73557401463809,-4.90876298425484,37.9318314524445));
#34499=CARTESIAN_POINT('Ctrl Pts',(5.62948480164565,-2.52177876160262,38.070851447957));
#34500=CARTESIAN_POINT('Ctrl Pts',(6.14976020627442,0.480537885866896,38.2098714434695));
#34501=CARTESIAN_POINT('Ctrl Pts',(5.16944923219678,3.36559978163918,38.348891438982));
#34502=CARTESIAN_POINT('Ctrl Pts',(2.92775491258089,5.42943076448057,38.4879114344945));
#34503=CARTESIAN_POINT('Ctrl Pts',(-0.0283329759951614,6.16844101024732,
38.6269314300071));
#34504=CARTESIAN_POINT('Ctrl Pts',(-2.97750741162013,5.40230662478325,38.7659514255196));
#34505=CARTESIAN_POINT('Ctrl Pts',(-5.20014830536553,3.31796999031538,38.9049714210321));
#34506=CARTESIAN_POINT('Ctrl Pts',(-6.15391505564063,0.424024459659371,
39.0439914165446));
#34507=CARTESIAN_POINT('Ctrl Pts',(-5.60608161363686,-2.57338613419603,
39.1830114120571));
#34508=CARTESIAN_POINT('Ctrl Pts',(-3.69032333795313,-4.94287172762838,
39.3220314075697));
#34509=CARTESIAN_POINT('Ctrl Pts',(-0.874099231373308,-6.10626054047339,
39.4610514030821));
#34510=CARTESIAN_POINT('Ctrl Pts',(2.15541146789322,-5.77967721058055,39.6000713985947));
#34511=CARTESIAN_POINT('Ctrl Pts',(4.65898603619837,-4.04281045424319,39.7390913941072));
#34512=CARTESIAN_POINT('Ctrl Pts',(6.02573400476567,-1.3194684377584,39.8781113896197));
#34513=CARTESIAN_POINT('Ctrl Pts',(5.92215889308766,1.72583350861328,40.0171313851323));
#34514=CARTESIAN_POINT('Ctrl Pts',(4.37353378443007,4.35001948166654,40.1561513806447));
#34515=CARTESIAN_POINT('Ctrl Pts',(1.75773450904124,5.91276894949864,40.2951713761573));
#34516=CARTESIAN_POINT('Ctrl Pts',(-1.28696481662245,6.03275963512601,40.4341913716697));
#34517=CARTESIAN_POINT('Ctrl Pts',(-4.01763533320709,4.68071293541866,40.5732113671824));
#34518=CARTESIAN_POINT('Ctrl Pts',(-5.76797350293554,2.18653811397452,40.7122313626948));
#34519=CARTESIAN_POINT('Ctrl Pts',(-6.11088403631264,-0.841167967274665,
40.8512513582074));
#34520=CARTESIAN_POINT('Ctrl Pts',(-4.96269426021928,-3.66362292464934,
40.9902713537199));
#34521=CARTESIAN_POINT('Ctrl Pts',(-2.6035708608976,-5.5921271468659,41.1292913492324));
#34522=CARTESIAN_POINT('Ctrl Pts',(0.390842832486891,-6.15611152715116,
41.2683113447449));
#34523=CARTESIAN_POINT('Ctrl Pts',(3.28988802190165,-5.21795976007649,41.4073313402574));
#34524=CARTESIAN_POINT('Ctrl Pts',(5.38617652039734,-3.00658772457253,41.54635133577));
#34525=CARTESIAN_POINT('Ctrl Pts',(6.16819863309635,-0.061586338565383,
41.6853713312824));
#34526=CARTESIAN_POINT('Ctrl Pts',(5.44513525635857,2.89844256358317,41.8243913267949));
#34527=CARTESIAN_POINT('Ctrl Pts',(3.39341913189756,5.15123032388393,41.9634113223075));
#34528=CARTESIAN_POINT('Ctrl Pts',(0.513683969983391,6.14708028525834,42.10243131782));
#34529=CARTESIAN_POINT('Ctrl Pts',(-2.49139383009257,5.64299778821561,42.2414513133325));
#34530=CARTESIAN_POINT('Ctrl Pts',(-4.8885533504256,3.76198264143688,42.3804713088451));
#34531=CARTESIAN_POINT('Ctrl Pts',(-6.09287017068981,0.963016270655894,
42.5194913043575));
#34532=CARTESIAN_POINT('Ctrl Pts',(-5.81048219618248,-2.07093309942065,
42.6585112998701));
#34533=CARTESIAN_POINT('Ctrl Pts',(-4.1102941538918,-4.59955967706829,42.7975312953826));
#34534=CARTESIAN_POINT('Ctrl Pts',(-1.40716433616188,-6.00586012037109,
42.9365512908951));
#34535=CARTESIAN_POINT('Ctrl Pts',(1.63932385077592,-5.94668685628449,43.0755712864076));
#34536=CARTESIAN_POINT('Ctrl Pts',(4.28580505235956,-4.43647859316362,43.2145912819201));
#34537=CARTESIAN_POINT('Ctrl Pts',(5.88651853818737,-1.84373717053327,43.3536112774327));
#34538=CARTESIAN_POINT('Ctrl Pts',(6.05087853377761,1.19888957952724,43.4926312729452));
#34539=CARTESIAN_POINT('Ctrl Pts',(4.73878000050854,3.94897852123938,43.6316512684577));
#34540=CARTESIAN_POINT('Ctrl Pts',(2.27038455777718,5.73548787935574,43.7706712639702));
#34541=CARTESIAN_POINT('Ctrl Pts',(-0.75200128905964,6.12249633039352,43.9096912594827));
#34542=CARTESIAN_POINT('Ctrl Pts',(-3.59089333235252,5.0155709874446,44.0487112549953));
#34543=CARTESIAN_POINT('Ctrl Pts',(-5.55358119187607,2.68480971386613,44.1877312505077));
#34544=CARTESIAN_POINT('Ctrl Pts',(-6.16115470384076,-0.301064726878676,
44.3267512460203));
#34545=CARTESIAN_POINT('Ctrl Pts',(-5.26536149652208,-3.21347717673118,
44.4657712415327));
#34546=CARTESIAN_POINT('Ctrl Pts',(-3.08478165108631,-5.34177773962483,
44.6047912370454));
#34547=CARTESIAN_POINT('Ctrl Pts',(-0.151492566324147,-6.16664554330616,
44.7438112325578));
#34548=CARTESIAN_POINT('Ctrl Pts',(2.81876181039641,-5.48680682279593,44.8828312280704));
#34549=CARTESIAN_POINT('Ctrl Pts',(5.10121773065381,-3.46814718818215,45.0218512235828));
#34550=CARTESIAN_POINT('Ctrl Pts',(6.13893928978386,-0.603234324926554,
45.1608712190954));
#34551=CARTESIAN_POINT('Ctrl Pts',(5.67871485281819,2.40887211674427,45.2998912146079));
#34552=CARTESIAN_POINT('Ctrl Pts',(3.83284254164173,4.83319617907093,45.4389112101205));
#34553=CARTESIAN_POINT('Ctrl Pts',(1.05172867360261,6.07818509520536,45.5779312056329));
#34554=CARTESIAN_POINT('Ctrl Pts',(-1.98601466760215,5.84005248217085,45.7169512011455));
#34555=CARTESIAN_POINT('Ctrl Pts',(-4.53915593353827,4.176904435742,45.8559711966579));
#34556=CARTESIAN_POINT('Ctrl Pts',(-5.98471001952974,1.49456121888098,45.9949911921705));
#34557=CARTESIAN_POINT('Ctrl Pts',(-5.96995117696109,-1.55246584446183,
46.134011187683));
#34558=CARTESIAN_POINT('Ctrl Pts',(-4.49848067160452,-4.22067991005896,
46.2730311831955));
#34559=CARTESIAN_POINT('Ctrl Pts',(-1.92934804644225,-5.85901726984058,
46.412051178708));
#34560=CARTESIAN_POINT('Ctrl Pts',(1.11055958361069,-6.06771164987773,46.5510711742206));
#34561=CARTESIAN_POINT('Ctrl Pts',(3.879482571308,-4.79584009731413,46.6900911697331));
#34562=CARTESIAN_POINT('Ctrl Pts',(5.7017834900662,-2.35374855623714,46.8291111652456));
#34563=CARTESIAN_POINT('Ctrl Pts',(6.1328076273202,0.662674815135318,46.9681311607581));
#34564=CARTESIAN_POINT('Ctrl Pts',(5.06738192214114,3.51740069056444,47.1071511562706));
#34565=CARTESIAN_POINT('Ctrl Pts',(2.76547807274594,5.51385513116234,47.2461711517831));
#34566=CARTESIAN_POINT('Ctrl Pts',(-0.211222675940933,6.16488865755735,
47.3851911472957));
#34567=CARTESIAN_POINT('Ctrl Pts',(-3.13638342552245,5.31164438281825,47.5242111428081));
#34568=CARTESIAN_POINT('Ctrl Pts',(-5.29624396900741,3.16232004910531,47.6632311383208));
#34569=CARTESIAN_POINT('Ctrl Pts',(-6.16378185167675,0.241366655694626,
47.8022511338331));
#34570=CARTESIAN_POINT('Ctrl Pts',(-5.5273128969791,-2.73848218739485,47.9412711293458));
#34571=CARTESIAN_POINT('Ctrl Pts',(-3.5421374446362,-5.05012095098419,48.0802911248582));
#34572=CARTESIAN_POINT('Ctrl Pts',(-0.692658125609615,-6.12949419366117,
48.2193111203708));
#34573=CARTESIAN_POINT('Ctrl Pts',(2.3258417114082,-5.71322444769426,48.3583311158833));
#34574=CARTESIAN_POINT('Ctrl Pts',(4.7768057663147,-3.90288948418925,48.4973511113958));
#34575=CARTESIAN_POINT('Ctrl Pts',(6.06222055645793,-1.14021465560235,48.6363711069083));
#34576=CARTESIAN_POINT('Ctrl Pts',(5.86835812258636,1.900668491112,48.7753911024208));
#34577=CARTESIAN_POINT('Ctrl Pts',(4.24267335475951,4.47779881807613,48.9144110979333));
#34578=CARTESIAN_POINT('Ctrl Pts',(1.58155006867202,5.96226637531529,49.0534310934459));
#34579=CARTESIAN_POINT('Ctrl Pts',(-1.46509874999526,5.99198956129919,49.1924510889584));
#34580=CARTESIAN_POINT('Ctrl Pts',(-4.15503569018137,4.55944298225233,49.3314710844709));
#34581=CARTESIAN_POINT('Ctrl Pts',(-5.27116507023042,2.86295887331669,49.4241510814793));
#34582=CARTESIAN_POINT('Ctrl Pts',(-5.5926845116257,1.9324550623107,49.4704910799834));
#34583=CARTESIAN_POINT('Ctrl Pts',(3.24353530767675,-4.54538816146824,-0.3843885632452));
#34584=CARTESIAN_POINT('Ctrl Pts',(3.99988254819268,-4.00566902158514,-0.338043015427469));
#34585=CARTESIAN_POINT('Ctrl Pts',(5.23710322327956,-2.54200492850901,-0.245357469105566));
#34586=CARTESIAN_POINT('Ctrl Pts',(5.81469291328025,0.275550394094319,-0.106331924279489));
#34587=CARTESIAN_POINT('Ctrl Pts',(4.97347786147395,3.02500010026102,0.0326880712330279));
#34588=CARTESIAN_POINT('Ctrl Pts',(2.91867860759893,5.03670007919148,0.171708066745545));
#34589=CARTESIAN_POINT('Ctrl Pts',(0.151709961649961,5.81921915220708,0.310728062258062));
#34590=CARTESIAN_POINT('Ctrl Pts',(-2.65228184789175,5.18190313468451,0.449748057770581));
#34591=CARTESIAN_POINT('Ctrl Pts',(-4.80909505824059,3.28011531771315,0.588768053283096));
#34592=CARTESIAN_POINT('Ctrl Pts',(-5.79245523628694,0.577980837100627,
0.727788048795615));
#34593=CARTESIAN_POINT('Ctrl Pts',(-5.36241340853576,-2.26519820802741,
0.866808044308132));
#34594=CARTESIAN_POINT('Ctrl Pts',(-3.62390389962763,-4.55564568490122,
1.00582803982065));
#34595=CARTESIAN_POINT('Ctrl Pts',(-1.00113521754353,-5.73448578002076,
1.14484803533317));
#34596=CARTESIAN_POINT('Ctrl Pts',(1.86591767799704,-5.51406773646999,1.28386803084568));
#34597=CARTESIAN_POINT('Ctrl Pts',(4.27767308501967,-3.94817781406936,1.42288802635821));
#34598=CARTESIAN_POINT('Ctrl Pts',(5.645645012807,-1.41890322681348,1.56190802187072));
#34599=CARTESIAN_POINT('Ctrl Pts',(5.63603836045111,1.45659386915713,1.70092801738324));
#34600=CARTESIAN_POINT('Ctrl Pts',(4.25119720352968,3.97667154972591,1.83994801289576));
#34601=CARTESIAN_POINT('Ctrl Pts',(1.82903290165202,5.52641228379608,1.97896800840828));
#34602=CARTESIAN_POINT('Ctrl Pts',(-1.03942878029484,5.72766811386036,2.11798800392079));
#34603=CARTESIAN_POINT('Ctrl Pts',(-3.65426225203626,4.53133110047943,2.25700799943331));
#34604=CARTESIAN_POINT('Ctrl Pts',(-5.37742906147621,2.22931623176881,2.39602799494583));
#34605=CARTESIAN_POINT('Ctrl Pts',(-5.78846392873392,-0.616668073994028,
2.53504799045834));
#34606=CARTESIAN_POINT('Ctrl Pts',(-4.78707134629015,-3.31218086633208,
2.67406798597086));
#34607=CARTESIAN_POINT('Ctrl Pts',(-2.61759841346924,-5.19949735210785,
2.81308798148338));
#34608=CARTESIAN_POINT('Ctrl Pts',(0.190587638603466,-5.81809853118683,
2.95210797699589));
#34609=CARTESIAN_POINT('Ctrl Pts',(2.95226891573283,-5.01704120144163,3.09112797250841));
#34610=CARTESIAN_POINT('Ctrl Pts',(4.99357502819268,-2.9917891979699,3.23014796802093));
#34611=CARTESIAN_POINT('Ctrl Pts',(5.8164123846374,-0.236518792580586,3.36916796353344));
#34612=CARTESIAN_POINT('Ctrl Pts',(5.22000266402811,2.57646392463758,3.50818795904597));
#34613=CARTESIAN_POINT('Ctrl Pts',(3.34987419151473,4.76077063807932,3.64720795455848));
#34614=CARTESIAN_POINT('Ctrl Pts',(0.662351964844652,5.78341456598765,3.786227950071));
#34615=CARTESIAN_POINT('Ctrl Pts',(-2.18678897589165,5.3948631254471,3.92524794558351));
#34616=CARTESIAN_POINT('Ctrl Pts',(-4.50233744468419,3.68992570407515,4.06426794109604));
#34617=CARTESIAN_POINT('Ctrl Pts',(-5.71928271347876,1.08461947737435,4.20328793660855));
#34618=CARTESIAN_POINT('Ctrl Pts',(-5.54068125395366,-1.78534181866763,
4.34230793212107));
#34619=CARTESIAN_POINT('Ctrl Pts',(-4.01011312588206,-4.2196666793748,4.48132792763359));
#34620=CARTESIAN_POINT('Ctrl Pts',(-1.50104812444773,-5.62436207009194,
4.6203479231461));
#34621=CARTESIAN_POINT('Ctrl Pts',(1.37428357581349,-5.65667206232133,4.75936791865862));
#34622=CARTESIAN_POINT('Ctrl Pts',(3.91428005239532,-4.3087127821215,4.89838791417113));
#34623=CARTESIAN_POINT('Ctrl Pts',(5.49916362505065,-1.90939613289568,5.03740790968366));
#34624=CARTESIAN_POINT('Ctrl Pts',(5.74221113365761,0.95582710983514,5.17642790519617));
#34625=CARTESIAN_POINT('Ctrl Pts',(4.58411721206192,3.58782156098583,5.31544790070869));
#34626=CARTESIAN_POINT('Ctrl Pts',(2.30746523030072,5.34436136300218,5.45446789622121));
#34627=CARTESIAN_POINT('Ctrl Pts',(-0.532225110321242,5.79683798284382,
5.59348789173372));
#34628=CARTESIAN_POINT('Ctrl Pts',(-3.24204863920333,4.83484382254867,5.73250788724625));
#34629=CARTESIAN_POINT('Ctrl Pts',(-5.16078863573428,2.69311247902369,5.87152788275876));
#34630=CARTESIAN_POINT('Ctrl Pts',(-5.8202585354793,-0.105757966969696,
6.01054787827129));
#34631=CARTESIAN_POINT('Ctrl Pts',(-5.05954286929301,-2.87882269707314,
6.14956787378379));
#34632=CARTESIAN_POINT('Ctrl Pts',(-3.06426181234631,-4.94943367596671,
6.28858786929631));
#34633=CARTESIAN_POINT('Ctrl Pts',(-0.321278506504521,-5.81234671098133,
6.42760786480884));
#34634=CARTESIAN_POINT('Ctrl Pts',(2.50009910000284,-5.25700472299219,6.56662786032134));
#34635=CARTESIAN_POINT('Ctrl Pts',(4.71143427736757,-3.41891521062502,6.70564785583387));
#34636=CARTESIAN_POINT('Ctrl Pts',(5.77314510131853,-0.746585431494017,
6.84466785134638));
#34637=CARTESIAN_POINT('Ctrl Pts',(5.42616638116412,2.10791664240345,6.98368784685891));
#34638=CARTESIAN_POINT('Ctrl Pts',(3.7551634572917,4.44807166943365,7.12270784237141));
#34639=CARTESIAN_POINT('Ctrl Pts',(1.16787324012308,5.70286474172425,7.26172783788393));
#34640=CARTESIAN_POINT('Ctrl Pts',(-1.70438657218461,5.56611719064143,7.40074783339646));
#34641=CARTESIAN_POINT('Ctrl Pts',(-4.16076362020811,4.07119641679812,7.53976782890896));
#34642=CARTESIAN_POINT('Ctrl Pts',(-5.6018839746241,1.58287400074895,7.67878782442149));
#34643=CARTESIAN_POINT('Ctrl Pts',(-5.67610374991866,-1.29168122520867,
7.81780781993401));
#34644=CARTESIAN_POINT('Ctrl Pts',(-4.36531277917439,-3.85105680396615,
7.95682781544651));
#34645=CARTESIAN_POINT('Ctrl Pts',(-1.98935362698809,-5.47074641289345,
8.09584781095906));
#34646=CARTESIAN_POINT('Ctrl Pts',(0.872022330888087,-5.75553396496188,
8.23486780647155));
#34647=CARTESIAN_POINT('Ctrl Pts',(3.52061847495569,-4.63592921874331,8.37388780198407));
#34648=CARTESIAN_POINT('Ctrl Pts',(5.31015801340958,-2.38512390454236,8.51290779749659));
#34649=CARTESIAN_POINT('Ctrl Pts',(5.80398023664667,0.447669051881049,8.6519277930091));
#34650=CARTESIAN_POINT('Ctrl Pts',(4.88158891768631,3.17122749201622,8.79094778852162));
#34651=CARTESIAN_POINT('Ctrl Pts',(2.76805427108038,5.12098327665214,8.92996778403414));
#34652=CARTESIAN_POINT('Ctrl Pts',(-0.0209058222714769,5.82118176266575,
9.06898777954667));
#34653=CARTESIAN_POINT('Ctrl Pts',(-2.80476474239316,5.10096940857573,9.20800777505916));
#34654=CARTESIAN_POINT('Ctrl Pts',(-4.90424059281125,3.13608328575942,9.34702777057171));
#34655=CARTESIAN_POINT('Ctrl Pts',(-5.80704594151402,0.405969950295367,
9.4860477660842));
#34656=CARTESIAN_POINT('Ctrl Pts',(-5.29288969365446,-2.42320301629962,
9.62506776159673));
#34657=CARTESIAN_POINT('Ctrl Pts',(-3.48722972664344,-4.66109675945605,
9.76408775710924));
#34658=CARTESIAN_POINT('Ctrl Pts',(-0.83066025231826,-5.76164887099307,
9.90310775262178));
#34659=CARTESIAN_POINT('Ctrl Pts',(2.02859638673404,-5.45631660253753,10.0421277481342));
#34660=CARTESIAN_POINT('Ctrl Pts',(4.39286070027743,-3.81960325627614,10.1811477436468));
#34661=CARTESIAN_POINT('Ctrl Pts',(5.68523493855165,-1.25087883540689,10.3201677391593));
#34662=CARTESIAN_POINT('Ctrl Pts',(5.59037035411014,1.62306915172573,10.4591877346718));
#34663=CARTESIAN_POINT('Ctrl Pts',(4.13141459799293,4.10097641871886,10.5982077301843));
#34664=CARTESIAN_POINT('Ctrl Pts',(1.66436352391329,5.57821550566704,10.7372277256968));
#34665=CARTESIAN_POINT('Ctrl Pts',(-1.20880439853578,5.69432929268037,10.8762477212093));
#34666=CARTESIAN_POINT('Ctrl Pts',(-3.78701522442807,4.42098516818901,11.0152677167219));
#34667=CARTESIAN_POINT('Ctrl Pts',(-5.44116669335026,2.06888839297171,11.1542877122344));
#34668=CARTESIAN_POINT('Ctrl Pts',(-5.76763377289058,-0.788032251376195,
11.2933077077469));
#34669=CARTESIAN_POINT('Ctrl Pts',(-4.68675611269034,-3.45266727437747,
11.4323277032594));
#34670=CARTESIAN_POINT('Ctrl Pts',(-2.46227575138857,-5.27482628069598,
11.5713476987719));
#34671=CARTESIAN_POINT('Ctrl Pts',(0.363017865913463,-5.8098891724735,11.7103676942845));
#34672=CARTESIAN_POINT('Ctrl Pts',(3.0997324741899,-4.92729669858126,11.849387689797));
#34673=CARTESIAN_POINT('Ctrl Pts',(5.08008973317371,-2.8424078648745,11.9884076853095));
#34674=CARTESIAN_POINT('Ctrl Pts',(5.82086801663436,-0.063950764813749,
12.127427680822));
#34675=CARTESIAN_POINT('Ctrl Pts',(5.14131201631318,2.73011078865145,12.2664476763345));
#34676=CARTESIAN_POINT('Ctrl Pts',(3.20723835650867,4.85800538204074,12.405467671847));
#34677=CARTESIAN_POINT('Ctrl Pts',(0.490575127418006,5.8005112026231,12.5444876673595));
#34678=CARTESIAN_POINT('Ctrl Pts',(-2.34579201357227,5.32764995063094,12.6835076628721));
#34679=CARTESIAN_POINT('Ctrl Pts',(-4.60976878082841,3.55480322306271,12.8225276583846));
#34680=CARTESIAN_POINT('Ctrl Pts',(-5.74892831790386,0.914558561821075,
12.9615476538971));
#34681=CARTESIAN_POINT('Ctrl Pts',(-5.48530738279048,-1.94884506405755,
13.1005676494096));
#34682=CARTESIAN_POINT('Ctrl Pts',(-3.88323140787979,-4.33671626928177,
13.2395876449221));
#34683=CARTESIAN_POINT('Ctrl Pts',(-1.33361862493489,-5.66639705020959,
13.3786076404346));
#34684=CARTESIAN_POINT('Ctrl Pts',(1.5414068368531,-5.61343559067883,13.5176276359472));
#34685=CARTESIAN_POINT('Ctrl Pts',(4.04031777940071,-4.19075487339164,13.6566476314597));
#34686=CARTESIAN_POINT('Ctrl Pts',(5.55336169265697,-1.74549937780777,13.7956676269722));
#34687=CARTESIAN_POINT('Ctrl Pts',(5.711344817766,1.12567070672322,13.9346876224847));
#34688=CARTESIAN_POINT('Ctrl Pts',(4.47571811904957,3.72216892230976,14.0737076179972));
#34689=CARTESIAN_POINT('Ctrl Pts',(2.14798353009009,5.41043075196965,14.2127276135098));
#34690=CARTESIAN_POINT('Ctrl Pts',(-0.703874718788708,5.7785079862926,14.3517476090223));
#34691=CARTESIAN_POINT('Ctrl Pts',(-3.38398239855548,4.73658709343171,14.4907676045348));
#34692=CARTESIAN_POINT('Ctrl Pts',(-5.23837367268526,2.53890437644177,14.6297876000473));
#34693=CARTESIAN_POINT('Ctrl Pts',(-5.81456353470378,-0.278289540389685,
14.7688075955598));
#34694=CARTESIAN_POINT('Ctrl Pts',(-4.97195745254918,-3.02757877807298,
14.9078275910723));
#34695=CARTESIAN_POINT('Ctrl Pts',(-2.91615746062379,-5.03811669498091,
15.0468475865849));
#34696=CARTESIAN_POINT('Ctrl Pts',(-0.148793762668019,-5.81931736405468,
15.1858675820974));
#34697=CARTESIAN_POINT('Ctrl Pts',(2.65487669945529,-5.18056211989457,15.3248875776099));
#34698=CARTESIAN_POINT('Ctrl Pts',(4.81073786841581,-3.27771190448267,15.4639075731224));
#34699=CARTESIAN_POINT('Ctrl Pts',(5.79274388290926,-0.575076059677866,
15.6029275686349));
#34700=CARTESIAN_POINT('Ctrl Pts',(5.36127810753363,2.26788254128779,15.7419475641475));
#34701=CARTESIAN_POINT('Ctrl Pts',(3.62162134083876,4.55746124843408,15.88096755966));
#34702=CARTESIAN_POINT('Ctrl Pts',(0.998262532013878,5.73498614510745,16.0199875551725));
#34703=CARTESIAN_POINT('Ctrl Pts',(-1.86867962114769,5.51313256152113,16.159007550685));
#34704=CARTESIAN_POINT('Ctrl Pts',(-4.27965030686907,3.94603439142549,16.2980275461975));
#34705=CARTESIAN_POINT('Ctrl Pts',(-5.64635507965907,1.41607502689844,16.43704754171));
#34706=CARTESIAN_POINT('Ctrl Pts',(-5.63530799909529,-1.45941698041719,
16.5760675372226));
#34707=CARTESIAN_POINT('Ctrl Pts',(-4.24920463347018,-3.97880059192374,
16.7150875327351));
#34708=CARTESIAN_POINT('Ctrl Pts',(-1.82626432145237,-5.52732781691002,
16.8541075282476));
#34709=CARTESIAN_POINT('Ctrl Pts',(1.04229781528194,-5.72714670945801,16.9931275237601));
#34710=CARTESIAN_POINT('Ctrl Pts',(3.65653167713951,-4.52950000126642,17.1321475192726));
#34711=CARTESIAN_POINT('Ctrl Pts',(5.37854511999187,-2.22662223100573,17.2711675147851));
#34712=CARTESIAN_POINT('Ctrl Pts',(5.78815429444966,0.619567616197914,17.4101875102977));
#34713=CARTESIAN_POINT('Ctrl Pts',(4.78541157212288,3.31457844269668,17.5492075058102));
#34714=CARTESIAN_POINT('Ctrl Pts',(2.61499349648643,5.20080793538185,17.6882275013227));
#34715=CARTESIAN_POINT('Ctrl Pts',(-0.193502079672655,5.81800233005794,
17.8272474968352));
#34716=CARTESIAN_POINT('Ctrl Pts',(-2.95478173597983,5.01556168939405,17.9662674923477));
#34717=CARTESIAN_POINT('Ctrl Pts',(-4.99507308114313,2.98928738689283,18.1052874878603));
#34718=CARTESIAN_POINT('Ctrl Pts',(-5.81653013443292,0.233605142561025,
18.2443074833728));
#34719=CARTESIAN_POINT('Ctrl Pts',(-5.21871137886108,-2.57907846168803,
18.3833274788853));
#34720=CARTESIAN_POINT('Ctrl Pts',(-3.34748895439027,-4.76244809605651,
18.5223474743978));
#34721=CARTESIAN_POINT('Ctrl Pts',(-0.659454791032004,-5.78374563289069,
18.6613674699103));
#34722=CARTESIAN_POINT('Ctrl Pts',(2.18949115483542,-5.39376701854044,18.8003874654228));
#34723=CARTESIAN_POINT('Ctrl Pts',(4.50418527737289,-3.687669881442,18.9394074609354));
#34724=CARTESIAN_POINT('Ctrl Pts',(5.71982531524873,-1.08175437620428,19.0784274564479));
#34725=CARTESIAN_POINT('Ctrl Pts',(5.53978622601238,1.78811709277684,19.2174474519604));
#34726=CARTESIAN_POINT('Ctrl Pts',(4.00799886158025,4.22167493928282,19.3564674474729));
#34727=CARTESIAN_POINT('Ctrl Pts',(1.49823051970747,5.62511328572272,19.4954874429854));
#34728=CARTESIAN_POINT('Ctrl Pts',(-1.37711700486929,5.6559829315776,19.6345074384979));
#34729=CARTESIAN_POINT('Ctrl Pts',(-3.91643792839529,4.30675145793487,19.7735274340104));
#34730=CARTESIAN_POINT('Ctrl Pts',(-5.50011941049998,1.90664119268375,19.912547429523));
#34731=CARTESIAN_POINT('Ctrl Pts',(-5.74173160993018,-0.958703440551738,
20.0515674250355));
#34732=CARTESIAN_POINT('Ctrl Pts',(-4.58231938644739,-3.59011743651731,
20.190587420548));
#34733=CARTESIAN_POINT('Ctrl Pts',(-2.30478778537174,-5.34551657296078,
20.3296074160606));
#34734=CARTESIAN_POINT('Ctrl Pts',(0.535128858458774,-5.79657064756757,
20.468627411573));
#34735=CARTESIAN_POINT('Ctrl Pts',(3.24447015480882,-4.83321917379629,20.6076474070856));
#34736=CARTESIAN_POINT('Ctrl Pts',(5.16213705132485,-2.69052694294937,20.7466674025981));
#34737=CARTESIAN_POINT('Ctrl Pts',(5.82020482780844,0.108673500691432,20.8856873981106));
#34738=CARTESIAN_POINT('Ctrl Pts',(5.05810014342445,2.88135681693307,21.0247073936231));
#34739=CARTESIAN_POINT('Ctrl Pts',(3.06178210392277,4.95096803822197,21.1637273891357));
#34740=CARTESIAN_POINT('Ctrl Pts',(0.318366882481225,5.81250692004203,21.3027473846481));
#34741=CARTESIAN_POINT('Ctrl Pts',(-2.50273218211169,5.25575168667811,21.4417673801607));
#34742=CARTESIAN_POINT('Ctrl Pts',(-4.71314632630798,3.41655467894293,21.5807873756732));
#34743=CARTESIAN_POINT('Ctrl Pts',(-5.7735183646524,0.743693391404382,21.7198073711857));
#34744=CARTESIAN_POINT('Ctrl Pts',(-5.4251097799135,-2.11063451200913,21.8588273666982));
#34745=CARTESIAN_POINT('Ctrl Pts',(-3.7529348098741,-4.44995218853332,21.9978473622107));
#34746=CARTESIAN_POINT('Ctrl Pts',(-1.16501635277576,-5.70344904993131,
22.1368673577233));
#34747=CARTESIAN_POINT('Ctrl Pts',(1.70717459809594,-5.56526271248836,22.2758873532358));
#34748=CARTESIAN_POINT('Ctrl Pts',(4.16280248601068,-4.06911165119126,22.4149073487483));
#34749=CARTESIAN_POINT('Ctrl Pts',(5.60267618217995,-1.5800676457135,22.5539273442608));
#34750=CARTESIAN_POINT('Ctrl Pts',(5.67545599480169,1.29452439855982,22.6929473397733));
#34751=CARTESIAN_POINT('Ctrl Pts',(4.36338311836127,3.85324304058244,22.8319673352858));
#34752=CARTESIAN_POINT('Ctrl Pts',(1.9866129118022,5.47174225508275,22.9709873307984));
#34753=CARTESIAN_POINT('Ctrl Pts',(-0.874905345936364,5.75509641996111,
23.1100073263109));
#34754=CARTESIAN_POINT('Ctrl Pts',(-3.52294031315086,4.63416505072638,23.2490273218234));
#34755=CARTESIAN_POINT('Ctrl Pts',(-5.31135212928438,2.38246358338242,23.3880473173359));
#34756=CARTESIAN_POINT('Ctrl Pts',(-5.80375525721159,-0.450576388402698,
23.5270673128484));
#34757=CARTESIAN_POINT('Ctrl Pts',(-4.87999973956568,-3.17367243256704,
23.666087308361));
#34758=CARTESIAN_POINT('Ctrl Pts',(-2.76548866533538,-5.12236923789166,
23.8051073038735));
#34759=CARTESIAN_POINT('Ctrl Pts',(0.0238218291122001,-5.82117055993508,
23.944127299386));
#34760=CARTESIAN_POINT('Ctrl Pts',(2.80731962337594,-5.09956377542292,24.0831472948985));
#34761=CARTESIAN_POINT('Ctrl Pts',(4.90581093832766,-3.13362620693373,24.222167290411));
#34762=CARTESIAN_POINT('Ctrl Pts',(5.80724857579574,-0.403060970965061,
24.3611872859235));
#34763=CARTESIAN_POINT('Ctrl Pts',(5.29167517245777,2.42585408394472,24.5002072814361));
#34764=CARTESIAN_POINT('Ctrl Pts',(3.48489440200532,4.66284303555988,24.6392272769485));
#34765=CARTESIAN_POINT('Ctrl Pts',(0.827773960496438,5.76206425143987,24.7782472724611));
#34766=CARTESIAN_POINT('Ctrl Pts',(-2.03132936946743,5.4552997314663,24.9172672679736));
#34767=CARTESIAN_POINT('Ctrl Pts',(-4.39477350618678,3.81740225765061,25.0562872634861));
#34768=CARTESIAN_POINT('Ctrl Pts',(-5.6858608290331,1.24803076895726,25.1953072589986));
#34769=CARTESIAN_POINT('Ctrl Pts',(-5.58955660731777,-1.62586933699712,
25.3343272545112));
#34770=CARTESIAN_POINT('Ctrl Pts',(-4.12935977408376,-4.10304545716667,
25.4733472500237));
#34771=CARTESIAN_POINT('Ctrl Pts',(-1.66156901491974,-5.57904853680768,
25.6123672455362));
#34772=CARTESIAN_POINT('Ctrl Pts',(1.21165671202161,-5.69372305083503,25.7513872410487));
#34773=CARTESIAN_POINT('Ctrl Pts',(3.78922935709598,-4.41908758079302,25.8904072365612));
#34774=CARTESIAN_POINT('Ctrl Pts',(5.44220238066783,-2.06616248520063,26.0294272320737));
#34775=CARTESIAN_POINT('Ctrl Pts',(5.76723829959271,0.790921338129275,26.1684472275863));
#34776=CARTESIAN_POINT('Ctrl Pts',(4.6850259771483,3.45501458185676,26.3074672230988));
#34777=CARTESIAN_POINT('Ctrl Pts',(2.45963311930325,5.27605904874309,26.4464872186113));
#34778=CARTESIAN_POINT('Ctrl Pts',(-0.365928173024152,5.80970659668666,
26.5855072141238));
#34779=CARTESIAN_POINT('Ctrl Pts',(-3.102200320148,4.9257433287851,26.7245272096363));
#34780=CARTESIAN_POINT('Ctrl Pts',(-5.08151294555208,2.83986273463768,26.8635472051489));
#34781=CARTESIAN_POINT('Ctrl Pts',(-5.82089932122442,0.0610349044915131,
27.0025672006613));
#34782=CARTESIAN_POINT('Ctrl Pts',(-5.13994377456644,-2.73268588785704,
27.1415871961739));
#34783=CARTESIAN_POINT('Ctrl Pts',(-3.2048044293984,-4.85961137712736,27.2806071916864));
#34784=CARTESIAN_POINT('Ctrl Pts',(-0.48766941092484,-5.80075621906708,
27.4196271871989));
#34785=CARTESIAN_POINT('Ctrl Pts',(2.34846050341454,-5.32647420263152,27.5586471827114));
#34786=CARTESIAN_POINT('Ctrl Pts',(4.6115489130204,-3.5524936017138,27.697667178224));
#34787=CARTESIAN_POINT('Ctrl Pts',(5.7493857271972,-0.911678631590233,27.8366871737365));
#34788=CARTESIAN_POINT('Ctrl Pts',(5.48433045797889,1.95159257917282,27.975707169249));
#34789=CARTESIAN_POINT('Ctrl Pts',(3.88105852574804,4.33866095553867,28.1147271647615));
#34790=CARTESIAN_POINT('Ctrl Pts',(1.33077998458343,5.66706438996677,28.253747160274));
#34791=CARTESIAN_POINT('Ctrl Pts',(-1.54421858645868,5.61266274816444,28.3927671557865));
#34792=CARTESIAN_POINT('Ctrl Pts',(-4.04241655083305,4.18873042782036,28.531787151299));
#34793=CARTESIAN_POINT('Ctrl Pts',(-5.55423537036727,1.74271730867587,28.6708071468116));
#34794=CARTESIAN_POINT('Ctrl Pts',(-5.71078021801578,-1.12853155424069,
28.8098271423241));
#34795=CARTESIAN_POINT('Ctrl Pts',(-4.47385300829901,-3.72441048053663,
28.9488471378366));
#34796=CARTESIAN_POINT('Ctrl Pts',(-2.14527300897614,-5.41150606433697,
29.0878671333492));
#34797=CARTESIAN_POINT('Ctrl Pts',(0.706769263329594,-5.77815466873377,
29.2268871288616));
#34798=CARTESIAN_POINT('Ctrl Pts',(3.38635467652741,-4.73489135801003,29.3659071243742));
#34799=CARTESIAN_POINT('Ctrl Pts',(5.23964483094734,-2.53627999497769,29.5049271198867));
#34800=CARTESIAN_POINT('Ctrl Pts',(5.81442340136165,0.281202199663012,29.6439471153992));
#34801=CARTESIAN_POINT('Ctrl Pts',(4.97044022116119,3.03006900503279,29.7829671109117));
#34802=CARTESIAN_POINT('Ctrl Pts',(2.91363334672317,5.03957685607234,29.9219871064243));
#34803=CARTESIAN_POINT('Ctrl Pts',(0.145878668470538,5.81939116931338,30.0610071019367));
#34804=CARTESIAN_POINT('Ctrl Pts',(-2.65747146968753,5.17923156029867,30.2000270974493));
#34805=CARTESIAN_POINT('Ctrl Pts',(-4.81237917180638,3.27530164628564,30.3390470929618));
#34806=CARTESIAN_POINT('Ctrl Pts',(-5.79303122945065,0.57217422347277,30.4780670884743));
#34807=CARTESIAN_POINT('Ctrl Pts',(-5.36014138257237,-2.27056788628583,
30.6170870839868));
#34808=CARTESIAN_POINT('Ctrl Pts',(-3.61933791356257,-4.55927485844469,
30.7561070794994));
#34809=CARTESIAN_POINT('Ctrl Pts',(-0.995389575345323,-5.73548548605007,
30.8951270750118));
#34810=CARTESIAN_POINT('Ctrl Pts',(1.87144108481115,-5.51219579056096,31.0341470705244));
#34811=CARTESIAN_POINT('Ctrl Pts',(4.28162646023702,-3.94389008751453,31.1731670660369));
#34812=CARTESIAN_POINT('Ctrl Pts',(5.64706372688543,-1.4132464158427,31.3121870615494));
#34813=CARTESIAN_POINT('Ctrl Pts',(5.63457622508423,1.46223969687353,31.4512070570619));
#34814=CARTESIAN_POINT('Ctrl Pts',(4.24721099642181,3.98092865036174,31.5902270525745));
#34815=CARTESIAN_POINT('Ctrl Pts',(1.8234952833584,5.52824195553766,31.7292470480869));
#34816=CARTESIAN_POINT('Ctrl Pts',(-1.04516658891478,5.72662387177763,31.8682670435995));
#34817=CARTESIAN_POINT('Ctrl Pts',(-3.65880018460502,4.52766776348834,32.0072870391119));
#34818=CARTESIAN_POINT('Ctrl Pts',(-5.37965982891017,2.22392767252164,32.1463070346245));
#34819=CARTESIAN_POINT('Ctrl Pts',(-5.78784320770817,-0.622467003449729,
32.285327030137));
#34820=CARTESIAN_POINT('Ctrl Pts',(-4.7837505971572,-3.31697518706355,32.4243470256496));
#34821=CARTESIAN_POINT('Ctrl Pts',(-2.61238792331202,-5.2021172137439,32.563367021162));
#34822=CARTESIAN_POINT('Ctrl Pts',(0.19641647218261,-5.81790466893816,32.7023870166746));
#34823=CARTESIAN_POINT('Ctrl Pts',(2.95729381478017,-5.01408091881854,32.8414070121871));
#34824=CARTESIAN_POINT('Ctrl Pts',(4.99656988067041,-2.98678482569044,32.9804270076996));
#34825=CARTESIAN_POINT('Ctrl Pts',(5.81664642467701,-0.230691433931826,
33.1194470032122));
#34826=CARTESIAN_POINT('Ctrl Pts',(5.21741878415356,2.58169235157071,33.2584669987246));
#34827=CARTESIAN_POINT('Ctrl Pts',(3.34510287727474,4.76412435898198,33.3974869942372));
#34828=CARTESIAN_POINT('Ctrl Pts',(0.656557451741129,5.78407524846973,33.5365069897497));
#34829=CARTESIAN_POINT('Ctrl Pts',(-2.1921927843664,5.39266955816591,33.6755269852622));
#34830=CARTESIAN_POINT('Ctrl Pts',(-4.5060319798187,3.68541313345579,33.8145469807748));
#34831=CARTESIAN_POINT('Ctrl Pts',(-5.72036648173308,1.07888900358752,33.9535669762872));
#34832=CARTESIAN_POINT('Ctrl Pts',(-5.53888980796299,-1.79089191819071,
34.0925869717998));
#34833=CARTESIAN_POINT('Ctrl Pts',(-4.00588359154434,-4.22368213983876,
34.2316069673123));
#34834=CARTESIAN_POINT('Ctrl Pts',(-1.49541253901362,-5.62586308983412,
34.3706269628248));
#34835=CARTESIAN_POINT('Ctrl Pts',(1.37995008836278,-5.65529238156834,34.5096469583373));
#34836=CARTESIAN_POINT('Ctrl Pts',(3.91859482163678,-4.30478905304764,34.6486669538498));
#34837=CARTESIAN_POINT('Ctrl Pts',(5.5010738157949,-1.90388577403503,34.7876869493624));
#34838=CARTESIAN_POINT('Ctrl Pts',(5.74125064542016,0.961579530699287,34.9267069448748));
#34839=CARTESIAN_POINT('Ctrl Pts',(4.58052041098353,3.59241241117446,35.0657269403874));
#34840=CARTESIAN_POINT('Ctrl Pts',(2.30210976209836,5.34667044155973,35.2047469358999));
#34841=CARTESIAN_POINT('Ctrl Pts',(-0.53803247231554,5.79630185774787,35.3437669314124));
#34842=CARTESIAN_POINT('Ctrl Pts',(-3.24689085627389,4.83159331223588,35.482786926925));
#34843=CARTESIAN_POINT('Ctrl Pts',(-5.1634841715715,2.68794073173646,35.6218069224374));
#34844=CARTESIAN_POINT('Ctrl Pts',(-5.82014965966356,-0.111589007143574,
35.76082691795));
#34845=CARTESIAN_POINT('Ctrl Pts',(-5.05665614831808,-2.88389021376926,
35.8998469134625));
#34846=CARTESIAN_POINT('Ctrl Pts',(-3.05930162720085,-4.95250115812238,
36.038866908975));
#34847=CARTESIAN_POINT('Ctrl Pts',(-0.315455178569425,-5.81266567056034,
36.1778869044875));
#34848=CARTESIAN_POINT('Ctrl Pts',(2.50536463620572,-5.25449733152917,36.3169069));
#34849=CARTESIAN_POINT('Ctrl Pts',(4.7148571925705,-3.41419328993885,36.4559268955126));
#34850=CARTESIAN_POINT('Ctrl Pts',(5.77389017922739,-0.740801164698446,
36.594946891025));
#34851=CARTESIAN_POINT('Ctrl Pts',(5.42405181733073,2.11335185198976,36.7339668865376));
#34852=CARTESIAN_POINT('Ctrl Pts',(3.750705220726,4.45183159099891,36.8729868820501));
#34853=CARTESIAN_POINT('Ctrl Pts',(1.16215917308872,5.70403192696209,37.0120068775626));
#34854=CARTESIAN_POINT('Ctrl Pts',(-1.7099621956231,5.5644068378343,37.1510268730751));
#34855=CARTESIAN_POINT('Ctrl Pts',(-4.16484030723409,4.06702586451518,37.2900468685877));
#34856=CARTESIAN_POINT('Ctrl Pts',(-5.60346698384665,1.57726089418894,37.4290668641001));
#34857=CARTESIAN_POINT('Ctrl Pts',(-5.67480681553278,-1.29736724707385,
37.5680868596127));
#34858=CARTESIAN_POINT('Ctrl Pts',(-4.36145236263682,-3.85542831029796,
37.7071068551252));
#34859=CARTESIAN_POINT('Ctrl Pts',(-1.98387169811197,-5.47273672423838,
37.8461268506377));
#34860=CARTESIAN_POINT('Ctrl Pts',(0.877788141443237,-5.75465743082409,
37.9851468461503));
#34861=CARTESIAN_POINT('Ctrl Pts',(3.52526126732858,-4.63239971985041,38.1241668416627));
#34862=CARTESIAN_POINT('Ctrl Pts',(5.31254491237248,-2.37980266438677,38.2631868371753));
#34863=CARTESIAN_POINT('Ctrl Pts',(5.80352882143023,0.453483611860533,38.4022068326878));
#34864=CARTESIAN_POINT('Ctrl Pts',(4.87840933689825,3.17611657674293,38.5412268282003));
#34865=CARTESIAN_POINT('Ctrl Pts',(2.76292236564143,5.12375391376631,38.6802468237129));
#34866=CARTESIAN_POINT('Ctrl Pts',(-0.026737829975367,5.82115789648808,
38.8192668192253));
#34867=CARTESIAN_POINT('Ctrl Pts',(-2.80987379991321,5.09815686262776,38.9582868147379));
#34868=CARTESIAN_POINT('Ctrl Pts',(-4.90738005282049,3.1311683417818,39.0973068102503));
#34869=CARTESIAN_POINT('Ctrl Pts',(-5.80744975285464,0.400151890493876,
39.2363268057629));
#34870=CARTESIAN_POINT('Ctrl Pts',(-5.29045932341185,-2.42850454286624,
39.3753468012754));
#34871=CARTESIAN_POINT('Ctrl Pts',(-3.48255820289654,-4.66458814160855,
39.514366796788));
#34872=CARTESIAN_POINT('Ctrl Pts',(-0.824887460959776,-5.76247818600198,
39.6533867923004));
#34873=CARTESIAN_POINT('Ctrl Pts',(2.03406184247587,-5.4542814914873,39.792406787813));
#34874=CARTESIAN_POINT('Ctrl Pts',(4.39668520930807,-3.81520030111772,39.9314267833255));
#34875=CARTESIAN_POINT('Ctrl Pts',(5.68648529275177,-1.24518238933703,40.0704467788382));
#34876=CARTESIAN_POINT('Ctrl Pts',(5.5887414579283,1.62866911428645,40.2094667743506));
#34877=CARTESIAN_POINT('Ctrl Pts',(4.12730391398715,4.10511346603033,40.3484867698631));
#34878=CARTESIAN_POINT('Ctrl Pts',(1.65877408898573,5.5798801679881,40.4875067653756));
#34879=CARTESIAN_POINT('Ctrl Pts',(-1.21450872146438,5.69311538025396,40.6265267608882));
#34880=CARTESIAN_POINT('Ctrl Pts',(-3.79144253892607,4.41718888450776,40.7655467564006));
#34881=CARTESIAN_POINT('Ctrl Pts',(-5.44323670236427,2.06343605896375,40.9045667519131));
#34882=CARTESIAN_POINT('Ctrl Pts',(-5.76684137911178,-0.793810226415255,
41.0435867474256));
#34883=CARTESIAN_POINT('Ctrl Pts',(-4.68329466598454,-3.45736102236341,
41.1826067429381));
#34884=CARTESIAN_POINT('Ctrl Pts',(-2.45698987001788,-5.27729049285965,
41.3216267384507));
#34885=CARTESIAN_POINT('Ctrl Pts',(0.368838388311899,-5.80952256306013,
41.4606467339632));
#34886=CARTESIAN_POINT('Ctrl Pts',(3.10466738766565,-4.92418872296366,41.5996667294757));
#34887=CARTESIAN_POINT('Ctrl Pts',(5.08293488281772,-2.83731689178915,41.7386867249883));
#34888=CARTESIAN_POINT('Ctrl Pts',(5.8209291651662,-0.0581190288535307,
41.8777067205007));
#34889=CARTESIAN_POINT('Ctrl Pts',(5.13857424304467,2.73526030134519,42.0167267160134));
#34890=CARTESIAN_POINT('Ctrl Pts',(3.20236969810097,4.86121615278336,42.1557467115258));
#34891=CARTESIAN_POINT('Ctrl Pts',(0.484763572059907,5.80099977991734,42.2947667070383));
#34892=CARTESIAN_POINT('Ctrl Pts',(-2.35112840395363,5.32529711805075,42.4337867025508));
#34893=CARTESIAN_POINT('Ctrl Pts',(-4.61332788802856,3.5501830889315,42.5728066980634));
#34894=CARTESIAN_POINT('Ctrl Pts',(-5.74984169378732,0.90879847259015,42.7118266935758));
#34895=CARTESIAN_POINT('Ctrl Pts',(-5.48335215697474,-1.95433960457174,
42.8508466890884));
#34896=CARTESIAN_POINT('Ctrl Pts',(-3.87888466973552,-4.34060455308798,
42.9898666846009));
#34897=CARTESIAN_POINT('Ctrl Pts',(-1.32794101029701,-5.66773030767773,
43.1288866801135));
#34898=CARTESIAN_POINT('Ctrl Pts',(1.54702994857086,-5.61188849725491,43.2679066756258));
#34899=CARTESIAN_POINT('Ctrl Pts',(4.04451430789495,-4.18670493116369,43.4069266711385));
#34900=CARTESIAN_POINT('Ctrl Pts',(5.55510765434376,-1.73993480224076,43.5459466666509));
#34901=CARTESIAN_POINT('Ctrl Pts',(5.71021418524961,1.13139211857394,43.6849666621635));
#34902=CARTESIAN_POINT('Ctrl Pts',(4.47198677491675,3.72665110419086,43.8239866576759));
#34903=CARTESIAN_POINT('Ctrl Pts',(2.1425619495451,5.41258001878576,43.9630066531885));
#34904=CARTESIAN_POINT('Ctrl Pts',(-0.709663630519674,5.77779990125263,
44.102026648701));
#34905=CARTESIAN_POINT('Ctrl Pts',(-3.3887261047556,4.73319443445388,44.2410466442136));
#34906=CARTESIAN_POINT('Ctrl Pts',(-5.24091467441638,2.53365497708039,44.3800666397261));
#34907=CARTESIAN_POINT('Ctrl Pts',(-5.81428180899623,-0.284114788373957,
44.5190866352387));
#34908=CARTESIAN_POINT('Ctrl Pts',(-4.96892174253198,-3.03255847165228,
44.658106630751));
#34909=CARTESIAN_POINT('Ctrl Pts',(-2.91110850169949,-5.04103575257413,
44.7971266262637));
#34910=CARTESIAN_POINT('Ctrl Pts',(-0.142963537667334,-5.81946351430219,
44.9361466217762));
#34911=CARTESIAN_POINT('Ctrl Pts',(2.66006557307581,-5.17789970106932,45.0751666172887));
#34912=CARTESIAN_POINT('Ctrl Pts',(4.81401926761876,-3.27289056621134,45.2141866128011));
#34913=CARTESIAN_POINT('Ctrl Pts',(5.79331712233613,-0.569272243690995,
45.3532066083137));
#34914=CARTESIAN_POINT('Ctrl Pts',(5.35900331258278,2.27325266152679,45.4922266038261));
#34915=CARTESIAN_POINT('Ctrl Pts',(3.61705357807721,4.56108732438807,45.6312465993388));
#34916=CARTESIAN_POINT('Ctrl Pts',(0.992516368906552,5.73598338777858,45.7702665948512));
#34917=CARTESIAN_POINT('Ctrl Pts',(-1.87420207887986,5.51125763641381,45.9092865903637));
#34918=CARTESIAN_POINT('Ctrl Pts',(-4.28360153919141,3.94174479396065,46.0483065858762));
#34919=CARTESIAN_POINT('Ctrl Pts',(-5.64777095711903,1.41041745015005,46.1873265813888));
#34920=CARTESIAN_POINT('Ctrl Pts',(-5.63384303711158,-1.46506204639129,
46.3263465769013));
#34921=CARTESIAN_POINT('Ctrl Pts',(-4.24521629374547,-3.98305570989048,
46.4653665724138));
#34922=CARTESIAN_POINT('Ctrl Pts',(-1.82072578743378,-5.52915470689165,
46.6043865679263));
#34923=CARTESIAN_POINT('Ctrl Pts',(1.04803509977905,-5.72609959722744,46.7434065634389));
#34924=CARTESIAN_POINT('Ctrl Pts',(3.66106777494364,-4.52583438933708,46.8824265589513));
#34925=CARTESIAN_POINT('Ctrl Pts',(5.38077318598422,-2.22123255644752,47.0214465544639));
#34926=CARTESIAN_POINT('Ctrl Pts',(5.78753067235475,0.625366235410245,47.1604665499763));
#34927=CARTESIAN_POINT('Ctrl Pts',(4.78208841449392,3.31937109732865,47.299486545489));
#34928=CARTESIAN_POINT('Ctrl Pts',(2.60978170886072,5.20342519017945,47.4385065410014));
#34929=CARTESIAN_POINT('Ctrl Pts',(-0.199330843227342,5.81780554118826,
47.5775265365139));
#34930=CARTESIAN_POINT('Ctrl Pts',(-2.95980509719784,5.01259890319342,47.7165465320265));
#34931=CARTESIAN_POINT('Ctrl Pts',(-4.99806553239269,2.98428148935706,47.855566527539));
#34932=CARTESIAN_POINT('Ctrl Pts',(-5.81676104845808,0.227777717483519,
47.9945865230515));
#34933=CARTESIAN_POINT('Ctrl Pts',(-5.21612528403191,-2.58430569135105,
48.1336065185641));
#34934=CARTESIAN_POINT('Ctrl Pts',(-3.34271517260787,-4.76579923569095,
48.2726265140765));
#34935=CARTESIAN_POINT('Ctrl Pts',(-0.653661486064455,-5.78440378494888,
48.4116465095892));
#34936=CARTESIAN_POINT('Ctrl Pts',(2.19489686646158,-5.39157001791135,48.5506665051015));
#34937=CARTESIAN_POINT('Ctrl Pts',(4.50787169081764,-3.68315687906655,48.6896865006141));
#34938=CARTESIAN_POINT('Ctrl Pts',(5.7209176522647,-1.07602059177106,48.8287064961267));
#34939=CARTESIAN_POINT('Ctrl Pts',(5.53796966980217,1.79366089053333,48.9677264916392));
#34940=CARTESIAN_POINT('Ctrl Pts',(4.00381092406488,4.22569882818473,49.1067464871517));
#34941=CARTESIAN_POINT('Ctrl Pts',(1.49250882932127,5.626590889655,49.2457664826643));
#34942=CARTESIAN_POINT('Ctrl Pts',(-1.3826137177127,5.65464066082273,49.3847864781767));
#34943=CARTESIAN_POINT('Ctrl Pts',(-3.92110725836691,4.30274642744152,49.5238064736894));
#34944=CARTESIAN_POINT('Ctrl Pts',(-4.97439857514882,2.70177434217856,49.6164864706976));
#34945=CARTESIAN_POINT('Ctrl Pts',(-5.27781647799386,1.82365787836681,49.6628264692018));
#34946=CARTESIAN_POINT('Ctrl Pts',(3.05002998429121,-4.27421589951819,-0.19205317402687));
#34947=CARTESIAN_POINT('Ctrl Pts',(3.76125447956637,-3.76669573907992,-0.145707626209139));
#34948=CARTESIAN_POINT('Ctrl Pts',(4.92466409230247,-2.39035204390054,-0.0530220798872355));
#34949=CARTESIAN_POINT('Ctrl Pts',(5.46779549246023,0.259111396808819,0.0860034649388399));
#34950=CARTESIAN_POINT('Ctrl Pts',(4.67676629503674,2.8445323183143,0.225023460451358));
#34951=CARTESIAN_POINT('Ctrl Pts',(2.7445538350136,4.7362167530772,0.364043455963875));
#34952=CARTESIAN_POINT('Ctrl Pts',(0.142659132105948,5.47205170154488,0.503063451476392));
#34953=CARTESIAN_POINT('Ctrl Pts',(-2.49404997803322,4.87275717303697,0.64208344698891));
#34954=CARTESIAN_POINT('Ctrl Pts',(-4.5221903674749,3.08442767596202,0.781103442501426));
#34955=CARTESIAN_POINT('Ctrl Pts',(-5.44688448789985,0.543499211903274,
0.920123438013945));
#34956=CARTESIAN_POINT('Ctrl Pts',(-5.04249842617391,-2.13005927158998,
1.05914343352647));
#34957=CARTESIAN_POINT('Ctrl Pts',(-3.40770625431275,-4.28386147173102,
1.19816342903898));
#34958=CARTESIAN_POINT('Ctrl Pts',(-0.941408722948332,-5.39237341802913,
1.3371834245515));
#34959=CARTESIAN_POINT('Ctrl Pts',(1.7545993264326,-5.18510524360307,1.47620342006402));
#34960=CARTESIAN_POINT('Ctrl Pts',(4.02247237495026,-3.71263438622792,1.61522341557653));
#34961=CARTESIAN_POINT('Ctrl Pts',(5.30883278161673,-1.33425320709353,1.75424341108905));
#34962=CARTESIAN_POINT('Ctrl Pts',(5.29979925031378,1.36969527211531,1.89326340660157));
#34963=CARTESIAN_POINT('Ctrl Pts',(3.99757601195593,3.73942822069339,2.03228340211409));
#34964=CARTESIAN_POINT('Ctrl Pts',(1.71991505043604,5.19671333043287,2.17130339762661));
#34965=CARTESIAN_POINT('Ctrl Pts',(-0.977417738888497,5.38596248543875,
2.31032339313912));
#34966=CARTESIAN_POINT('Ctrl Pts',(-3.43625346479038,4.26099746548253,2.44934338865164));
#34967=CARTESIAN_POINT('Ctrl Pts',(-5.05661826374546,2.09631796986123,2.58836338416416));
#34968=CARTESIAN_POINT('Ctrl Pts',(-5.44313129684181,-0.57987841587087,
2.72738337967668));
#34969=CARTESIAN_POINT('Ctrl Pts',(-4.50148056306639,-3.11458023342574,
2.86640337518919));
#34970=CARTESIAN_POINT('Ctrl Pts',(-2.46143571461011,-4.8893017411088,3.00542337070171));
#34971=CARTESIAN_POINT('Ctrl Pts',(0.179217414714102,-5.47099793539511,
3.14444336621423));
#34972=CARTESIAN_POINT('Ctrl Pts',(2.77614018671673,-4.71773069977217,3.28346336172674));
#34973=CARTESIAN_POINT('Ctrl Pts',(4.69566448953035,-2.81330273756845,3.42248335723926));
#34974=CARTESIAN_POINT('Ctrl Pts',(5.46941238227303,-0.2224083725902,3.56150335275178));
#34975=CARTESIAN_POINT('Ctrl Pts',(4.90858373136372,2.42275525874201,3.7005233482643));
#34976=CARTESIAN_POINT('Ctrl Pts',(3.15002482123177,4.47674892272896,3.83954334377682));
#34977=CARTESIAN_POINT('Ctrl Pts',(0.622836862034194,5.43838317286077,3.97856333928933));
#34978=CARTESIAN_POINT('Ctrl Pts',(-2.05632783771493,5.0730122329227,4.11758333480185));
#34979=CARTESIAN_POINT('Ctrl Pts',(-4.23373353549831,3.46978927918545,4.25660333031437));
#34980=CARTESIAN_POINT('Ctrl Pts',(-5.37807734772074,1.01991241461394,4.39562332582688));
#34981=CARTESIAN_POINT('Ctrl Pts',(-5.2101310313972,-1.67883052367498,4.5346433213394));
#34982=CARTESIAN_POINT('Ctrl Pts',(-3.77087471358557,-3.9679265600553,4.67366331685192));
#34983=CARTESIAN_POINT('Ctrl Pts',(-1.41149744126235,-5.28881955306291,
4.81268331236443));
#34984=CARTESIAN_POINT('Ctrl Pts',(1.29229550954153,-5.3192019709323,4.95170330787695));
#34985=CARTESIAN_POINT('Ctrl Pts',(3.68075892328426,-4.05166028193557,5.09072330338947));
#34986=CARTESIAN_POINT('Ctrl Pts',(5.17109029312276,-1.79548391023775,5.22974329890198));
#34987=CARTESIAN_POINT('Ctrl Pts',(5.39963788657859,0.898803641167593,5.36876329441451));
#34988=CARTESIAN_POINT('Ctrl Pts',(4.31063442263225,3.37377654357382,5.50778328992702));
#34989=CARTESIAN_POINT('Ctrl Pts',(2.16980469534884,5.0255233434532,5.64680328543954));
#34990=CARTESIAN_POINT('Ctrl Pts',(-0.500473215454255,5.45100576519269,
5.78582328095206));
#34991=CARTESIAN_POINT('Ctrl Pts',(-3.0486320086287,4.54640299220334,5.92484327646457));
#34992=CARTESIAN_POINT('Ctrl Pts',(-4.85290233910033,2.53244470397788,6.06386327197709));
#34993=CARTESIAN_POINT('Ctrl Pts',(-5.47302907649065,-0.099448576857391,
6.20288326748962));
#34994=CARTESIAN_POINT('Ctrl Pts',(-4.75769677044274,-2.70707567904368,
6.34190326300212));
#34995=CARTESIAN_POINT('Ctrl Pts',(-2.88145172499117,-4.65415655603638,
6.48092325851464));
#34996=CARTESIAN_POINT('Ctrl Pts',(-0.302111426327919,-5.46558926170208,
6.61994325402716));
#34997=CARTESIAN_POINT('Ctrl Pts',(2.35094626553332,-4.94337829304272,6.75896324953968));
#34998=CARTESIAN_POINT('Ctrl Pts',(4.43035590855997,-3.21494693813735,6.8979832450522));
#34999=CARTESIAN_POINT('Ctrl Pts',(5.42872637181122,-0.70204506376189,7.03700324056471));
#35000=CARTESIAN_POINT('Ctrl Pts',(5.10244797494064,1.98216093054403,7.17602323607723));
#35001=CARTESIAN_POINT('Ctrl Pts',(3.53113502835836,4.1827051895934,7.31504323158974));
#35002=CARTESIAN_POINT('Ctrl Pts',(1.09819936036962,5.36263885194919,7.45406322710226));
#35003=CARTESIAN_POINT('Ctrl Pts',(-1.60270496753428,5.23404949141599,7.59308322261479));
#35004=CARTESIAN_POINT('Ctrl Pts',(-3.91253758488377,3.82831385056435,7.73210321812729));
#35005=CARTESIAN_POINT('Ctrl Pts',(-5.26768247309822,1.4884416865181,7.87112321363982));
#35006=CARTESIAN_POINT('Ctrl Pts',(-5.33747438796964,-1.21462111348319,
8.01014320915234));
#35007=CARTESIAN_POINT('Ctrl Pts',(-4.10488359284374,-3.62130749602312,
8.14916320466484));
#35008=CARTESIAN_POINT('Ctrl Pts',(-1.87067123866715,-5.14436841685882,
8.28818320017738));
#35009=CARTESIAN_POINT('Ctrl Pts',(0.819998552161644,-5.41216589416879,
8.42720319568988));
#35010=CARTESIAN_POINT('Ctrl Pts',(3.31058271092346,-4.35935538878005,8.56622319120241));
#35011=CARTESIAN_POINT('Ctrl Pts',(4.99336052359004,-2.24283034868973,8.70524318671491));
#35012=CARTESIAN_POINT('Ctrl Pts',(5.45772192092638,0.420961667364843,8.84426318222745));
#35013=CARTESIAN_POINT('Ctrl Pts',(4.59035933251229,2.98203596389586,8.98328317773994));
#35014=CARTESIAN_POINT('Ctrl Pts',(2.60291556098025,4.81547171873721,9.12230317325249));
#35015=CARTESIAN_POINT('Ctrl Pts',(-0.0196586066515966,5.47389722507973,
9.26132316876499));
#35016=CARTESIAN_POINT('Ctrl Pts',(-2.6374359307682,4.79665185339147,9.40034316427751));
#35017=CARTESIAN_POINT('Ctrl Pts',(-4.61165963658542,2.94898841771886,9.53936315979002));
#35018=CARTESIAN_POINT('Ctrl Pts',(-5.46060472961549,0.381750282844645,
9.67838315530255));
#35019=CARTESIAN_POINT('Ctrl Pts',(-4.97712241053276,-2.27863770751815,
9.81740315081505));
#35020=CARTESIAN_POINT('Ctrl Pts',(-3.27918589423115,-4.38302146499723,
9.95642314632758));
#35021=CARTESIAN_POINT('Ctrl Pts',(-0.781104084279084,-5.41791599243413,
10.0954431418401));
#35022=CARTESIAN_POINT('Ctrl Pts',(1.90757282367781,-5.13079947122442,10.2344631373526));
#35023=CARTESIAN_POINT('Ctrl Pts',(4.1307880388876,-3.59173042826634,10.3734831328651));
#35024=CARTESIAN_POINT('Ctrl Pts',(5.34606082113004,-1.1762529440258,10.5125031283776));
#35025=CARTESIAN_POINT('Ctrl Pts',(5.25685574100989,1.52623884427124,10.6515231238902));
#35026=CARTESIAN_POINT('Ctrl Pts',(3.88493948920281,3.8563172142322,10.7905431194027));
#35027=CARTESIAN_POINT('Ctrl Pts',(1.56506964505107,5.24542603586122,10.9295631149152));
#35028=CARTESIAN_POINT('Ctrl Pts',(-1.13668861626112,5.3546126172874,11.0685831104277));
#35029=CARTESIAN_POINT('Ctrl Pts',(-3.56108655827961,4.15723463566725,11.2076031059403));
#35030=CARTESIAN_POINT('Ctrl Pts',(-5.11655338696839,1.94546105842631,11.3466231014528));
#35031=CARTESIAN_POINT('Ctrl Pts',(-5.42354384245238,-0.74101921739443,
11.4856430969653));
#35032=CARTESIAN_POINT('Ctrl Pts',(-4.40715001280646,-3.24668539531798,
11.6246630924778));
#35033=CARTESIAN_POINT('Ctrl Pts',(-2.31537941133364,-4.96013663855375,
11.7636830879903));
#35034=CARTESIAN_POINT('Ctrl Pts',(0.341360666939199,-5.4632783369162,11.9027030835028));
#35035=CARTESIAN_POINT('Ctrl Pts',(2.91480625081657,-4.63334024346925,12.0417230790154));
#35036=CARTESIAN_POINT('Ctrl Pts',(4.77701783371922,-2.67283331090427,12.1807430745279));
#35037=CARTESIAN_POINT('Ctrl Pts',(5.47360219675033,-0.060135540913871,
12.3197630700404));
#35038=CARTESIAN_POINT('Ctrl Pts',(4.83458767081651,2.56723574000129,12.4587830655529));
#35039=CARTESIAN_POINT('Ctrl Pts',(3.01589846454521,4.56818276156996,12.5978030610654));
#35040=CARTESIAN_POINT('Ctrl Pts',(0.461308019256385,5.45445984520197,12.7368230565779));
#35041=CARTESIAN_POINT('Ctrl Pts',(-2.20584494991392,5.00980891337088,12.8758430520905));
#35042=CARTESIAN_POINT('Ctrl Pts',(-4.33475565038537,3.34272803904282,13.014863047603));
#35043=CARTESIAN_POINT('Ctrl Pts',(-5.40595433188213,0.85999712392298,13.1538830431155));
#35044=CARTESIAN_POINT('Ctrl Pts',(-5.15806069721761,-1.83257936673147,
13.292903038628));
#35045=CARTESIAN_POINT('Ctrl Pts',(-3.65156260267703,-4.07799311552651,
13.4319230341405));
#35046=CARTESIAN_POINT('Ctrl Pts',(-1.25405657957035,-5.32834677801541,
13.570943029653));
#35047=CARTESIAN_POINT('Ctrl Pts',(1.44944840257059,-5.27854493396018,13.7099630251656));
#35048=CARTESIAN_POINT('Ctrl Pts',(3.79927739465977,-3.94073959682421,13.8489830206781));
#35049=CARTESIAN_POINT('Ctrl Pts',(5.22205497073815,-1.64136503378741,13.9880030161906));
#35050=CARTESIAN_POINT('Ctrl Pts',(5.37061301709398,1.05851457815739,14.1270230117031));
#35051=CARTESIAN_POINT('Ctrl Pts',(4.20870228606042,3.5001089067143,14.2660430072156));
#35052=CARTESIAN_POINT('Ctrl Pts',(2.01983747703712,5.08765111401199,14.4050630027282));
#35053=CARTESIAN_POINT('Ctrl Pts',(-0.661882419595964,5.43376931366991,
14.5440829982406));
#35054=CARTESIAN_POINT('Ctrl Pts',(-3.18209817463055,4.45400813858303,14.6831029937532));
#35055=CARTESIAN_POINT('Ctrl Pts',(-4.92585874826066,2.38743646695259,14.8221229892657));
#35056=CARTESIAN_POINT('Ctrl Pts',(-5.46767383245036,-0.261687129008328,
14.9611429847782));
#35057=CARTESIAN_POINT('Ctrl Pts',(-4.67533659183668,-2.84695715538257,
15.1001629802908));
#35058=CARTESIAN_POINT('Ctrl Pts',(-2.74218309656324,-4.73754885531261,
15.2391829758032));
#35059=CARTESIAN_POINT('Ctrl Pts',(-0.139916909965175,-5.47214405419455,
15.3782029713158));
#35060=CARTESIAN_POINT('Ctrl Pts',(2.49649002394695,-4.8714961615385,15.5172229668283));
#35061=CARTESIAN_POINT('Ctrl Pts',(4.52373516961751,-3.08216764740608,15.6562429623408));
#35062=CARTESIAN_POINT('Ctrl Pts',(5.44715591422003,-0.540767729925525,
15.7952629578533));
#35063=CARTESIAN_POINT('Ctrl Pts',(5.0414308558319,2.13258346083268,15.9342829533659));
#35064=CARTESIAN_POINT('Ctrl Pts',(3.4055598701712,4.28556872097864,16.0733029488783));
#35065=CARTESIAN_POINT('Ctrl Pts',(0.938707418300856,5.39284393195074,16.2123229443909));
#35066=CARTESIAN_POINT('Ctrl Pts',(-1.75719649545506,5.18422586004037,16.3513429399034));
#35067=CARTESIAN_POINT('Ctrl Pts',(-4.02433163817825,3.71061883754025,16.4903629354159));
#35068=CARTESIAN_POINT('Ctrl Pts',(-5.30950048675456,1.33159373410367,16.6293829309284));
#35069=CARTESIAN_POINT('Ctrl Pts',(-5.29911246141731,-1.3723499600331,16.768402926441));
#35070=CARTESIAN_POINT('Ctrl Pts',(-3.99570231617316,-3.74143024685473,
16.9074229219534));
#35071=CARTESIAN_POINT('Ctrl Pts',(-1.71731164032274,-5.19757424396833,
17.046442917466));
#35072=CARTESIAN_POINT('Ctrl Pts',(0.980115610780298,-5.38547218738113,
17.1854629129785));
#35073=CARTESIAN_POINT('Ctrl Pts',(3.43838749878582,-4.25927560739433,17.324482908491));
#35074=CARTESIAN_POINT('Ctrl Pts',(5.05766773958404,-2.09378468986712,17.4635029040035));
#35075=CARTESIAN_POINT('Ctrl Pts',(5.44284013495777,0.582604974956452,17.6025228995161));
#35076=CARTESIAN_POINT('Ctrl Pts',(4.49991980898261,3.11683477333606,17.7415428950285));
#35077=CARTESIAN_POINT('Ctrl Pts',(2.45898620376762,4.89053413659811,17.8805628905411));
#35078=CARTESIAN_POINT('Ctrl Pts',(-0.181957983817034,5.47090747350714,
18.0195828860536));
#35079=CARTESIAN_POINT('Ctrl Pts',(-2.77850309520129,4.71633945359194,18.1586028815661));
#35080=CARTESIAN_POINT('Ctrl Pts',(-4.697073170486,2.81095018146029,18.2976228770786));
#35081=CARTESIAN_POINT('Ctrl Pts',(-5.46952310726072,0.219668547343855,
18.4366428725912));
#35082=CARTESIAN_POINT('Ctrl Pts',(-4.90736948268007,-2.42521381573074,
18.5756628681037));
#35083=CARTESIAN_POINT('Ctrl Pts',(-3.14778188441772,-4.47832630562831,
18.7146828636162));
#35084=CARTESIAN_POINT('Ctrl Pts',(-0.620112530044538,-5.43869448871995,
18.8537028591287));
#35085=CARTESIAN_POINT('Ctrl Pts',(2.05886880798953,-5.0719815184047,18.9927228546412));
#35086=CARTESIAN_POINT('Ctrl Pts',(4.23547112876366,-3.46766803615348,19.1317428501537));
#35087=CARTESIAN_POINT('Ctrl Pts',(5.3785875785371,-1.01721824185249,19.2707628456663));
#35088=CARTESIAN_POINT('Ctrl Pts',(5.20928939972103,1.68144022834744,19.4097828411788));
#35089=CARTESIAN_POINT('Ctrl Pts',(3.76888658368916,3.96981500964954,19.5488028366913));
#35090=CARTESIAN_POINT('Ctrl Pts',(1.40884793135217,5.28952595209399,19.6878228322038));
#35091=CARTESIAN_POINT('Ctrl Pts',(-1.29495989970804,5.31855395288035,19.8268428277163));
#35092=CARTESIAN_POINT('Ctrl Pts',(-3.68278806305859,4.04981596793535,19.9658628232288));
#35093=CARTESIAN_POINT('Ctrl Pts',(-5.17198905758884,1.79289332636729,20.1048828187414));
#35094=CARTESIAN_POINT('Ctrl Pts',(-5.39918697064639,-0.901508373534651,
20.2439028142538));
#35095=CARTESIAN_POINT('Ctrl Pts',(-4.3089438530806,-3.37593544999751,20.3829228097664));
#35096=CARTESIAN_POINT('Ctrl Pts',(-2.16728698348817,-5.02660963500785,
20.5219428052789));
#35097=CARTESIAN_POINT('Ctrl Pts',(0.503203729552668,-5.45075437880991,
20.6609628007914));
#35098=CARTESIAN_POINT('Ctrl Pts',(3.05090905959427,-4.54487526799544,20.7999827963039));
#35099=CARTESIAN_POINT('Ctrl Pts',(4.85417030987677,-2.53001341780274,20.9390027918165));
#35100=CARTESIAN_POINT('Ctrl Pts',(5.47297857295331,0.102190173426562,21.0780227873289));
#35101=CARTESIAN_POINT('Ctrl Pts',(4.75634011582337,2.70945861643248,21.2170427828415));
#35102=CARTESIAN_POINT('Ctrl Pts',(2.87911995291945,4.65559938012842,21.356062778354));
#35103=CARTESIAN_POINT('Ctrl Pts',(0.299373506209391,5.46573991288745,21.4950827738665));
#35104=CARTESIAN_POINT('Ctrl Pts',(-2.3534222612051,4.94220001133254,21.634102769379));
#35105=CARTESIAN_POINT('Ctrl Pts',(-4.43196581876828,3.2127272328694,21.7731227648916));
#35106=CARTESIAN_POINT('Ctrl Pts',(-5.42907736671412,0.69932555922365,21.9121427604041));
#35107=CARTESIAN_POINT('Ctrl Pts',(-5.10145440921986,-1.98471665539497,
22.0511627559166));
#35108=CARTESIAN_POINT('Ctrl Pts',(-3.52903933930205,-4.18447351923866,
22.1901827514291));
#35109=CARTESIAN_POINT('Ctrl Pts',(-1.09551291140435,-5.36318830104793,
22.3292027469416));
#35110=CARTESIAN_POINT('Ctrl Pts',(1.60532666325203,-5.23324599037759,22.4682227424542));
#35111=CARTESIAN_POINT('Ctrl Pts',(3.91445481446258,-3.82635345950707,22.6072427379667));
#35112=CARTESIAN_POINT('Ctrl Pts',(5.26842741852657,-1.48580275516922,22.7462627334792));
#35113=CARTESIAN_POINT('Ctrl Pts',(5.33686527712551,1.21729466661241,22.8852827289917));
#35114=CARTESIAN_POINT('Ctrl Pts',(4.10306905321916,3.62336330445434,23.0243027245042));
#35115=CARTESIAN_POINT('Ctrl Pts',(1.8680940311752,5.14530484832907,23.1633227200167));
#35116=CARTESIAN_POINT('Ctrl Pts',(-0.822709570081384,5.41175445256412,
23.3023427155292));
#35117=CARTESIAN_POINT('Ctrl Pts',(-3.3127660311103,4.35769646885517,23.4413627110418));
#35118=CARTESIAN_POINT('Ctrl Pts',(-4.99448339998182,2.24032873901511,23.5803827065543));
#35119=CARTESIAN_POINT('Ctrl Pts',(-5.45751036348743,-0.423695555768791,
23.7194027020668));
#35120=CARTESIAN_POINT('Ctrl Pts',(-4.58886496280194,-2.98433504230336,
23.8584226975793));
#35121=CARTESIAN_POINT('Ctrl Pts',(-2.60050301611552,-4.81677499523542,
23.9974426930919));
#35122=CARTESIAN_POINT('Ctrl Pts',(0.0224006481140536,-5.47388669069018,
24.1364626886043));
#35123=CARTESIAN_POINT('Ctrl Pts',(2.63983839069682,-4.7953300785821,24.2754826841169));
#35124=CARTESIAN_POINT('Ctrl Pts',(4.61313629722153,-2.94667792519104,24.4145026796294));
#35125=CARTESIAN_POINT('Ctrl Pts',(5.46079527498544,-0.379014849639979,
24.5535226751419));
#35126=CARTESIAN_POINT('Ctrl Pts',(4.97598034617548,2.28113061573125,24.6925426706544));
#35127=CARTESIAN_POINT('Ctrl Pts',(3.27698989218598,4.38466356041853,24.8315626661669));
#35128=CARTESIAN_POINT('Ctrl Pts',(0.778389985074074,5.41830659179484,24.9705826616795));
#35129=CARTESIAN_POINT('Ctrl Pts',(-1.91014276002585,5.12984326542945,25.109602657192));
#35130=CARTESIAN_POINT('Ctrl Pts',(-4.13258672915122,3.58966073850917,25.2486226527045));
#35131=CARTESIAN_POINT('Ctrl Pts',(-5.3466493717559,1.17357478971434,25.387642648217));
#35132=CARTESIAN_POINT('Ctrl Pts',(-5.25609054134937,-1.52887197393661,
25.5266626437296));
#35133=CARTESIAN_POINT('Ctrl Pts',(-3.88300725355842,-3.85826281639337,
25.665682639242));
#35134=CARTESIAN_POINT('Ctrl Pts',(-1.56244185302379,-5.24620936938954,
25.8047026347546));
#35135=CARTESIAN_POINT('Ctrl Pts',(1.13937076423583,-5.35404254308423,25.9437226302671));
#35136=CARTESIAN_POINT('Ctrl Pts',(3.56316859851835,-4.1554502559992,26.0827426257796));
#35137=CARTESIAN_POINT('Ctrl Pts',(5.11752728645563,-1.94289777495703,26.2217626212921));
#35138=CARTESIAN_POINT('Ctrl Pts',(5.42317196260459,0.74373594478854,26.3607826168046));
#35139=CARTESIAN_POINT('Ctrl Pts',(4.40552309502093,3.24889266532279,26.4998026123171));
#35140=CARTESIAN_POINT('Ctrl Pts',(2.31289443542522,4.96129586117681,26.6388226078297));
#35141=CARTESIAN_POINT('Ctrl Pts',(-0.344097348710505,5.46310665337603,
26.7778426033422));
#35142=CARTESIAN_POINT('Ctrl Pts',(-2.91712686812292,4.63187954580281,26.9168625988547));
#35143=CARTESIAN_POINT('Ctrl Pts',(-4.7783561389992,2.67044002000411,27.0558825943672));
#35144=CARTESIAN_POINT('Ctrl Pts',(-5.47363163374707,0.0573936372287894,
27.1949025898798));
#35145=CARTESIAN_POINT('Ctrl Pts',(-4.83330105668796,-2.56965721195845,
27.3339225853923));
#35146=CARTESIAN_POINT('Ctrl Pts',(-3.01360974252997,-4.56969294496682,
27.4729425809048));
#35147=CARTESIAN_POINT('Ctrl Pts',(-0.458575654232012,-5.45469024426655,
27.6119625764173));
#35148=CARTESIAN_POINT('Ctrl Pts',(2.20835424093734,-5.00870330904966,27.7509825719298));
#35149=CARTESIAN_POINT('Ctrl Pts',(4.33642958208229,-3.34055620686025,27.8900025674423));
#35150=CARTESIAN_POINT('Ctrl Pts',(5.40638445270014,-0.85728900678427,28.0290225629549));
#35151=CARTESIAN_POINT('Ctrl Pts',(5.15714205453761,1.83516296847739,28.1680425584673));
#35152=CARTESIAN_POINT('Ctrl Pts',(3.64951935201825,4.07982178419541,28.3070625539799));
#35153=CARTESIAN_POINT('Ctrl Pts',(1.25138728900764,5.32897430510424,28.4460825494924));
#35154=CARTESIAN_POINT('Ctrl Pts',(-1.45209240665622,5.27781819827875,28.5851025450049));
#35155=CARTESIAN_POINT('Ctrl Pts',(-3.80125095597222,3.93883592718345,28.7241225405174));
#35156=CARTESIAN_POINT('Ctrl Pts',(-5.22287652591183,1.63874893947494,28.86314253603));
#35157=CARTESIAN_POINT('Ctrl Pts',(-5.37008210066978,-1.06120475103391,
29.0021625315424));
#35158=CARTESIAN_POINT('Ctrl Pts',(-4.20694844552114,-3.50221673633691,
29.141182527055));
#35159=CARTESIAN_POINT('Ctrl Pts',(-2.01728866227594,-5.08866227456726,
29.2802025225675));
#35160=CARTESIAN_POINT('Ctrl Pts',(0.664604279172973,-5.43343707460167,
29.41922251808));
#35161=CARTESIAN_POINT('Ctrl Pts',(3.18432892541915,-4.45241356864901,29.5582425135925));
#35162=CARTESIAN_POINT('Ctrl Pts',(4.92705407078572,-2.38496865285581,29.6972625091051));
#35163=CARTESIAN_POINT('Ctrl Pts',(5.4675420592909,0.264426022615144,29.8362825046176));
#35164=CARTESIAN_POINT('Ctrl Pts',(4.67390987660545,2.84929881846764,29.9753025001301));
#35165=CARTESIAN_POINT('Ctrl Pts',(2.73980956819053,4.73892190499091,30.1143224956426));
#35166=CARTESIAN_POINT('Ctrl Pts',(0.137175726698781,5.47221345632237,30.2533424911551));
#35167=CARTESIAN_POINT('Ctrl Pts',(-2.49892999338152,4.87024498149005,30.3923624866676));
#35168=CARTESIAN_POINT('Ctrl Pts',(-4.52527855486839,3.07990118224584,30.5313824821802));
#35169=CARTESIAN_POINT('Ctrl Pts',(-5.44742611802051,0.538039013696014,
30.6704024776926));
#35170=CARTESIAN_POINT('Ctrl Pts',(-5.04036194648243,-2.13510860145403,
30.8094224732052));
#35171=CARTESIAN_POINT('Ctrl Pts',(-3.4034126693552,-4.28727413324872,30.9484424687177));
#35172=CARTESIAN_POINT('Ctrl Pts',(-0.936005858690288,-5.39331348282746,
31.0874624642302));
#35173=CARTESIAN_POINT('Ctrl Pts',(1.75979321359596,-5.18334497568246,31.2264824597427));
#35174=CARTESIAN_POINT('Ctrl Pts',(4.0261898966691,-3.7086024601608,31.3655024552553));
#35175=CARTESIAN_POINT('Ctrl Pts',(5.31016685695979,-1.32893387450125,31.5045224507678));
#35176=CARTESIAN_POINT('Ctrl Pts',(5.29842434414289,1.37500427670065,31.6435424462803));
#35177=CARTESIAN_POINT('Ctrl Pts',(3.99382761705674,3.74343134794615,31.7825624417928));
#35178=CARTESIAN_POINT('Ctrl Pts',(1.71470779963254,5.19843384621083,31.9215824373054));
#35179=CARTESIAN_POINT('Ctrl Pts',(-0.982813236909919,5.38498054155311,
32.0606024328178));
#35180=CARTESIAN_POINT('Ctrl Pts',(-3.44052066988868,4.25755267866645,32.1996224283304));
#35181=CARTESIAN_POINT('Ctrl Pts',(-5.05871594634058,2.09125088542497,32.3386424238428));
#35182=CARTESIAN_POINT('Ctrl Pts',(-5.44254760726829,-0.585331388334223,
32.4776624193555));
#35183=CARTESIAN_POINT('Ctrl Pts',(-4.49835792573859,-3.11908853088459,
32.6166824148679));
#35184=CARTESIAN_POINT('Ctrl Pts',(-2.4565360758811,-4.89176530502493,32.7557024103805));
#35185=CARTESIAN_POINT('Ctrl Pts',(0.184698507257711,-5.47081563872953,
32.8947224058929));
#35186=CARTESIAN_POINT('Ctrl Pts',(2.78086530647299,-4.71494702396602,33.0337424014054));
#35187=CARTESIAN_POINT('Ctrl Pts',(4.69848067279618,-2.80859691997837,33.172762396918));
#35188=CARTESIAN_POINT('Ctrl Pts',(5.46963245977199,-0.216928666984451,
33.3117823924305));
#35189=CARTESIAN_POINT('Ctrl Pts',(4.90615400258152,2.42767176416095,33.4508023879431));
#35190=CARTESIAN_POINT('Ctrl Pts',(3.14553815772543,4.47990256477127,33.5898223834555));
#35191=CARTESIAN_POINT('Ctrl Pts',(0.617388042448883,5.43900443983934,33.728842378968));
#35192=CARTESIAN_POINT('Ctrl Pts',(-2.06140926162863,5.07094953116503,33.8678623744806));
#35193=CARTESIAN_POINT('Ctrl Pts',(-4.237207659215,3.46554592297388,34.0068823699931));
#35194=CARTESIAN_POINT('Ctrl Pts',(-5.37909645969521,1.01452381383852,34.1459023655056));
#35195=CARTESIAN_POINT('Ctrl Pts',(-5.20844646086891,-1.68404951109316,
34.2849223610181));
#35196=CARTESIAN_POINT('Ctrl Pts',(-3.76689750805951,-3.97170246309136,
34.4239423565306));
#35197=CARTESIAN_POINT('Ctrl Pts',(-1.40619806791734,-5.29023102381516,
34.5629623520432));
#35198=CARTESIAN_POINT('Ctrl Pts',(1.29762396492809,-5.31790460023452,34.7019823475557));
#35199=CARTESIAN_POINT('Ctrl Pts',(3.68481627870462,-4.04797063770782,34.8410023430682));
#35200=CARTESIAN_POINT('Ctrl Pts',(5.17288652423882,-1.79030229260299,34.9800223385807));
#35201=CARTESIAN_POINT('Ctrl Pts',(5.39873469988693,0.90421287968471,35.1190423340932));
#35202=CARTESIAN_POINT('Ctrl Pts',(4.30725220227824,3.37809350929193,35.2580623296057));
#35203=CARTESIAN_POINT('Ctrl Pts',(2.1647687277864,5.0276946652267,35.3970823251183));
#35204=CARTESIAN_POINT('Ctrl Pts',(-0.505934117381339,5.45050162465994,
35.5361023206308));
#35205=CARTESIAN_POINT('Ctrl Pts',(-3.05318534499002,4.54334640333416,35.6751223161433));
#35206=CARTESIAN_POINT('Ctrl Pts',(-4.85543706258792,2.52758149676695,35.8141423116559));
#35207=CARTESIAN_POINT('Ctrl Pts',(-5.47292669607204,-0.10493174435301,
35.9531623071683));
#35208=CARTESIAN_POINT('Ctrl Pts',(-4.75498226768737,-2.71184087393226,
36.0921823026809));
#35209=CARTESIAN_POINT('Ctrl Pts',(-2.87678745838508,-4.65704103598298,
36.2312022981934));
#35210=CARTESIAN_POINT('Ctrl Pts',(-0.296635510968414,-5.46588919254529,
36.3702222937059));
#35211=CARTESIAN_POINT('Ctrl Pts',(2.35589766632866,-4.94102048946757,36.5092422892184));
#35212=CARTESIAN_POINT('Ctrl Pts',(4.43357461685579,-3.21050672142625,36.6482622847309));
#35213=CARTESIAN_POINT('Ctrl Pts',(5.4294269992893,-0.696605879202412,36.7872822802435));
#35214=CARTESIAN_POINT('Ctrl Pts',(5.10045956338232,1.98727188221763,36.926302275756));
#35215=CARTESIAN_POINT('Ctrl Pts',(3.52694276469771,4.18624079886686,37.0653222712684));
#35216=CARTESIAN_POINT('Ctrl Pts',(1.09282618754001,5.36373640435264,37.2043422667811));
#35217=CARTESIAN_POINT('Ctrl Pts',(-1.60794795614249,5.23244117615174,37.3433622622934));
#35218=CARTESIAN_POINT('Ctrl Pts',(-3.91637106178054,3.8243921082963,37.4823822578061));
#35219=CARTESIAN_POINT('Ctrl Pts',(-5.26917104193937,1.48316345098525,37.6214022533185));
#35220=CARTESIAN_POINT('Ctrl Pts',(-5.33625482709259,-1.21996791428387,
37.7604222488311));
#35221=CARTESIAN_POINT('Ctrl Pts',(-4.1012534840043,-3.62541820366888,37.8994422443435));
#35222=CARTESIAN_POINT('Ctrl Pts',(-1.86551635491906,-5.14623998867916,
38.0384622398561));
#35223=CARTESIAN_POINT('Ctrl Pts',(0.825420381557286,-5.41134165297858,
38.1774822353686));
#35224=CARTESIAN_POINT('Ctrl Pts',(3.31494852001907,-4.35603645544599,38.3165022308812));
#35225=CARTESIAN_POINT('Ctrl Pts',(4.9956050230993,-2.23782656717092,38.4555222263936));
#35226=CARTESIAN_POINT('Ctrl Pts',(5.45729743658602,0.426429337854175,38.5945422219062));
#35227=CARTESIAN_POINT('Ctrl Pts',(4.58736944159972,2.98663337184665,38.7335622174186));
#35228=CARTESIAN_POINT('Ctrl Pts',(2.59808981870197,4.81807706305204,38.8725822129312));
#35229=CARTESIAN_POINT('Ctrl Pts',(-0.0251426839555714,5.47387478272882,
39.0116022084437));
#35230=CARTESIAN_POINT('Ctrl Pts',(-2.6422401882063,4.79400710047229,39.1506222039563));
#35231=CARTESIAN_POINT('Ctrl Pts',(-4.61461180027545,2.94436669324823,39.2896421994687));
#35232=CARTESIAN_POINT('Ctrl Pts',(-5.46098445006866,0.376279321328379,
39.4286621949813));
#35233=CARTESIAN_POINT('Ctrl Pts',(-4.97483703318683,-2.28362295153644,
39.5676821904938));
#35234=CARTESIAN_POINT('Ctrl Pts',(-3.27479306783995,-4.38630455558871,
39.7067021860063));
#35235=CARTESIAN_POINT('Ctrl Pts',(-0.775675690546239,-5.41869583153057,
39.8457221815188));
#35236=CARTESIAN_POINT('Ctrl Pts',(1.91271221705852,-5.12888577239404,39.9847421770314));
#35237=CARTESIAN_POINT('Ctrl Pts',(4.13438438241777,-3.58759014799223,40.1237621725439));
#35238=CARTESIAN_POINT('Ctrl Pts',(5.34723658073789,-1.17089634091565,40.2627821680564));
#35239=CARTESIAN_POINT('Ctrl Pts',(5.25532402276895,1.53150471995962,40.4018021635689));
#35240=CARTESIAN_POINT('Ctrl Pts',(3.88107404354422,3.86020745039412,40.5408221590814));
#35241=CARTESIAN_POINT('Ctrl Pts',(1.55981366893021,5.24699138647753,40.679842154594));
#35242=CARTESIAN_POINT('Ctrl Pts',(-1.14205262630631,5.35347112538193,40.8188621501064));
#35243=CARTESIAN_POINT('Ctrl Pts',(-3.56524974464505,4.15366483359686,40.957882145619));
#35244=CARTESIAN_POINT('Ctrl Pts',(-5.118499901793,1.94033400395298,41.0969021411315));
#35245=CARTESIAN_POINT('Ctrl Pts',(-5.4227987219109,-0.746452485555846,
41.235922136644));
#35246=CARTESIAN_POINT('Ctrl Pts',(-4.40389507174982,-3.25109912007749,
41.3749421321565));
#35247=CARTESIAN_POINT('Ctrl Pts',(-2.31040887913814,-4.96245383885338,
41.513962127669));
#35248=CARTESIAN_POINT('Ctrl Pts',(0.346833944136911,-5.4629335989691,41.6529821231815));
#35249=CARTESIAN_POINT('Ctrl Pts',(2.91944675342964,-4.63041768585082,41.7920021186941));
#35250=CARTESIAN_POINT('Ctrl Pts',(4.77969324523812,-2.66804605900577,41.9310221142067));
#35251=CARTESIAN_POINT('Ctrl Pts',(5.47365969723602,-0.0546517191416722,
42.070042109719));
#35252=CARTESIAN_POINT('Ctrl Pts',(4.83201322973078,2.57207803910722,42.2090621052317));
#35253=CARTESIAN_POINT('Ctrl Pts',(3.01132026430437,4.57120198168282,42.3480821007441));
#35254=CARTESIAN_POINT('Ctrl Pts',(0.455843174136428,5.45491927457632,42.4871020962567));
#35255=CARTESIAN_POINT('Ctrl Pts',(-2.21086297781468,5.00759644788588,42.6261220917692));
#35256=CARTESIAN_POINT('Ctrl Pts',(-4.33810242563154,3.3383835364261,42.7651420872817));
#35257=CARTESIAN_POINT('Ctrl Pts',(-5.40681321688483,0.854580674524409,
42.9041620827942));
#35258=CARTESIAN_POINT('Ctrl Pts',(-5.156222117767,-1.83774610972284,43.0431820783068));
#35259=CARTESIAN_POINT('Ctrl Pts',(-3.64747518557922,-4.08164942910766,
43.1822020738192));
#35260=CARTESIAN_POINT('Ctrl Pts',(-1.24871768443212,-5.32960049498436,
43.3212220693318));
#35261=CARTESIAN_POINT('Ctrl Pts',(1.45473604636581,-5.27709013822532,43.4602420648443));
#35262=CARTESIAN_POINT('Ctrl Pts',(3.80322356343032,-3.93693126916376,43.5992620603568));
#35263=CARTESIAN_POINT('Ctrl Pts',(5.22369677050014,-1.63613243394826,43.7382820558693));
#35264=CARTESIAN_POINT('Ctrl Pts',(5.36954983672162,1.06389465762065,43.8773020513818));
#35265=CARTESIAN_POINT('Ctrl Pts',(4.20519354932497,3.50432368714232,44.0163220468944));
#35266=CARTESIAN_POINT('Ctrl Pts',(2.014739341313,5.08967215821577,44.1553420424069));
#35267=CARTESIAN_POINT('Ctrl Pts',(-0.667325971979708,5.43310347211171,
44.2943620379194));
#35268=CARTESIAN_POINT('Ctrl Pts',(-3.18655887715868,4.45081788146317,44.4333820334319));
#35269=CARTESIAN_POINT('Ctrl Pts',(-4.92824815695669,2.38250024029464,44.5724020289444));
#35270=CARTESIAN_POINT('Ctrl Pts',(-5.46740891415169,-0.267164849869239,
44.711422024457));
#35271=CARTESIAN_POINT('Ctrl Pts',(-4.67248198854188,-2.85163976657336,
44.8504420199694));
#35272=CARTESIAN_POINT('Ctrl Pts',(-2.73743535231266,-4.74029376552342,
44.989462015482));
#35273=CARTESIAN_POINT('Ctrl Pts',(-0.134434509010523,-5.47228148529823,
45.1284820109945));
#35274=CARTESIAN_POINT('Ctrl Pts',(2.50136933575522,-4.86899257934269,45.267502006507));
#35275=CARTESIAN_POINT('Ctrl Pts',(4.5268208045837,-3.07763394424053,45.4065220020195));
#35276=CARTESIAN_POINT('Ctrl Pts',(5.44769495488841,-0.535310162455436,
45.5455419975321));
#35277=CARTESIAN_POINT('Ctrl Pts',(5.03929177234735,2.1376332063093,45.6845619930446));
#35278=CARTESIAN_POINT('Ctrl Pts',(3.40126461451271,4.28897846970521,45.8235819885571));
#35279=CARTESIAN_POINT('Ctrl Pts',(0.93330406421049,5.39378168035181,45.9626019840697));
#35280=CARTESIAN_POINT('Ctrl Pts',(-1.76238949015754,5.18246279065678,46.101621979582));
#35281=CARTESIAN_POINT('Ctrl Pts',(-4.02804714484456,3.70658515217929,46.2406419750947));
#35282=CARTESIAN_POINT('Ctrl Pts',(-5.31083189470833,1.32627368141911,46.3796619706071));
#35283=CARTESIAN_POINT('Ctrl Pts',(-5.29773489726207,-1.37765824832074,
46.5186819661197));
#35284=CARTESIAN_POINT('Ctrl Pts',(-3.99195191588644,-3.74543150972201,
46.6577019616322));
#35285=CARTESIAN_POINT('Ctrl Pts',(-1.71210352842529,-5.19929214394272,
46.7967219571447));
#35286=CARTESIAN_POINT('Ctrl Pts',(0.985510615947398,-5.38448754457717,
46.9357419526573));
#35287=CARTESIAN_POINT('Ctrl Pts',(3.44265297857929,-4.25582868136,47.0747619481697));
#35288=CARTESIAN_POINT('Ctrl Pts',(5.05976288190223,-2.0887165566579,47.2137819436824));
#35289=CARTESIAN_POINT('Ctrl Pts',(5.44225371738929,0.588057655685179,47.3528019391947));
#35290=CARTESIAN_POINT('Ctrl Pts',(4.49679490684671,3.12134150409286,47.4918219347074));
#35291=CARTESIAN_POINT('Ctrl Pts',(2.4540853449755,4.89299524919655,47.6308419302197));
#35292=CARTESIAN_POINT('Ctrl Pts',(-0.187439010513757,5.47072242481917,
47.7698619257324));
#35293=CARTESIAN_POINT('Ctrl Pts',(-2.78322676887322,4.71355342356861,47.9088819212448));
#35294=CARTESIAN_POINT('Ctrl Pts',(-4.69988709577799,2.80624292960881,48.0479019167574));
#35295=CARTESIAN_POINT('Ctrl Pts',(-5.4697402452394,0.214188779272411,48.1869219122698));
#35296=CARTESIAN_POINT('Ctrl Pts',(-4.90493767108471,-2.43012919530724,
48.3259419077824));
#35297=CARTESIAN_POINT('Ctrl Pts',(-3.14329290057951,-4.4814775203977,48.4649619032949));
#35298=CARTESIAN_POINT('Ctrl Pts',(-0.614664846519301,-5.43931337623658,
48.6039818988075));
#35299=CARTESIAN_POINT('Ctrl Pts',(2.06395202151498,-5.06991558812843,48.7430018943199));
#35300=CARTESIAN_POINT('Ctrl Pts',(4.23893761532058,-3.46342427394386,48.8820218898325));
#35301=CARTESIAN_POINT('Ctrl Pts',(5.37961474807146,-1.01182652793978,49.0210418853449));
#35302=CARTESIAN_POINT('Ctrl Pts',(5.207581217018,1.68665328995466,49.1600618808576));
#35303=CARTESIAN_POINT('Ctrl Pts',(3.76494849337024,3.97359883829332,49.29908187637));
#35304=CARTESIAN_POINT('Ctrl Pts',(1.40346758997053,5.29091540399473,49.4381018718826));
#35305=CARTESIAN_POINT('Ctrl Pts',(-1.30012868543015,5.31729176034627,49.577121867395));
#35306=CARTESIAN_POINT('Ctrl Pts',(-3.68717882655246,4.04604987263071,49.7161418629077));
#35307=CARTESIAN_POINT('Ctrl Pts',(-4.67763208006722,2.54058981104043,49.8088218599159));
#35308=CARTESIAN_POINT('Ctrl Pts',(-4.96294844436203,1.71486069442291,49.8551618584201));
#35309=CARTESIAN_POINT('Ctrl Pts',(2.85652466090568,-4.00304363756816,0.000282215191459768));
#35310=CARTESIAN_POINT('Ctrl Pts',(3.52262641094007,-3.5277224565747,0.0466277630091907));
#35311=CARTESIAN_POINT('Ctrl Pts',(4.61222496132538,-2.23869915929206,0.139313309331095));
#35312=CARTESIAN_POINT('Ctrl Pts',(5.12089807164022,0.242672399523322,0.27833885415717));
#35313=CARTESIAN_POINT('Ctrl Pts',(4.38005472859954,2.66406453636758,0.417358849669687));
#35314=CARTESIAN_POINT('Ctrl Pts',(2.57042906242826,4.43573342696293,0.556378845182204));
#35315=CARTESIAN_POINT('Ctrl Pts',(0.133608302561927,5.12488425088266,0.695398840694722));
#35316=CARTESIAN_POINT('Ctrl Pts',(-2.33581810817467,4.56361121138943,0.83441883620724));
#35317=CARTESIAN_POINT('Ctrl Pts',(-4.23528567670923,2.8887400342109,0.973438831719756));
#35318=CARTESIAN_POINT('Ctrl Pts',(-5.10131373951276,0.509017586705921,
1.11245882723228));
#35319=CARTESIAN_POINT('Ctrl Pts',(-4.72258344381205,-1.99492033515254,
1.2514788227448));
#35320=CARTESIAN_POINT('Ctrl Pts',(-3.19150860899786,-4.01207725856082,
1.39049881825731));
#35321=CARTESIAN_POINT('Ctrl Pts',(-0.881682228353137,-5.05026105603751,
1.52951881376983));
#35322=CARTESIAN_POINT('Ctrl Pts',(1.64328097486816,-4.85614275073615,1.66853880928235));
#35323=CARTESIAN_POINT('Ctrl Pts',(3.76727166488086,-3.47709095838648,1.80755880479487));
#35324=CARTESIAN_POINT('Ctrl Pts',(4.97202055042645,-1.24960318737358,1.94657880030738));
#35325=CARTESIAN_POINT('Ctrl Pts',(4.96356014017646,1.2827966750735,2.0855987958199));
#35326=CARTESIAN_POINT('Ctrl Pts',(3.74395482038217,3.50218489166088,2.22461879133242));
#35327=CARTESIAN_POINT('Ctrl Pts',(1.61079719922008,4.86701437706966,2.36363878684493));
#35328=CARTESIAN_POINT('Ctrl Pts',(-0.915406697482164,5.04425685701712,
2.50265878235745));
#35329=CARTESIAN_POINT('Ctrl Pts',(-3.21824467754449,3.99066383048563,2.64167877786997));
#35330=CARTESIAN_POINT('Ctrl Pts',(-4.73580746601471,1.96331970795363,2.78069877338249));
#35331=CARTESIAN_POINT('Ctrl Pts',(-5.09779866494969,-0.543088757747706,
2.91971876889501));
#35332=CARTESIAN_POINT('Ctrl Pts',(-4.21588977984263,-2.91697960051942,
3.05873876440752));
#35333=CARTESIAN_POINT('Ctrl Pts',(-2.30527301575098,-4.57910613010975,
3.19775875992004));
#35334=CARTESIAN_POINT('Ctrl Pts',(0.167847190824738,-5.12389733960339,
3.33677875543256));
#35335=CARTESIAN_POINT('Ctrl Pts',(2.60001145770063,-4.41842019810271,3.47579875094507));
#35336=CARTESIAN_POINT('Ctrl Pts',(4.39775395086801,-2.63481627716698,3.61481874645759));
#35337=CARTESIAN_POINT('Ctrl Pts',(5.12241237990866,-0.208297952599817,
3.75383874197011));
#35338=CARTESIAN_POINT('Ctrl Pts',(4.59716479869933,2.26904659284643,3.89285873748263));
#35339=CARTESIAN_POINT('Ctrl Pts',(2.9501754509488,4.19272720737859,4.03187873299514));
#35340=CARTESIAN_POINT('Ctrl Pts',(0.583321759223736,5.09335177973389,4.17089872850766));
#35341=CARTESIAN_POINT('Ctrl Pts',(-1.92586669953822,4.7511613403983,4.30991872402018));
#35342=CARTESIAN_POINT('Ctrl Pts',(-3.96512962631244,3.24965285429574,4.44893871953269));
#35343=CARTESIAN_POINT('Ctrl Pts',(-5.03687198196272,0.955205351853525,
4.58795871504521));
#35344=CARTESIAN_POINT('Ctrl Pts',(-4.87958080884073,-1.57231922868232,
4.72697871055773));
#35345=CARTESIAN_POINT('Ctrl Pts',(-3.53163630128907,-3.7161864407358,4.86599870607025));
#35346=CARTESIAN_POINT('Ctrl Pts',(-1.32194675807696,-4.9532770360339,5.00501870158276));
#35347=CARTESIAN_POINT('Ctrl Pts',(1.21030744326956,-4.98173187954325,5.14403869709529));
#35348=CARTESIAN_POINT('Ctrl Pts',(3.44723779417319,-3.79460778174965,5.2830586926078));
#35349=CARTESIAN_POINT('Ctrl Pts',(4.84301696119486,-1.68157168757982,5.42207868812032));
#35350=CARTESIAN_POINT('Ctrl Pts',(5.05706463949957,0.841780172500049,5.56109868363283));
#35351=CARTESIAN_POINT('Ctrl Pts',(4.03715163320258,3.1597315261618,5.70011867914535));
#35352=CARTESIAN_POINT('Ctrl Pts',(2.03214416039696,4.70668532390425,5.83913867465787));
#35353=CARTESIAN_POINT('Ctrl Pts',(-0.468721320587276,5.10517354754156,
5.97815867017038));
#35354=CARTESIAN_POINT('Ctrl Pts',(-2.85521537805407,4.25796216185801,6.11717866568291));
#35355=CARTESIAN_POINT('Ctrl Pts',(-4.54501604246637,2.37177692893208,6.25619866119542));
#35356=CARTESIAN_POINT('Ctrl Pts',(-5.125799617502,-0.0931391867450908,
6.39521865670794));
#35357=CARTESIAN_POINT('Ctrl Pts',(-4.45585067159246,-2.5353286610142,6.53423865222046));
#35358=CARTESIAN_POINT('Ctrl Pts',(-2.69864163763604,-4.35887943610605,
6.67325864773297));
#35359=CARTESIAN_POINT('Ctrl Pts',(-0.282944346151318,-5.11883181242284,
6.81227864324549));
#35360=CARTESIAN_POINT('Ctrl Pts',(2.2017934310638,-4.62975186309325,6.95129863875801));
#35361=CARTESIAN_POINT('Ctrl Pts',(4.14927753975237,-3.0109786656497,7.09031863427053));
#35362=CARTESIAN_POINT('Ctrl Pts',(5.08430764230391,-0.657504696029762,
7.22933862978304));
#35363=CARTESIAN_POINT('Ctrl Pts',(4.77872956871716,1.8564052186846,7.36835862529557));
#35364=CARTESIAN_POINT('Ctrl Pts',(3.30710659942503,3.91733870975315,7.50737862080806));
#35365=CARTESIAN_POINT('Ctrl Pts',(1.02852548061614,5.02241296217411,7.6463986163206));
#35366=CARTESIAN_POINT('Ctrl Pts',(-1.50102336288394,4.90198179219056,7.78541861183311));
#35367=CARTESIAN_POINT('Ctrl Pts',(-3.66431154955944,3.58543128433058,7.92443860734562));
#35368=CARTESIAN_POINT('Ctrl Pts',(-4.93348097157235,1.39400937228727,8.06345860285816));
#35369=CARTESIAN_POINT('Ctrl Pts',(-4.99884502602062,-1.13756100175772,
8.20247859837064));
#35370=CARTESIAN_POINT('Ctrl Pts',(-3.8444544065131,-3.39155818808009,8.34149859388319));
#35371=CARTESIAN_POINT('Ctrl Pts',(-1.7519888503462,-4.8179904208242,8.4805185893957));
#35372=CARTESIAN_POINT('Ctrl Pts',(0.767974773435199,-5.0687978233757,8.61953858490822));
#35373=CARTESIAN_POINT('Ctrl Pts',(3.10054694689124,-4.08278155881679,8.75855858042073));
#35374=CARTESIAN_POINT('Ctrl Pts',(4.6765630337705,-2.10053679283709,8.89757857593325));
#35375=CARTESIAN_POINT('Ctrl Pts',(5.11146360520611,0.394254282848632,9.03659857144578));
#35376=CARTESIAN_POINT('Ctrl Pts',(4.29912974733827,2.79284443577551,9.17561856695828));
#35377=CARTESIAN_POINT('Ctrl Pts',(2.43777685088012,4.50996016082228,9.3146385624708));
#35378=CARTESIAN_POINT('Ctrl Pts',(-0.018411391031715,5.1266126874937,9.45365855798332));
#35379=CARTESIAN_POINT('Ctrl Pts',(-2.47010711914323,4.49233429820722,9.59267855349584));
#35380=CARTESIAN_POINT('Ctrl Pts',(-4.31907868035958,2.76189354967829,9.73169854900835));
#35381=CARTESIAN_POINT('Ctrl Pts',(-5.11416351771696,0.357530615393925,
9.87071854452088));
#35382=CARTESIAN_POINT('Ctrl Pts',(-4.66135512741105,-2.13407239873668,
10.0097385400333));
#35383=CARTESIAN_POINT('Ctrl Pts',(-3.07114206181887,-4.10494617053842,
10.1487585355459));
#35384=CARTESIAN_POINT('Ctrl Pts',(-0.731547916239905,-5.0741831138752,
10.2877785310584));
#35385=CARTESIAN_POINT('Ctrl Pts',(1.78654926062158,-4.80528233991131,10.4267985265709));
#35386=CARTESIAN_POINT('Ctrl Pts',(3.86871537749776,-3.36385760025652,10.5658185220834));
#35387=CARTESIAN_POINT('Ctrl Pts',(5.00688670370844,-1.10162705264471,10.704838517596));
#35388=CARTESIAN_POINT('Ctrl Pts',(4.92334112790964,1.42940853681676,10.8438585131084));
#35389=CARTESIAN_POINT('Ctrl Pts',(3.63846438041272,3.61165800974553,10.982878508621));
#35390=CARTESIAN_POINT('Ctrl Pts',(1.46577576618884,4.9126365660554,11.1218985041335));
#35391=CARTESIAN_POINT('Ctrl Pts',(-1.06457283398646,5.01489594189442,11.260918499646));
#35392=CARTESIAN_POINT('Ctrl Pts',(-3.33515789213115,3.89348410314547,11.3999384951585));
#35393=CARTESIAN_POINT('Ctrl Pts',(-4.79194008058653,1.82203372388092,11.538958490671));
#35394=CARTESIAN_POINT('Ctrl Pts',(-5.07945391201418,-0.694006183412673,
11.6779784861835));
#35395=CARTESIAN_POINT('Ctrl Pts',(-4.1275439129226,-3.04070351625848,11.8169984816961));
#35396=CARTESIAN_POINT('Ctrl Pts',(-2.1684830712787,-4.64544699641152,11.9560184772086));
#35397=CARTESIAN_POINT('Ctrl Pts',(0.31970346796494,-5.11666750135889,12.0950384727211));
#35398=CARTESIAN_POINT('Ctrl Pts',(2.72988002744322,-4.33938378835726,12.2340584682336));
#35399=CARTESIAN_POINT('Ctrl Pts',(4.47394593426475,-2.50325875693404,12.3730784637462));
#35400=CARTESIAN_POINT('Ctrl Pts',(5.12633637686628,-0.056320317013998,
12.5120984592586));
#35401=CARTESIAN_POINT('Ctrl Pts',(4.52786332531986,2.40436069135114,12.6511184547712));
#35402=CARTESIAN_POINT('Ctrl Pts',(2.82455857258174,4.27836014109916,12.7901384502837));
#35403=CARTESIAN_POINT('Ctrl Pts',(0.432040911094763,5.10840848778086,12.9291584457962));
#35404=CARTESIAN_POINT('Ctrl Pts',(-2.06589788625557,4.69196787611082,13.0681784413087));
#35405=CARTESIAN_POINT('Ctrl Pts',(-4.05974251994234,3.13065285502295,13.2071984368212));
#35406=CARTESIAN_POINT('Ctrl Pts',(-5.06298034586039,0.805435686024888,
13.3462184323338));
#35407=CARTESIAN_POINT('Ctrl Pts',(-4.83081401164476,-1.71631366940539,
13.4852384278463));
#35408=CARTESIAN_POINT('Ctrl Pts',(-3.41989379747425,-3.81926996177125,
13.6242584233588));
#35409=CARTESIAN_POINT('Ctrl Pts',(-1.1744945342058,-4.99029650582126,13.7632784188713));
#35410=CARTESIAN_POINT('Ctrl Pts',(1.35748996828809,-4.94365427724152,13.9022984143838));
#35411=CARTESIAN_POINT('Ctrl Pts',(3.55823700991883,-3.6907243202568,14.0413184098964));
#35412=CARTESIAN_POINT('Ctrl Pts',(4.89074824881934,-1.53723068976704,14.1803384054088));
#35413=CARTESIAN_POINT('Ctrl Pts',(5.02988121642198,0.991358449591552,14.3193584009214));
#35414=CARTESIAN_POINT('Ctrl Pts',(3.94168645307127,3.27804889111885,14.4583783964339));
#35415=CARTESIAN_POINT('Ctrl Pts',(1.89169142398414,4.76487147605431,14.5973983919464));
#35416=CARTESIAN_POINT('Ctrl Pts',(-0.619890120403223,5.08903064104723,
14.7364183874589));
#35417=CARTESIAN_POINT('Ctrl Pts',(-2.98021395070562,4.17142918373435,14.8754383829715));
#35418=CARTESIAN_POINT('Ctrl Pts',(-4.61334382383605,2.2359685574634,15.014458378484));
#35419=CARTESIAN_POINT('Ctrl Pts',(-5.12078413019695,-0.245084717626975,
15.1534783739965));
#35420=CARTESIAN_POINT('Ctrl Pts',(-4.37871573112417,-2.66633553269217,
15.292498369509));
#35421=CARTESIAN_POINT('Ctrl Pts',(-2.5682087325027,-4.4369810156443,15.4315183650215));
#35422=CARTESIAN_POINT('Ctrl Pts',(-0.131040057262327,-5.12497074433441,
15.570538360534));
#35423=CARTESIAN_POINT('Ctrl Pts',(2.33810334843862,-4.56243020318243,15.7095583560466));
#35424=CARTESIAN_POINT('Ctrl Pts',(4.23673247081922,-2.88662339032947,15.8485783515591));
#35425=CARTESIAN_POINT('Ctrl Pts',(5.1015679455308,-0.506459400173185,15.9875983470716));
#35426=CARTESIAN_POINT('Ctrl Pts',(4.72158360413018,1.99728438037758,16.1266183425841));
#35427=CARTESIAN_POINT('Ctrl Pts',(3.18949839950364,4.01367619352319,16.2656383380966));
#35428=CARTESIAN_POINT('Ctrl Pts',(0.879152304587834,5.05070171879402,16.4046583336091));
#35429=CARTESIAN_POINT('Ctrl Pts',(-1.64571336976244,4.85531915855964,16.5436783291217));
#35430=CARTESIAN_POINT('Ctrl Pts',(-3.76901296948745,3.475203283655,16.6826983246342));
#35431=CARTESIAN_POINT('Ctrl Pts',(-4.97264589385004,1.24711244130889,16.8217183201467));
#35432=CARTESIAN_POINT('Ctrl Pts',(-4.96291692373935,-1.28528293964901,
16.9607383156592));
#35433=CARTESIAN_POINT('Ctrl Pts',(-3.74219999887612,-3.50405990178573,
17.0997583111718));
#35434=CARTESIAN_POINT('Ctrl Pts',(-1.60835895919313,-4.86782067102664,
17.2387783066842));
#35435=CARTESIAN_POINT('Ctrl Pts',(0.91793340627866,-5.04379766530427,17.3777983021968));
#35436=CARTESIAN_POINT('Ctrl Pts',(3.22024332043214,-3.98905121352225,17.5168182977093));
#35437=CARTESIAN_POINT('Ctrl Pts',(4.7367903591762,-1.96094714872851,17.6558382932218));
#35438=CARTESIAN_POINT('Ctrl Pts',(5.09752597546587,0.545642333714995,17.7948582887343));
#35439=CARTESIAN_POINT('Ctrl Pts',(4.21442804584234,2.91909110397544,17.9338782842469));
#35440=CARTESIAN_POINT('Ctrl Pts',(2.30297891104881,4.58026033781438,18.0728982797593));
#35441=CARTESIAN_POINT('Ctrl Pts',(-0.170413887961411,5.12381261695634,
18.2119182752719));
#35442=CARTESIAN_POINT('Ctrl Pts',(-2.60222445442275,4.41711721778983,18.3509382707844));
#35443=CARTESIAN_POINT('Ctrl Pts',(-4.39907325982889,2.63261297602774,18.4899582662969));
#35444=CARTESIAN_POINT('Ctrl Pts',(-5.12251608008851,0.205731952126684,
18.6289782618094));
#35445=CARTESIAN_POINT('Ctrl Pts',(-4.59602758649907,-2.27134916977346,
18.767998257322));
#35446=CARTESIAN_POINT('Ctrl Pts',(-2.94807481444516,-4.19420451520013,
18.9070182528345));
#35447=CARTESIAN_POINT('Ctrl Pts',(-0.580770269057073,-5.09364334454921,
19.046038248347));
#35448=CARTESIAN_POINT('Ctrl Pts',(1.92824646114365,-4.75019601826895,19.1850582438595));
#35449=CARTESIAN_POINT('Ctrl Pts',(3.96675698015443,-3.24766619086495,19.324078239372));
#35450=CARTESIAN_POINT('Ctrl Pts',(5.03734984182548,-0.952682107500701,
19.4630982348845));
#35451=CARTESIAN_POINT('Ctrl Pts',(4.87879257342969,1.57476336391802,19.602118230397));
#35452=CARTESIAN_POINT('Ctrl Pts',(3.52977430579807,3.71795508001628,19.7411382259096));
#35453=CARTESIAN_POINT('Ctrl Pts',(1.31946534299687,4.95393861846523,19.8801582214221));
#35454=CARTESIAN_POINT('Ctrl Pts',(-1.2128027945468,4.9811249741831,20.0191782169346));
#35455=CARTESIAN_POINT('Ctrl Pts',(-3.44913819772191,3.79288047793584,20.1581982124471));
#35456=CARTESIAN_POINT('Ctrl Pts',(-4.84385870467769,1.67914546005085,20.2972182079597));
#35457=CARTESIAN_POINT('Ctrl Pts',(-5.05664233136262,-0.844313306517566,
20.4362382034721));
#35458=CARTESIAN_POINT('Ctrl Pts',(-4.03556831971381,-3.16175346347771,
20.5752581989847));
#35459=CARTESIAN_POINT('Ctrl Pts',(-2.02978618160459,-4.70770269705492,
20.7142781944972));
#35460=CARTESIAN_POINT('Ctrl Pts',(0.471278600646567,-5.10493811005225,
20.8532981900097));
#35461=CARTESIAN_POINT('Ctrl Pts',(2.85734796437971,-4.2565313621946,20.9923181855222));
#35462=CARTESIAN_POINT('Ctrl Pts',(4.5462035684287,-2.36949989265611,21.1313381810348));
#35463=CARTESIAN_POINT('Ctrl Pts',(5.12575231809818,0.0957068461616923,
21.2703581765473));
#35464=CARTESIAN_POINT('Ctrl Pts',(4.4545800882223,2.53756041593189,21.4093781720598));
#35465=CARTESIAN_POINT('Ctrl Pts',(2.69645780191612,4.36023072203488,21.5483981675723));
#35466=CARTESIAN_POINT('Ctrl Pts',(0.280380129937561,5.11897290573287,21.6874181630848));
#35467=CARTESIAN_POINT('Ctrl Pts',(-2.20411234029851,4.62864833598698,21.8264381585973));
#35468=CARTESIAN_POINT('Ctrl Pts',(-4.15078531122857,3.00889978679588,21.9654581541098));
#35469=CARTESIAN_POINT('Ctrl Pts',(-5.08463636877582,0.654957727042922,
22.1044781496224));
#35470=CARTESIAN_POINT('Ctrl Pts',(-4.77779903852622,-1.8587987987808,22.2434981451349));
#35471=CARTESIAN_POINT('Ctrl Pts',(-3.30514386873,-3.918994849944,22.3825181406474));
#35472=CARTESIAN_POINT('Ctrl Pts',(-1.02600947003294,-5.02292755216456,
22.5215381361599));
#35473=CARTESIAN_POINT('Ctrl Pts',(1.50347872840812,-4.90122926826684,22.6605581316724));
#35474=CARTESIAN_POINT('Ctrl Pts',(3.6661071429145,-3.58359526782287,22.799578127185));
#35475=CARTESIAN_POINT('Ctrl Pts',(4.93417865487318,-1.39153786462493,22.9385981226975));
#35476=CARTESIAN_POINT('Ctrl Pts',(4.99827455944932,1.140064934665,23.07761811821));
#35477=CARTESIAN_POINT('Ctrl Pts',(3.84275498807705,3.39348356832622,23.2166381137225));
#35478=CARTESIAN_POINT('Ctrl Pts',(1.74957515054818,4.8188674415754,23.355658109235));
#35479=CARTESIAN_POINT('Ctrl Pts',(-0.770513794226398,5.06841248516712,
23.4946781047475));
#35480=CARTESIAN_POINT('Ctrl Pts',(-3.10259174906973,4.08122788698396,23.6336981002601));
#35481=CARTESIAN_POINT('Ctrl Pts',(-4.67761467067925,2.09819389464779,23.7727180957726));
#35482=CARTESIAN_POINT('Ctrl Pts',(-5.11126546976328,-0.39681472313488,
23.9117380912851));
#35483=CARTESIAN_POINT('Ctrl Pts',(-4.29773018603819,-2.79499765203967,
24.0507580867976));
#35484=CARTESIAN_POINT('Ctrl Pts',(-2.43551736689566,-4.51118075257917,
24.1897780823101));
#35485=CARTESIAN_POINT('Ctrl Pts',(0.0209794671159091,-5.12660282144528,
24.3287980778226));
#35486=CARTESIAN_POINT('Ctrl Pts',(2.47235715801771,-4.4910963817413,24.4678180733352));
#35487=CARTESIAN_POINT('Ctrl Pts',(4.32046165611542,-2.75972964344834,24.6068380688477));
#35488=CARTESIAN_POINT('Ctrl Pts',(5.11434197417513,-0.354968728314899,
24.7458580643602));
#35489=CARTESIAN_POINT('Ctrl Pts',(4.66028551989319,2.13640714751776,24.8848780598727));
#35490=CARTESIAN_POINT('Ctrl Pts',(3.06908538236661,4.10648408527718,25.0238980553852));
#35491=CARTESIAN_POINT('Ctrl Pts',(0.729006009651713,5.07454893214982,25.1629180508977));
#35492=CARTESIAN_POINT('Ctrl Pts',(-1.78895615058429,4.80438679939259,25.3019380464103));
#35493=CARTESIAN_POINT('Ctrl Pts',(-3.87039995211566,3.36191921936774,25.4409580419228));
#35494=CARTESIAN_POINT('Ctrl Pts',(-5.00743791447871,1.09911881047142,25.5799780374353));
#35495=CARTESIAN_POINT('Ctrl Pts',(-4.92262447538095,-1.43187461087609,
25.7189980329478));
#35496=CARTESIAN_POINT('Ctrl Pts',(-3.63665473303307,-3.61348017562008,
25.8580180284603));
#35497=CARTESIAN_POINT('Ctrl Pts',(-1.46331469112785,-4.91337020197141,
25.9970380239728));
#35498=CARTESIAN_POINT('Ctrl Pts',(1.06708481645005,-5.0143620353334,26.1360580194854));
#35499=CARTESIAN_POINT('Ctrl Pts',(3.33710783994068,-3.89181293120539,26.2750780149979));
#35500=CARTESIAN_POINT('Ctrl Pts',(4.79285219224344,-1.81963306471342,26.4140980105104));
#35501=CARTESIAN_POINT('Ctrl Pts',(5.07910562561647,0.696550551447801,26.5531180060229));
#35502=CARTESIAN_POINT('Ctrl Pts',(4.12602021289356,3.04277074878882,26.6921380015354));
#35503=CARTESIAN_POINT('Ctrl Pts',(2.1661557515472,4.64653267361053,26.831157997048));
#35504=CARTESIAN_POINT('Ctrl Pts',(-0.322266524396859,5.11650671006541,
26.9701779925605));
#35505=CARTESIAN_POINT('Ctrl Pts',(-2.73205341609784,4.33801576282051,27.109197988073));
#35506=CARTESIAN_POINT('Ctrl Pts',(-4.47519933244633,2.50101730537053,27.2482179835855));
#35507=CARTESIAN_POINT('Ctrl Pts',(-5.12636394626974,0.0537523699660611,
27.387237979098));
#35508=CARTESIAN_POINT('Ctrl Pts',(-4.52665833880949,-2.40662853605985,
27.5262579746105));
#35509=CARTESIAN_POINT('Ctrl Pts',(-2.82241505566153,-4.27977451280629,
27.6652779701231));
#35510=CARTESIAN_POINT('Ctrl Pts',(-0.429481897539188,-5.10862426946603,
27.8042979656356));
#35511=CARTESIAN_POINT('Ctrl Pts',(2.06824797846015,-4.6909324154678,27.9433179611481));
#35512=CARTESIAN_POINT('Ctrl Pts',(4.06131025114418,-3.1286188120067,28.0823379566606));
#35513=CARTESIAN_POINT('Ctrl Pts',(5.06338317820308,-0.802899381978309,
28.2213579521732));
#35514=CARTESIAN_POINT('Ctrl Pts',(4.82995365109632,1.71873335778196,28.3603779476856));
#35515=CARTESIAN_POINT('Ctrl Pts',(3.41798017828845,3.82098261285214,28.4993979431982));
#35516=CARTESIAN_POINT('Ctrl Pts',(1.17199459343186,4.9908842202417,28.6384179387107));
#35517=CARTESIAN_POINT('Ctrl Pts',(-1.35996622685374,4.94297364839307,28.7774379342232));
#35518=CARTESIAN_POINT('Ctrl Pts',(-3.5600853611114,3.68894142654656,28.9164579297357));
#35519=CARTESIAN_POINT('Ctrl Pts',(-4.89151768145639,1.53478057027402,29.0554779252482));
#35520=CARTESIAN_POINT('Ctrl Pts',(-5.0293839833238,-0.993877947827136,
29.1944979207607));
#35521=CARTESIAN_POINT('Ctrl Pts',(-3.94004388274326,-3.28002299213719,
29.3335179162733));
#35522=CARTESIAN_POINT('Ctrl Pts',(-1.88930431557573,-4.76581848479756,
29.4725379117858));
#35523=CARTESIAN_POINT('Ctrl Pts',(0.622439295016351,-5.08871948046958,
29.6115579072983));
#35524=CARTESIAN_POINT('Ctrl Pts',(2.9823031743109,-4.169935779288,29.7505779028108));
#35525=CARTESIAN_POINT('Ctrl Pts',(4.6144633106241,-2.23365731073393,29.8895978983234));
#35526=CARTESIAN_POINT('Ctrl Pts',(5.12066071722015,0.247649845567273,30.0286178938358));
#35527=CARTESIAN_POINT('Ctrl Pts',(4.37737953204971,2.6685286319025,30.1676378893484));
#35528=CARTESIAN_POINT('Ctrl Pts',(2.5659857896579,4.43826695390947,30.3066578848609));
#35529=CARTESIAN_POINT('Ctrl Pts',(0.128472784927027,5.12503574333136,30.4456778803734));
#35530=CARTESIAN_POINT('Ctrl Pts',(-2.34038851707551,4.56125840268145,30.5846978758859));
#35531=CARTESIAN_POINT('Ctrl Pts',(-4.2381779379304,2.88450071820604,30.7237178713985));
#35532=CARTESIAN_POINT('Ctrl Pts',(-5.10182100659037,0.503903803919262,
30.8627378669109));
#35533=CARTESIAN_POINT('Ctrl Pts',(-4.72058251039248,-1.99964931662224,
31.0017578624235));
#35534=CARTESIAN_POINT('Ctrl Pts',(-3.18748742514785,-4.01527340805273,
31.140777857936));
#35535=CARTESIAN_POINT('Ctrl Pts',(-0.876622142035253,-5.05114147960484,
31.2797978534485));
#35536=CARTESIAN_POINT('Ctrl Pts',(1.64814534238077,-4.85449416080395,31.418817848961));
#35537=CARTESIAN_POINT('Ctrl Pts',(3.77075333310117,-3.47331483280705,31.5578378444735));
#35538=CARTESIAN_POINT('Ctrl Pts',(4.97326998703416,-1.24462133315979,31.6968578399861));
#35539=CARTESIAN_POINT('Ctrl Pts',(4.96227246320154,1.28776885652777,31.8358778354985));
#35540=CARTESIAN_POINT('Ctrl Pts',(3.74044423769168,3.50593404553055,31.9748978310111));
#35541=CARTESIAN_POINT('Ctrl Pts',(1.60592031590668,4.86862573688399,32.1139178265236));
#35542=CARTESIAN_POINT('Ctrl Pts',(-0.920459884905055,5.0433372113286,32.2529378220362));
#35543=CARTESIAN_POINT('Ctrl Pts',(-3.22224115517232,3.98743759384455,32.3919578175486));
#35544=CARTESIAN_POINT('Ctrl Pts',(-4.73777206377099,1.95857409832829,32.5309778130612));
#35545=CARTESIAN_POINT('Ctrl Pts',(-5.09725200682841,-0.548195773218716,
32.6699978085737));
#35546=CARTESIAN_POINT('Ctrl Pts',(-4.21296525431996,-2.92120187470564,
32.8090178040862));
#35547=CARTESIAN_POINT('Ctrl Pts',(-2.3006842284502,-4.58141339630595,32.9480377995987));
#35548=CARTESIAN_POINT('Ctrl Pts',(0.172980542332811,-5.12372660852091,
33.0870577951112));
#35549=CARTESIAN_POINT('Ctrl Pts',(2.6044367981658,-4.41581312911349,33.2260777906237));
#35550=CARTESIAN_POINT('Ctrl Pts',(4.40039146492194,-2.6304090142663,33.3650977861363));
#35551=CARTESIAN_POINT('Ctrl Pts',(5.12261849486698,-0.203165900037072,
33.5041177816488));
#35552=CARTESIAN_POINT('Ctrl Pts',(4.59488922100946,2.2736511767512,33.6431377771613));
#35553=CARTESIAN_POINT('Ctrl Pts',(2.94597343817613,4.19568077056057,33.7821577726738));
#35554=CARTESIAN_POINT('Ctrl Pts',(0.578218633156638,5.09393363120894,33.9211777681863));
#35555=CARTESIAN_POINT('Ctrl Pts',(-1.93062573889086,4.74922950416415,34.0601977636989));
#35556=CARTESIAN_POINT('Ctrl Pts',(-3.9683833386113,3.24567871249196,34.1992177592113));
#35557=CARTESIAN_POINT('Ctrl Pts',(-5.03782643765737,0.950158624089521,
34.3382377547239));
#35558=CARTESIAN_POINT('Ctrl Pts',(-4.87800311377481,-1.57720710399561,
34.4772577502364));
#35559=CARTESIAN_POINT('Ctrl Pts',(-3.52791142457468,-3.71972278634396,
34.6162777457489));
#35560=CARTESIAN_POINT('Ctrl Pts',(-1.31698359682106,-4.95459895779621,
34.7552977412614));
#35561=CARTESIAN_POINT('Ctrl Pts',(1.21529784149338,-4.98051681890069,34.894317736774));
#35562=CARTESIAN_POINT('Ctrl Pts',(3.45103773577246,-3.79115222236799,35.0333377322865));
#35563=CARTESIAN_POINT('Ctrl Pts',(4.84469923268273,-1.67671881117096,35.172357727799));
#35564=CARTESIAN_POINT('Ctrl Pts',(5.05621875435371,0.846846228670134,35.3113777233115));
#35565=CARTESIAN_POINT('Ctrl Pts',(4.03398399357292,3.1637746074094,35.450397718824));
#35566=CARTESIAN_POINT('Ctrl Pts',(2.02742769347443,4.70871888889366,35.5894177143365));
#35567=CARTESIAN_POINT('Ctrl Pts',(-0.473835762447141,5.10470139157202,
35.7284377098491));
#35568=CARTESIAN_POINT('Ctrl Pts',(-2.85947983370614,4.25509949443244,35.8674577053615));
#35569=CARTESIAN_POINT('Ctrl Pts',(-4.54738995360437,2.36722226179743,36.0064777008742));
#35570=CARTESIAN_POINT('Ctrl Pts',(-5.1257037324805,-0.0982744815624442,
36.1454976963866));
#35571=CARTESIAN_POINT('Ctrl Pts',(-4.45330838705666,-2.53979153409525,
36.2845176918992));
#35572=CARTESIAN_POINT('Ctrl Pts',(-2.6942732895693,-4.36158091384358,36.4235376874117));
#35573=CARTESIAN_POINT('Ctrl Pts',(-0.277815843367409,-5.11911271453023,
36.5625576829242));
#35574=CARTESIAN_POINT('Ctrl Pts',(2.2064306964516,-4.62754364740596,36.7015776784367));
#35575=CARTESIAN_POINT('Ctrl Pts',(4.15229204114108,-3.00682015291364,36.8405976739492));
#35576=CARTESIAN_POINT('Ctrl Pts',(5.0849638193512,-0.652410593706373,36.9796176694617));
#35577=CARTESIAN_POINT('Ctrl Pts',(4.77686730943394,1.86119191244549,37.1186376649743));
#35578=CARTESIAN_POINT('Ctrl Pts',(3.30318030866942,3.92065000673483,37.2576576604868));
#35579=CARTESIAN_POINT('Ctrl Pts',(1.02349320199129,5.02344088174318,37.3966776559993));
#35580=CARTESIAN_POINT('Ctrl Pts',(-1.50593371666188,4.9004755144692,37.5356976515118));
#35581=CARTESIAN_POINT('Ctrl Pts',(-3.66790181632699,3.58175835207742,37.6747176470243));
#35582=CARTESIAN_POINT('Ctrl Pts',(-4.9348751000321,1.38906600778156,37.8137376425368));
#35583=CARTESIAN_POINT('Ctrl Pts',(-4.9977028386524,-1.1425685814939,37.9527576380494));
#35584=CARTESIAN_POINT('Ctrl Pts',(-3.84105460537178,-3.39540809703979,
38.0917776335618));
#35585=CARTESIAN_POINT('Ctrl Pts',(-1.74716101172614,-4.81974325311994,
38.2307976290744));
#35586=CARTESIAN_POINT('Ctrl Pts',(0.773052621671329,-5.06802587513306,
38.3698176245869));
#35587=CARTESIAN_POINT('Ctrl Pts',(3.10463577270955,-4.07967319104157,38.5088376200994));
#35588=CARTESIAN_POINT('Ctrl Pts',(4.67866513382612,-2.09585046995506,38.6478576156119));
#35589=CARTESIAN_POINT('Ctrl Pts',(5.11106605174182,0.39937506384781,38.7868776111245));
#35590=CARTESIAN_POINT('Ctrl Pts',(4.29632954630119,2.79715016695038,38.925897606637));
#35591=CARTESIAN_POINT('Ctrl Pts',(2.43325727176251,4.51240021233776,39.0649176021495));
#35592=CARTESIAN_POINT('Ctrl Pts',(-0.0235475379357751,5.12659166896957,
39.203937597662));
#35593=CARTESIAN_POINT('Ctrl Pts',(-2.47460657649937,4.48985733831679,39.3429575931745));
#35594=CARTESIAN_POINT('Ctrl Pts',(-4.3218435477304,2.75756504471465,39.481977588687));
#35595=CARTESIAN_POINT('Ctrl Pts',(-5.11451914728269,0.352406752162877,
39.6209975841996));
#35596=CARTESIAN_POINT('Ctrl Pts',(-4.6592147429618,-2.13874136020663,39.7600175797121));
#35597=CARTESIAN_POINT('Ctrl Pts',(-3.06702793278336,-4.10802096956888,
39.8990375752246));
#35598=CARTESIAN_POINT('Ctrl Pts',(-0.726463920132707,-5.07491347705914,
40.0380575707372));
#35599=CARTESIAN_POINT('Ctrl Pts',(1.79136259164118,-4.8034900533008,40.1770775662496));
#35600=CARTESIAN_POINT('Ctrl Pts',(3.87208355552747,-3.35997999486676,40.3160975617622));
#35601=CARTESIAN_POINT('Ctrl Pts',(5.007987868724,-1.09661029249428,40.4551175572747));
#35602=CARTESIAN_POINT('Ctrl Pts',(4.92190658760959,1.4343403256328,40.5941375527873));
#35603=CARTESIAN_POINT('Ctrl Pts',(3.6348441731013,3.61530143475791,40.7331575482997));
#35604=CARTESIAN_POINT('Ctrl Pts',(1.46085324887469,4.91410260496699,40.8721775438122));
#35605=CARTESIAN_POINT('Ctrl Pts',(-1.06959653114824,5.01382687050987,41.0111975393247));
#35606=CARTESIAN_POINT('Ctrl Pts',(-3.33905695036404,3.89014078268597,41.1502175348373));
#35607=CARTESIAN_POINT('Ctrl Pts',(-4.79376310122173,1.81723194894219,41.2892375303498));
#35608=CARTESIAN_POINT('Ctrl Pts',(-5.07875606471003,-0.699094744696433,
41.4282575258623));
#35609=CARTESIAN_POINT('Ctrl Pts',(-4.12449547751508,-3.04483721779157,
41.5672775213748));
#35610=CARTESIAN_POINT('Ctrl Pts',(-2.16382788825841,-4.64761718484712,
41.7062975168873));
#35611=CARTESIAN_POINT('Ctrl Pts',(0.324829499961922,-5.11634463487808,
41.8453175123999));
#35612=CARTESIAN_POINT('Ctrl Pts',(2.73422611919363,-4.33664664873797,41.9843375079123));
#35613=CARTESIAN_POINT('Ctrl Pts',(4.47645160765851,-2.49877522622239,42.1233575034249));
#35614=CARTESIAN_POINT('Ctrl Pts',(5.12639022930584,-0.0511844094298134,
42.2623774989373));
#35615=CARTESIAN_POINT('Ctrl Pts',(4.5254522164169,2.40889577686924,42.4013974944501));
#35616=CARTESIAN_POINT('Ctrl Pts',(2.82027083050778,4.28118781058226,42.5404174899624));
#35617=CARTESIAN_POINT('Ctrl Pts',(0.426922776212946,5.10883876923531,42.6794374854749));
#35618=CARTESIAN_POINT('Ctrl Pts',(-2.07059755167574,4.68989577772102,42.8184574809875));
#35619=CARTESIAN_POINT('Ctrl Pts',(-4.06287696323452,3.12658398392071,42.9574774765));
#35620=CARTESIAN_POINT('Ctrl Pts',(-5.06378473998233,0.800362876458667,
43.0964974720124));
#35621=CARTESIAN_POINT('Ctrl Pts',(-4.82909207855925,-1.72115261487393,
43.2355174675251));
#35622=CARTESIAN_POINT('Ctrl Pts',(-3.41606570142293,-3.82269430512735,
43.3745374630375));
#35623=CARTESIAN_POINT('Ctrl Pts',(-1.16949435856725,-4.99147068229099,
43.5135574585502));
#35624=CARTESIAN_POINT('Ctrl Pts',(1.36244214416074,-4.94229177919573,43.6525774540626));
#35625=CARTESIAN_POINT('Ctrl Pts',(3.5619328189657,-3.68715760716384,43.7915974495751));
#35626=CARTESIAN_POINT('Ctrl Pts',(4.89228588665652,-1.53233006565575,43.9306174450876));
#35627=CARTESIAN_POINT('Ctrl Pts',(5.02888548819363,0.996397196667345,44.0696374406001));
#35628=CARTESIAN_POINT('Ctrl Pts',(3.93840032373318,3.28199627009378,44.2086574361127));
#35629=CARTESIAN_POINT('Ctrl Pts',(1.88691673308091,4.76676429764577,44.3476774316251));
#35630=CARTESIAN_POINT('Ctrl Pts',(-0.624988313439745,5.08840704297079,
44.4866974271377));
#35631=CARTESIAN_POINT('Ctrl Pts',(-2.98439164956176,4.16844132847245,44.6257174226502));
#35632=CARTESIAN_POINT('Ctrl Pts',(-4.61558163949699,2.23134550350889,44.7647374181627));
#35633=CARTESIAN_POINT('Ctrl Pts',(-5.12053601930716,-0.250214911364518,
44.9037574136753));
#35634=CARTESIAN_POINT('Ctrl Pts',(-4.37604223455179,-2.67072106149444,
45.0427774091877));
#35635=CARTESIAN_POINT('Ctrl Pts',(-2.56376220292584,-4.43955177847271,
45.1817974047002));
#35636=CARTESIAN_POINT('Ctrl Pts',(-0.125905480353708,-5.12509945629427,
45.3208174002128));
#35637=CARTESIAN_POINT('Ctrl Pts',(2.34267309843463,-4.56008545761606,45.4598373957253));
#35638=CARTESIAN_POINT('Ctrl Pts',(4.23962234154865,-2.88237732226971,45.5988573912378));
#35639=CARTESIAN_POINT('Ctrl Pts',(5.10207278744068,-0.501348081219873,
45.7378773867503));
#35640=CARTESIAN_POINT('Ctrl Pts',(4.71958023211192,2.00201375109182,45.8768973822628));
#35641=CARTESIAN_POINT('Ctrl Pts',(3.18547565094819,4.01686961502235,46.0159173777754));
#35642=CARTESIAN_POINT('Ctrl Pts',(0.874091759514427,5.05157997292503,46.1549373732879));
#35643=CARTESIAN_POINT('Ctrl Pts',(-1.65057690143524,4.85366794489974,46.2939573688004));
#35644=CARTESIAN_POINT('Ctrl Pts',(-3.77249275049772,3.47142551039794,46.4329773643129));
#35645=CARTESIAN_POINT('Ctrl Pts',(-4.97389283229761,1.24212991268819,46.5719973598255));
#35646=CARTESIAN_POINT('Ctrl Pts',(-4.96162675741255,-1.29025445025019,
46.711017355338));
#35647=CARTESIAN_POINT('Ctrl Pts',(-3.7386875380274,-3.50780730955351,46.8500373508505));
#35648=CARTESIAN_POINT('Ctrl Pts',(-1.60348126941681,-4.86942958099378,
46.9890573463629));
#35649=CARTESIAN_POINT('Ctrl Pts',(0.922986132115756,-5.04287549192688,
47.1280773418756));
#35650=CARTESIAN_POINT('Ctrl Pts',(3.22423818221493,-3.98582297338294,47.267097337388));
#35651=CARTESIAN_POINT('Ctrl Pts',(4.73875257782023,-1.95620055686828,47.4061173329006));
#35652=CARTESIAN_POINT('Ctrl Pts',(5.09697676242384,0.550749075960109,47.545137328413));
#35653=CARTESIAN_POINT('Ctrl Pts',(4.21150139919949,2.92331191085705,47.6841573239256));
#35654=CARTESIAN_POINT('Ctrl Pts',(2.29838898109027,4.58256530821365,47.823177319438));
#35655=CARTESIAN_POINT('Ctrl Pts',(-0.17554717780017,5.12363930845007,47.9621973149507));
#35656=CARTESIAN_POINT('Ctrl Pts',(-2.6066484405486,4.41450794394377,48.101217310463));
#35657=CARTESIAN_POINT('Ctrl Pts',(-4.40170865916328,2.62820436986058,48.2402373059757));
#35658=CARTESIAN_POINT('Ctrl Pts',(-5.12271944202073,0.200599841061302,
48.3792573014881));
#35659=CARTESIAN_POINT('Ctrl Pts',(-4.59375005813751,-2.27595269926343,
48.5182772970008));
#35660=CARTESIAN_POINT('Ctrl Pts',(-2.94387062855117,-4.19715580510446,
48.6572972925132));
#35661=CARTESIAN_POINT('Ctrl Pts',(-0.575668206974144,-5.0942229675243,
48.7963172880258));
#35662=CARTESIAN_POINT('Ctrl Pts',(1.93300717656837,-4.74826115834551,48.9353372835382));
#35663=CARTESIAN_POINT('Ctrl Pts',(3.97000353982352,-3.24369166882115,49.0743572790508));
#35664=CARTESIAN_POINT('Ctrl Pts',(5.03831184387823,-0.947632464108493,
49.2133772745632));
#35665=CARTESIAN_POINT('Ctrl Pts',(4.87719276423381,1.57964568937599,49.3523972700758));
#35666=CARTESIAN_POINT('Ctrl Pts',(3.5260860626756,3.72149884840192,49.4914172655884));
#35667=CARTESIAN_POINT('Ctrl Pts',(1.31442635061977,4.95523991833443,49.6304372611009));
#35668=CARTESIAN_POINT('Ctrl Pts',(-1.21764365314759,4.9799428598698,49.7694572566133));
#35669=CARTESIAN_POINT('Ctrl Pts',(-3.45325039473801,3.78935331781989,49.9084772521259));
#35670=CARTESIAN_POINT('Ctrl Pts',(-4.38086558498562,2.3794052799023,50.0011572491342));
#35671=CARTESIAN_POINT('Ctrl Pts',(-4.6480804107302,1.60606351047903,50.0474972476384));
#35672=CARTESIAN_POINT('Origin',(-1.24911029906066,0.239195630269012,50.0000000000009));
#35673=CARTESIAN_POINT('Ctrl Pts',(2.58414624548329,5.32290476454751,4.9705248597598E-16));
#35674=CARTESIAN_POINT('Ctrl Pts',(2.70878071728787,5.24948204733452,-4.65901245328114E-15));
#35675=CARTESIAN_POINT('Ctrl Pts',(2.83052932791161,5.1715483667422,-4.68175003979269E-15));
#35676=CARTESIAN_POINT('Ctrl Pts',(2.94911242871282,5.08918295133373,-4.26395030395099E-15));
#35677=CARTESIAN_POINT('Ctrl Pts',(3.08549346351464,4.9944554521421,-3.77346057385956E-15));
#35678=CARTESIAN_POINT('Ctrl Pts',(3.21768860761213,4.89386633309252,-5.25738578620774E-16));
#35679=CARTESIAN_POINT('Ctrl Pts',(3.34538553148986,4.78775621336396,-2.98372437868011E-16));
#35680=CARTESIAN_POINT('Ctrl Pts',(3.47264577986623,4.68200895037717,-7.17838038905828E-17));
#35681=CARTESIAN_POINT('Ctrl Pts',(3.59543895347339,4.57077773595461,-3.19213500403142E-15));
#35682=CARTESIAN_POINT('Ctrl Pts',(3.71341282312126,4.45437143214694,-2.91433543964104E-16));
#35683=CARTESIAN_POINT('Ctrl Pts',(3.73983681572441,4.42829854566831,3.58270616402455E-16));
#35684=CARTESIAN_POINT('Ctrl Pts',(3.76601984852167,4.4019649171396,-2.99970839866107E-16));
#35685=CARTESIAN_POINT('Ctrl Pts',(3.79195443328246,4.37537715898866,5.41233724504764E-16));
#35686=CARTESIAN_POINT('Ctrl Pts',(3.81284818670717,4.35395718762434,1.21893575481746E-15));
#35687=CARTESIAN_POINT('Ctrl Pts',(3.8335749053755,4.3323781688725,2.30923463697903E-15));
#35688=CARTESIAN_POINT('Ctrl Pts',(3.85412745579704,4.31064779303087,2.44249065417534E-15));
#35689=CARTESIAN_POINT('Ctrl Pts',(3.96643270305237,4.19190655742792,3.17064115873798E-15));
#35690=CARTESIAN_POINT('Ctrl Pts',(4.07359664990735,4.06859126704819,1.94796900594839E-16));
#35691=CARTESIAN_POINT('Ctrl Pts',(4.17531676305532,3.94102919401566,5.41233724504764E-16));
#35692=CARTESIAN_POINT('Ctrl Pts',(4.27565036298719,3.81520587740661,8.82948382659753E-16));
#35693=CARTESIAN_POINT('Ctrl Pts',(4.37068783456493,3.68525011334924,3.32318783145209E-15));
#35694=CARTESIAN_POINT('Ctrl Pts',(4.46009412989579,3.55145356956696,3.99680288865056E-15));
#35695=CARTESIAN_POINT('Ctrl Pts',(4.54136308663149,3.42983455506927,4.60910868588099E-15));
#35696=CARTESIAN_POINT('Ctrl Pts',(4.61797895440299,3.30504150753519,1.83714078762577E-15));
#35697=CARTESIAN_POINT('Ctrl Pts',(4.68965400613746,3.17728361173429,6.60582699651968E-15));
#35698=CARTESIAN_POINT('Ctrl Pts',(4.69964533897967,3.15947446295409,6.42785852502324E-15));
#35699=CARTESIAN_POINT('Ctrl Pts',(4.70953894956037,3.14161057967267,3.94720314365333E-15));
#35700=CARTESIAN_POINT('Ctrl Pts',(4.71933011212868,3.12370005744086,3.46944695195361E-15));
#35701=CARTESIAN_POINT('Ctrl Pts',(4.75402963607211,3.06022581822917,1.32476286234967E-15));
#35702=CARTESIAN_POINT('Ctrl Pts',(4.78745810107654,2.99613834286576,2.98636140275833E-15));
#35703=CARTESIAN_POINT('Ctrl Pts',(4.81959019617709,2.93146624165117,3.99680288865056E-15));
#35704=CARTESIAN_POINT('Ctrl Pts',(4.89045936985516,2.78882822322252,6.09530346681891E-15));
#35705=CARTESIAN_POINT('Ctrl Pts',(4.95502572040444,2.64334740391261,2.50127599806969E-15));
#35706=CARTESIAN_POINT('Ctrl Pts',(5.01322356048623,2.49546111471738,3.3584246494911E-15));
#35707=CARTESIAN_POINT('Ctrl Pts',(5.07162447994012,2.34705878137496,3.35050327570378E-15));
#35708=CARTESIAN_POINT('Ctrl Pts',(5.12361247993031,2.19623337590386,3.66742926385365E-15));
#35709=CARTESIAN_POINT('Ctrl Pts',(5.16907007421431,2.04341570254536,2.1094237467878E-15));
#35710=CARTESIAN_POINT('Ctrl Pts',(5.21390629682536,1.89268693368885,1.53361017081258E-15));
#35711=CARTESIAN_POINT('Ctrl Pts',(5.25238939607452,1.74001924954489,2.50364342773557E-15));
#35712=CARTESIAN_POINT('Ctrl Pts',(5.28435659849648,1.58582660018576,3.60822483003176E-16));
#35713=CARTESIAN_POINT('Ctrl Pts',(5.30699058850528,1.47665236470033,-5.6045551921697E-16));
#35714=CARTESIAN_POINT('Ctrl Pts',(5.32635701224097,1.36671363152776,4.68892524957503E-15));
#35715=CARTESIAN_POINT('Ctrl Pts',(5.34238266598432,1.25616051768223,2.96984659087229E-15));
#35716=CARTESIAN_POINT('Ctrl Pts',(5.34800745436866,1.21735786534933,2.97246100623852E-15));
#35717=CARTESIAN_POINT('Ctrl Pts',(5.35322057164304,1.1784795614691,4.18116876452651E-15));
#35718=CARTESIAN_POINT('Ctrl Pts',(5.35801847245224,1.13953222602327,3.60822483003176E-15));
#35719=CARTESIAN_POINT('Ctrl Pts',(5.36104530259073,1.11496169540385,3.24677426288584E-15));
#35720=CARTESIAN_POINT('Ctrl Pts',(5.36390609156444,1.09036950507184,4.23502775416862E-15));
#35721=CARTESIAN_POINT('Ctrl Pts',(5.36659871116989,1.06577233689814,4.21884749357559E-15));
#35722=CARTESIAN_POINT('Ctrl Pts',(5.38350200775575,0.911360169664405,4.11727364219028E-15));
#35723=CARTESIAN_POINT('Ctrl Pts',(5.3938040052084,0.756577139039222,3.41788756861821E-15));
#35724=CARTESIAN_POINT('Ctrl Pts',(5.39741303532708,0.601823960215616,4.16333634234434E-15));
#35725=CARTESIAN_POINT('Ctrl Pts',(5.40010692670364,0.486311415232869,4.71976229534865E-15));
#35726=CARTESIAN_POINT('Ctrl Pts',(5.39907072069453,0.370815309359756,4.64881586728296E-15));
#35727=CARTESIAN_POINT('Ctrl Pts',(5.39424738914643,0.255503721863896,4.38538094726937E-15));
#35728=CARTESIAN_POINT('Ctrl Pts',(5.38775683563753,0.10033378975928,3.28400669008254E-15));
#35729=CARTESIAN_POINT('Ctrl Pts',(5.37441019776384,-0.0545030548216875,
3.88956332774984E-15));
#35730=CARTESIAN_POINT('Ctrl Pts',(5.35430867040058,-0.20856819236625,3.44169137633799E-15));
#35731=CARTESIAN_POINT('Ctrl Pts',(5.33439409683937,-0.361200450572585,
2.99798484791265E-15));
#35732=CARTESIAN_POINT('Ctrl Pts',(5.30784933644905,-0.513075978006889,
4.82803955867264E-15));
#35733=CARTESIAN_POINT('Ctrl Pts',(5.27472800412706,-0.663744430058508,
4.16333634234434E-15));
#35734=CARTESIAN_POINT('Ctrl Pts',(5.25927971775813,-0.734018456822544,
3.85330878861071E-15));
#35735=CARTESIAN_POINT('Ctrl Pts',(5.24240013898647,-0.804029489193217,
4.0102305330087E-15));
#35736=CARTESIAN_POINT('Ctrl Pts',(5.22409165812288,-0.873729395676655,
3.38618022510673E-15));
#35737=CARTESIAN_POINT('Ctrl Pts',(5.21856569074994,-0.894766608539603,
2.56437578661977E-15));
#35738=CARTESIAN_POINT('Ctrl Pts',(5.21290953948652,-0.915775466103714,
3.85815002206143E-15));
#35739=CARTESIAN_POINT('Ctrl Pts',(5.20712323720842,-0.93675461242177,4.66293670342566E-15));
#35740=CARTESIAN_POINT('Ctrl Pts',(5.20151158363336,-0.957100542478549,
5.44343240527273E-15));
#35741=CARTESIAN_POINT('Ctrl Pts',(5.19577955606844,-0.977411034412793,
5.45443632467064E-15));
#35742=CARTESIAN_POINT('Ctrl Pts',(5.18992938606291,-0.997678452611402,
5.32907051820075E-15));
#35743=CARTESIAN_POINT('Ctrl Pts',(5.14784463105866,-1.14347751975841,3.61622417999283E-15));
#35744=CARTESIAN_POINT('Ctrl Pts',(5.09962047179063,-1.28715624957652,8.5620977488092E-16));
#35745=CARTESIAN_POINT('Ctrl Pts',(5.04538459586395,-1.4283155996208,8.88178419700125E-16));
#35746=CARTESIAN_POINT('Ctrl Pts',(4.99037672763084,-1.57148420885657,1.49259684713777E-16));
#35747=CARTESIAN_POINT('Ctrl Pts',(4.92918455837232,-1.71206201410615,1.64585842454949E-15));
#35748=CARTESIAN_POINT('Ctrl Pts',(4.86189305225203,-1.84960649198228,1.83186799063151E-15));
#35749=CARTESIAN_POINT('Ctrl Pts',(4.79460154613173,-1.98715096985842,1.32090672371618E-15));
#35750=CARTESIAN_POINT('Ctrl Pts',(4.72121037278009,-2.12166286716527,2.86036616442949E-17));
#35751=CARTESIAN_POINT('Ctrl Pts',(4.64176094100255,-2.25266201421487,4.9960036108132E-16));
#35752=CARTESIAN_POINT('Ctrl Pts',(4.58721573082958,-2.34259816414614,6.83092991782841E-16));
#35753=CARTESIAN_POINT('Ctrl Pts',(4.52981397660194,-2.43087776084676,-2.86988927465527E-15));
#35754=CARTESIAN_POINT('Ctrl Pts',(4.46964647785047,-2.51737751627479,-6.66133814775094E-16));
#35755=CARTESIAN_POINT('Ctrl Pts',(4.43875608755086,-2.56178706065407,7.73849861614024E-16));
#35756=CARTESIAN_POINT('Ctrl Pts',(4.40713658096766,-2.60572729308483,-3.02645681402354E-15));
#35757=CARTESIAN_POINT('Ctrl Pts',(4.37479966267197,-2.6491803912438,-2.22044604925031E-15));
#35758=CARTESIAN_POINT('Ctrl Pts',(4.35422501482126,-2.67682780601809,-4.76874351599547E-16));
#35759=CARTESIAN_POINT('Ctrl Pts',(4.33335993315775,-2.70427800064961,-3.53144676016607E-15));
#35760=CARTESIAN_POINT('Ctrl Pts',(4.31220736271508,-2.73152621065158,-1.72084568816899E-15));
#35761=CARTESIAN_POINT('Ctrl Pts',(4.29999903121887,-2.74725267667535,-6.7584653999294E-16));
#35762=CARTESIAN_POINT('Ctrl Pts',(4.28770074273341,-2.7629043558843,-9.60893281977405E-16));
#35763=CARTESIAN_POINT('Ctrl Pts',(4.27531513424813,-2.77847828895174,-1.27675647831893E-15));
#35764=CARTESIAN_POINT('Ctrl Pts',(4.2326472946748,-2.83212975697908,-2.36489035600746E-15));
#35765=CARTESIAN_POINT('Ctrl Pts',(4.18893635069837,-2.8848676535937,-1.97050552418505E-15));
#35766=CARTESIAN_POINT('Ctrl Pts',(4.14421478376096,-2.93666546386691,-1.60982338570648E-15));
#35767=CARTESIAN_POINT('Ctrl Pts',(4.04793402946876,-3.048180613834,-8.3331328709926E-16));
#35768=CARTESIAN_POINT('Ctrl Pts',(3.94697122462269,-3.15534114389694,1.76209427040427E-15));
#35769=CARTESIAN_POINT('Ctrl Pts',(3.84162425024921,-3.25785439519544,6.66133814775094E-16));
#35770=CARTESIAN_POINT('Ctrl Pts',(3.73693153910005,-3.35973098226387,-4.23020117689046E-16));
#35771=CARTESIAN_POINT('Ctrl Pts',(3.62790829687089,-3.45701825449416,-4.73077726807451E-16));
#35772=CARTESIAN_POINT('Ctrl Pts',(3.51481945591763,-3.54938593120666,-3.33066907387547E-16));
#35773=CARTESIAN_POINT('Ctrl Pts',(3.40416108084475,-3.63976847406503,-1.96065151608371E-16));
#35774=CARTESIAN_POINT('Ctrl Pts',(3.2896093651333,-3.72544086154151,1.01954794998456E-15));
#35775=CARTESIAN_POINT('Ctrl Pts',(3.17139556349596,-3.80604757063947,0.));
#35776=CARTESIAN_POINT('Ctrl Pts',(3.06930259849605,-3.87566192883381,-8.8051201917039E-16));
#35777=CARTESIAN_POINT('Ctrl Pts',(2.96447778034216,-3.94149744951773,1.6904407368494E-15));
#35778=CARTESIAN_POINT('Ctrl Pts',(2.85706463458463,-4.00329423553976,1.11022302462516E-16));
#35779=CARTESIAN_POINT('Ctrl Pts',(-2.14763659377329,4.42399807618489,-0.576782495683815));
#35780=CARTESIAN_POINT('Ctrl Pts',(-2.88330608755926,4.0668662016747,-0.530467033922107));
#35781=CARTESIAN_POINT('Ctrl Pts',(-4.17230160089297,2.9788793155184,-0.437836110398691));
#35782=CARTESIAN_POINT('Ctrl Pts',(-5.08888703583058,0.619198826710665,
-0.298889725113564));
#35783=CARTESIAN_POINT('Ctrl Pts',(-4.76496251935548,-1.89075243704101,
-0.159943339828439));
#35784=CARTESIAN_POINT('Ctrl Pts',(-3.27959572109872,-3.9401495754155,-0.0209969545433121));
#35785=CARTESIAN_POINT('Ctrl Pts',(-0.994793592359738,-5.02895297143194,
0.117949430741813));
#35786=CARTESIAN_POINT('Ctrl Pts',(1.53248373837111,-4.89201169135806,0.256895816026939));
#35787=CARTESIAN_POINT('Ctrl Pts',(3.68621665053458,-3.56257803960143,0.395842201312065));
#35788=CARTESIAN_POINT('Ctrl Pts',(4.9414155898574,-1.36477265986452,0.534788586597191));
#35789=CARTESIAN_POINT('Ctrl Pts',(4.99212435123777,1.16571333689883,0.673734971882318));
#35790=CARTESIAN_POINT('Ctrl Pts',(3.82598040849633,3.41204582749421,0.812681357167443));
#35791=CARTESIAN_POINT('Ctrl Pts',(1.7272374644813,4.8266802929848,0.951627742452569));
#35792=CARTESIAN_POINT('Ctrl Pts',(-0.792527301558058,5.06478893033327,
1.09057412773769));
#35793=CARTESIAN_POINT('Ctrl Pts',(-3.11910999962733,4.06833403048449,1.22952051302282));
#35794=CARTESIAN_POINT('Ctrl Pts',(-4.68539612420164,2.08020462550141,1.36846689830795));
#35795=CARTESIAN_POINT('Ctrl Pts',(-5.10959655165582,-0.414983494631241,
1.50741328359307));
#35796=CARTESIAN_POINT('Ctrl Pts',(-4.28831062073647,-2.80901768900255,
1.6463596688782));
#35797=CARTESIAN_POINT('Ctrl Pts',(-2.42173032831516,-4.51834155710065,
1.78530605416333));
#35798=CARTESIAN_POINT('Ctrl Pts',(0.035157255613399,-5.12630005696805,
1.92425243944845));
#35799=CARTESIAN_POINT('Ctrl Pts',(2.48347510733904,-4.48470061981063,2.06319882473358));
#35800=CARTESIAN_POINT('Ctrl Pts',(4.3264351051218,-2.74993591880546,2.2021452100187));
#35801=CARTESIAN_POINT('Ctrl Pts',(5.11480773945644,-0.344862379916521,
2.34109159530383));
#35802=CARTESIAN_POINT('Ctrl Pts',(4.65642375300045,2.14427286129782,2.48003798058896));
#35803=CARTESIAN_POINT('Ctrl Pts',(3.06301623538964,4.11073227238675,2.61898436587408));
#35804=CARTESIAN_POINT('Ctrl Pts',(0.722985195410011,5.07518282222839,2.75793075115921));
#35805=CARTESIAN_POINT('Ctrl Pts',(-1.7932766287375,4.80253549758407,2.89687713644433));
#35806=CARTESIAN_POINT('Ctrl Pts',(-3.87241947927127,3.35924926864857,3.03582352172946));
#35807=CARTESIAN_POINT('Ctrl Pts',(-5.00764324831504,1.09713142788837,3.17476990701458));
#35808=CARTESIAN_POINT('Ctrl Pts',(-4.92223220735804,-1.43241696768481,
3.31371629229971));
#35809=CARTESIAN_POINT('Ctrl Pts',(-3.63700566890923,-3.61280750064991,
3.45266267758483));
#35810=CARTESIAN_POINT('Ctrl Pts',(-1.46524318859916,-4.91256050046432,
3.59160906286996));
#35811=CARTESIAN_POINT('Ctrl Pts',(1.06367868834549,-5.01485552338266,3.73055544815509));
#35812=CARTESIAN_POINT('Ctrl Pts',(3.33332426119376,-3.89475771289902,3.86950183344021));
#35813=CARTESIAN_POINT('Ctrl Pts',(4.79045755541376,-1.82529577938104,4.00844821872534));
#35814=CARTESIAN_POINT('Ctrl Pts',(5.07989599637985,0.68908993492224,4.14739460401047));
#35815=CARTESIAN_POINT('Ctrl Pts',(4.13108770591761,3.03550698211419,4.28634098929559));
#35816=CARTESIAN_POINT('Ctrl Pts',(2.17530882929733,4.64200600706508,4.42528737458072));
#35817=CARTESIAN_POINT('Ctrl Pts',(-0.310711030532882,5.11699588899118,
4.56423375986584));
#35818=CARTESIAN_POINT('Ctrl Pts',(-2.72099372600968,4.34469577939161,4.70318014515097));
#35819=CARTESIAN_POINT('Ctrl Pts',(-4.46802237261035,2.51335718717033,4.84212653043609));
#35820=CARTESIAN_POINT('Ctrl Pts',(-5.12595114339145,0.0693768550111596,
4.98107291572122));
#35821=CARTESIAN_POINT('Ctrl Pts',(-4.53440704045836,-2.39151438713821,
5.12001930100635));
#35822=CARTESIAN_POINT('Ctrl Pts',(-2.83758151034357,-4.26946360150824,
5.25896568629147));
#35823=CARTESIAN_POINT('Ctrl Pts',(-0.449083152114085,-5.10671250364994,
5.3979120715766));
#35824=CARTESIAN_POINT('Ctrl Pts',(2.04888117660792,-4.69917803414481,5.53685845686173));
#35825=CARTESIAN_POINT('Ctrl Pts',(4.0474218120441,-3.14619849148731,5.67580484214685));
#35826=CARTESIAN_POINT('Ctrl Pts',(5.05938578664962,-0.826319390003141,
5.81475122743198));
#35827=CARTESIAN_POINT('Ctrl Pts',(4.83810248260642,1.69497865480515,5.9536976127171));
#35828=CARTESIAN_POINT('Ctrl Pts',(3.43751066719364,3.80311828443151,6.09264399800223));
#35829=CARTESIAN_POINT('Ctrl Pts',(1.19901068379161,4.98423130007035,6.23159038328735));
#35830=CARTESIAN_POINT('Ctrl Pts',(-1.33175336588475,4.95041626986075,6.37053676857248));
#35831=CARTESIAN_POINT('Ctrl Pts',(-3.53789674349407,3.70991575441024,6.50948315385761));
#35832=CARTESIAN_POINT('Ctrl Pts',(-4.88166241063757,1.56510714681635,6.64842953914273));
#35833=CARTESIAN_POINT('Ctrl Pts',(-5.03550164459886,-0.961203131335693,
6.78737592442786));
#35834=CARTESIAN_POINT('Ctrl Pts',(-3.96191546336068,-3.25321596787409,
6.92632230971299));
#35835=CARTESIAN_POINT('Ctrl Pts',(-1.92259516547955,-4.75224327051151,
7.0652686949981));
#35836=CARTESIAN_POINT('Ctrl Pts',(0.585366061509484,-5.09289061795758,
7.20421508028325));
#35837=CARTESIAN_POINT('Ctrl Pts',(2.95064176641898,-4.19212373847805,7.34316146556836));
#35838=CARTESIAN_POINT('Ctrl Pts',(4.59668571432242,-2.26950847458025,7.48210785085349));
#35839=CARTESIAN_POINT('Ctrl Pts',(5.12226753756436,0.206309345551128,7.62105423613861));
#35840=CARTESIAN_POINT('Ctrl Pts',(4.39927438202509,2.63183836587758,7.76000062142375));
#35841=CARTESIAN_POINT('Ctrl Pts',(2.60393897221896,4.41584534391849,7.89894700670886));
#35842=CARTESIAN_POINT('Ctrl Pts',(0.173882118610286,5.12347082369706,8.037893391994));
#35843=CARTESIAN_POINT('Ctrl Pts',(-2.29855925727532,4.58222801846888,8.17683977727911));
#35844=CARTESIAN_POINT('Ctrl Pts',(-4.21071682236168,2.92404721479112,8.31578616256425));
#35845=CARTESIAN_POINT('Ctrl Pts',(-5.09649385800896,0.553117191673102,
8.45473254784938));
#35846=CARTESIAN_POINT('Ctrl Pts',(-4.73997836130483,-1.95263755131597,
8.59367893313449));
#35847=CARTESIAN_POINT('Ctrl Pts',(-3.22807253434404,-3.98242840305523,
8.73262531841964));
#35848=CARTESIAN_POINT('Ctrl Pts',(-0.929309994703741,-5.04148501993124,
8.87157170370474));
#35849=CARTESIAN_POINT('Ctrl Pts',(1.59597589585668,-4.87165774786078,9.01051808898988));
#35850=CARTESIAN_POINT('Ctrl Pts',(3.73223572409388,-3.51434272265025,9.149464474275));
#35851=CARTESIAN_POINT('Ctrl Pts',(4.95874687055243,-1.3003913819439,9.28841085956013));
#35852=CARTESIAN_POINT('Ctrl Pts',(4.97654191163832,1.23053601091333,9.42735724484525));
#35853=CARTESIAN_POINT('Ctrl Pts',(3.78128322873188,3.46151490196971,9.56630363013038));
#35854=CARTESIAN_POINT('Ctrl Pts',(1.6643203215817,4.84873448846372,9.7052500154155));
#35855=CARTESIAN_POINT('Ctrl Pts',(-0.858327898755408,5.05405396594313,
9.84419640070063));
#35856=CARTESIAN_POINT('Ctrl Pts',(-3.17175496261903,4.02742581924844,9.98314278598575));
#35857=CARTESIAN_POINT('Ctrl Pts',(-4.71205296672362,2.01909512188963,10.1220891712709));
#35858=CARTESIAN_POINT('Ctrl Pts',(-5.10376757689243,-0.481398788437435,
10.261035556556));
#35859=CARTESIAN_POINT('Ctrl Pts',(-4.25141665411314,-2.86454965144206,
10.3999819418411));
#35860=CARTESIAN_POINT('Ctrl Pts',(-2.36276444098316,-4.54945408470871,
10.5389283271262));
#35861=CARTESIAN_POINT('Ctrl Pts',(0.10182187557482,-5.12540930834815,10.6778747124114));
#35862=CARTESIAN_POINT('Ctrl Pts',(2.54158866734169,-4.45202373292053,10.8168210976965));
#35863=CARTESIAN_POINT('Ctrl Pts',(4.36183217315665,-2.69343801964384,10.9557674829816));
#35864=CARTESIAN_POINT('Ctrl Pts',(5.11886012587774,-0.278315080702345,
11.0947138682668));
#35865=CARTESIAN_POINT('Ctrl Pts',(4.62814367122823,2.20464836899615,11.2336602535518));
#35866=CARTESIAN_POINT('Ctrl Pts',(3.00929707817369,4.15021919514412,11.372606638837));
#35867=CARTESIAN_POINT('Ctrl Pts',(0.656921240898197,5.08415605147049,11.5115530241221));
#35868=CARTESIAN_POINT('Ctrl Pts',(-1.85558200448324,4.77880776942172,11.6504994094073));
#35869=CARTESIAN_POINT('Ctrl Pts',(-3.91577907005585,3.30860432009629,11.7894457946923));
#35870=CARTESIAN_POINT('Ctrl Pts',(-5.02148796540853,1.03191418524254,11.9283921799775));
#35871=CARTESIAN_POINT('Ctrl Pts',(-4.90318734078181,-1.49630951799562,
12.0673385652626));
#35872=CARTESIAN_POINT('Ctrl Pts',(-3.5897134876814,-3.65980127176404,12.2062849505478));
#35873=CARTESIAN_POINT('Ctrl Pts',(-1.40123136747207,-4.93120055638176,
12.3452313358328));
#35874=CARTESIAN_POINT('Ctrl Pts',(1.12880698971214,-5.00059826944982,12.484177721118));
#35875=CARTESIAN_POINT('Ctrl Pts',(3.38369373622936,-3.85107841673595,12.6231241064031));
#35876=CARTESIAN_POINT('Ctrl Pts',(4.81379042562212,-1.76284145930265,12.7620704916883));
#35877=CARTESIAN_POINT('Ctrl Pts',(5.07050477321974,0.755095766908508,12.9010168769733));
#35878=CARTESIAN_POINT('Ctrl Pts',(4.09126154085794,3.08897511753399,13.0399632622585));
#35879=CARTESIAN_POINT('Ctrl Pts',(2.11475552319577,4.66990335548396,13.1789096475436));
#35880=CARTESIAN_POINT('Ctrl Pts',(-0.377231346088842,5.11252235046219,
13.3178560328287));
#35881=CARTESIAN_POINT('Ctrl Pts',(-2.77726643493942,4.30894179837768,13.4568024181139));
#35882=CARTESIAN_POINT('Ctrl Pts',(-4.50033075749474,2.45503795196616,13.595748803399));
#35883=CARTESIAN_POINT('Ctrl Pts',(-5.12641989497035,0.00270793271152465,
13.7346951886841));
#35884=CARTESIAN_POINT('Ctrl Pts',(-4.50292189849674,-2.45028215691293,
13.8736415739692));
#35885=CARTESIAN_POINT('Ctrl Pts',(-2.7818171150605,-4.30600531941193,14.0125879592544));
#35886=CARTESIAN_POINT('Ctrl Pts',(-0.382632317267694,-5.1121209670967,
14.1515343445395));
#35887=CARTESIAN_POINT('Ctrl Pts',(2.10982077116202,-4.67213490665891,14.2904807298246));
#35888=CARTESIAN_POINT('Ctrl Pts',(4.08799587522889,-3.09329565294991,14.4294271151098));
#35889=CARTESIAN_POINT('Ctrl Pts',(5.06970421418836,-0.760452137276422,
14.5683735003949));
#35890=CARTESIAN_POINT('Ctrl Pts',(4.81565011293228,1.75775489254407,14.70731988568));
#35891=CARTESIAN_POINT('Ctrl Pts',(3.38776036301521,3.84750152634543,14.8462662709651));
#35892=CARTESIAN_POINT('Ctrl Pts',(1.13408929801697,4.99940293800877,14.9852126562503));
#35893=CARTESIAN_POINT('Ctrl Pts',(-1.39602096325972,4.93267815112508,15.1241590415354));
#35894=CARTESIAN_POINT('Ctrl Pts',(-3.58584504623797,3.66359162254993,15.2631054268205));
#35895=CARTESIAN_POINT('Ctrl Pts',(-4.90160381152525,1.50148871034336,15.4020518121056));
#35896=CARTESIAN_POINT('Ctrl Pts',(-5.02257534047868,-1.02660860198166,
15.5409981973908));
#35897=CARTESIAN_POINT('Ctrl Pts',(-3.91927229705261,-3.30446560490549,
15.6799445826759));
#35898=CARTESIAN_POINT('Ctrl Pts',(-1.86062959414104,-4.77684475211974,
15.818890967961));
#35899=CARTESIAN_POINT('Ctrl Pts',(0.651549660500337,-5.08484722605797,
15.9578373532461));
#35900=CARTESIAN_POINT('Ctrl Pts',(3.00491085310802,-4.15339608481073,16.0967837385313));
#35901=CARTESIAN_POINT('Ctrl Pts',(4.62581196292139,-2.20953659307574,16.2357301238164));
#35902=CARTESIAN_POINT('Ctrl Pts',(5.11915129836543,0.272907048078267,16.3746765091015));
#35903=CARTESIAN_POINT('Ctrl Pts',(4.36467525187932,2.6888284099361,16.5136228943866));
#35904=CARTESIAN_POINT('Ctrl Pts',(2.54629063950183,4.44933615853341,16.6525692796718));
#35905=CARTESIAN_POINT('Ctrl Pts',(0.107236615018882,5.12529887722137,16.7915156649569));
#35906=CARTESIAN_POINT('Ctrl Pts',(-2.35795680053252,4.55194771490949,16.930462050242));
#35907=CARTESIAN_POINT('Ctrl Pts',(-4.24838799591456,2.86903950976915,17.0694084355271));
#35908=CARTESIAN_POINT('Ctrl Pts',(-5.10325614954743,0.486790452406175,
17.2083548208123));
#35909=CARTESIAN_POINT('Ctrl Pts',(-4.7141834328707,-2.01411589380919,17.3473012060974));
#35910=CARTESIAN_POINT('Ctrl Pts',(-3.1760080118737,-4.02407273554559,17.4862475913825));
#35911=CARTESIAN_POINT('Ctrl Pts',(-0.863666831873859,-5.05314435534632,
17.6251939766677));
#35912=CARTESIAN_POINT('Ctrl Pts',(1.65919689275546,-4.85049007251,17.7641403619528));
#35913=CARTESIAN_POINT('Ctrl Pts',(3.77762416224581,-3.46550774941626,17.9030867472379));
#35914=CARTESIAN_POINT('Ctrl Pts',(4.97523912085433,-1.23579284783815,18.042033132523));
#35915=CARTESIAN_POINT('Ctrl Pts',(4.96011791638736,1.2951519323927,18.1809795178082));
#35916=CARTESIAN_POINT('Ctrl Pts',(3.73594640816555,3.51039779907668,18.3199259030933));
#35917=CARTESIAN_POINT('Ctrl Pts',(1.60112172279223,4.86996894253445,18.4588722883784));
#35918=CARTESIAN_POINT('Ctrl Pts',(-0.923983342588718,5.04246398649172,
18.5978186736635));
#35919=CARTESIAN_POINT('Ctrl Pts',(-3.22386345165755,3.98583651414782,18.7367650589486));
#35920=CARTESIAN_POINT('Ctrl Pts',(-4.73791283024863,1.95764406504679,18.8757114442338));
#35921=CARTESIAN_POINT('Ctrl Pts',(-5.09707536075682,-0.54773263478927,
19.0146578295189));
#35922=CARTESIAN_POINT('Ctrl Pts',(-4.21380361509104,-2.91959712390135,
19.153604214804));
#35923=CARTESIAN_POINT('Ctrl Pts',(-2.30339892084015,-4.57979712257211,
19.2925506000892));
#35924=CARTESIAN_POINT('Ctrl Pts',(0.168469273241985,-5.12365166423526,
19.4314969853743));
#35925=CARTESIAN_POINT('Ctrl Pts',(2.59927234963534,-4.41859384022433,19.5704433706594));
#35926=CARTESIAN_POINT('Ctrl Pts',(4.3964914917667,-2.63648456002883,19.7093897559445));
#35927=CARTESIAN_POINT('Ctrl Pts',(5.12204672122891,-0.211720707526411,
19.8483361412297));
#35928=CARTESIAN_POINT('Ctrl Pts',(4.59908079685158,2.26465098778562,19.9872825265148));
#35929=CARTESIAN_POINT('Ctrl Pts',(2.95506893603482,4.18900416038578,20.1262289117999));
#35930=CARTESIAN_POINT('Ctrl Pts',(0.59074617637326,5.09226935928841,20.265175297085));
#35931=CARTESIAN_POINT('Ctrl Pts',(-1.91757353175325,4.75427176576673,20.4041216823702));
#35932=CARTESIAN_POINT('Ctrl Pts',(-3.9584763558217,3.25739976251733,20.5430680676553));
#35933=CARTESIAN_POINT('Ctrl Pts',(-5.03448336065964,0.9665224072357,20.6820144529404));
#35934=CARTESIAN_POINT('Ctrl Pts',(-4.88331316143473,-1.55994898628306,
20.8209608382255));
#35935=CARTESIAN_POINT('Ctrl Pts',(-3.54181415134507,-3.7061760332962,20.9599072235107));
#35936=CARTESIAN_POINT('Ctrl Pts',(-1.33698254559689,-4.94900656144409,
21.0988536087958));
#35937=CARTESIAN_POINT('Ctrl Pts',(1.19374436750442,-4.98549522690562,21.2377999940809));
#35938=CARTESIAN_POINT('Ctrl Pts',(3.43349090181907,-3.80674775885835,21.376746379366));
#35939=CARTESIAN_POINT('Ctrl Pts',(4.83630910342842,-1.70008897665469,21.5156927646512));
#35940=CARTESIAN_POINT('Ctrl Pts',(5.06025593763869,0.820973883896323,21.6546391499363));
#35941=CARTESIAN_POINT('Ctrl Pts',(4.05074339011407,3.14192079147367,21.7935855352214));
#35942=CARTESIAN_POINT('Ctrl Pts',(2.05384453266536,4.69701084819781,21.9325319205066));
#35943=CARTESIAN_POINT('Ctrl Pts',(-0.443687857683883,5.10718409276494,
22.0714783057917));
#35944=CARTESIAN_POINT('Ctrl Pts',(-2.83306940401134,4.27245901378845,22.2104246910768));
#35945=CARTESIAN_POINT('Ctrl Pts',(-4.53187796775673,2.39630347781925,22.3493710763619));
#35946=CARTESIAN_POINT('Ctrl Pts',(-5.12602157678528,-0.063961447601001,
22.488317461647));
#35947=CARTESIAN_POINT('Ctrl Pts',(-4.47067514365369,-2.50863549212803,
22.6272638469322));
#35948=CARTESIAN_POINT('Ctrl Pts',(-2.72558221022914,-4.34181873040893,
22.7662102322173));
#35949=CARTESIAN_POINT('Ctrl Pts',(-0.316116764953832,-5.11666477926417,
22.9051566175024));
#35950=CARTESIAN_POINT('Ctrl Pts',(2.17040351593876,-4.64430154602909,23.0441030027875));
#35951=CARTESIAN_POINT('Ctrl Pts',(4.12787850507594,-3.03986962216792,23.1830493880727));
#35952=CARTESIAN_POINT('Ctrl Pts',(5.07916516471065,-0.694456263588383,
23.3219957733578));
#35953=CARTESIAN_POINT('Ctrl Pts',(4.79238323631331,1.82023382804259,23.460942158643));
#35954=CARTESIAN_POINT('Ctrl Pts',(3.33743706157193,3.89123401153074,23.599888543928));
#35955=CARTESIAN_POINT('Ctrl Pts',(1.06897609523158,5.01372898951177,23.7388349292132));
#35956=CARTESIAN_POINT('Ctrl Pts',(-1.46005244116113,4.91410573161657,23.8777813144983));
#35957=CARTESIAN_POINT('Ctrl Pts',(-3.63318684817203,3.61664784001942,24.0167276997835));
#35958=CARTESIAN_POINT('Ctrl Pts',(-4.92071616747572,1.43761631584731,24.1556740850685));
#35959=CARTESIAN_POINT('Ctrl Pts',(-5.00879953060122,-1.09184043463153,
24.2946204703537));
#35960=CARTESIAN_POINT('Ctrl Pts',(-3.87596623488826,-3.35515633293791,
24.4335668556388));
#35961=CARTESIAN_POINT('Ctrl Pts',(-1.7983493205939,-4.80063829022421,24.572513240924));
#35962=CARTESIAN_POINT('Ctrl Pts',(0.717623058020787,-5.075943795891,24.7114596262091));
#35963=CARTESIAN_POINT('Ctrl Pts',(3.05867169673505,-4.11396593617877,24.8504060114942));
#35964=CARTESIAN_POINT('Ctrl Pts',(4.65415581332253,-2.14919099611072,24.9893523967793));
#35965=CARTESIAN_POINT('Ctrl Pts',(5.1151692187947,0.339458591793783,25.1282987820644));
#35966=CARTESIAN_POINT('Ctrl Pts',(4.32933789154216,2.74536367232189,25.2672451673496));
#35967=CARTESIAN_POINT('Ctrl Pts',(2.48821163359192,4.48207442362409,25.4061915526347));
#35968=CARTESIAN_POINT('Ctrl Pts',(0.0405729736962985,5.12626005058783,
25.5451379379198));
#35969=CARTESIAN_POINT('Ctrl Pts',(-2.41695552490853,4.52089750636546,25.684084323205));
#35970=CARTESIAN_POINT('Ctrl Pts',(-4.28534060780991,2.81354654262248,25.8230307084901));
#35971=CARTESIAN_POINT('Ctrl Pts',(-5.10915528917953,0.420381378626828,
25.9619770937752));
#35972=CARTESIAN_POINT('Ctrl Pts',(-4.6875911593107,-2.07525357380717,26.1009234790603));
#35973=CARTESIAN_POINT('Ctrl Pts',(-3.12340630739848,-4.06503644649722,
26.2398698643455));
#35974=CARTESIAN_POINT('Ctrl Pts',(-0.797877590608867,-5.06394901463785,
26.3788162496306));
#35975=CARTESIAN_POINT('Ctrl Pts',(1.722137257266,-4.82850199747124,26.5177626349157));
#35976=CARTESIAN_POINT('Ctrl Pts',(3.82237366255062,-3.41608662892009,26.6567090202008));
#35977=CARTESIAN_POINT('Ctrl Pts',(4.99088987172806,-1.17098529483918,26.795655405486));
#35978=CARTESIAN_POINT('Ctrl Pts',(4.9428549792707,1.35954879513255,26.9346017907711));
#35979=CARTESIAN_POINT('Ctrl Pts',(3.68997769902266,3.55868695633134,27.0735481760562));
#35980=CARTESIAN_POINT('Ctrl Pts',(1.53765231430271,4.89037970231012,27.2124945613413));
#35981=CARTESIAN_POINT('Ctrl Pts',(-0.989482506204021,5.03002113736749,
27.3514409466265));
#35982=CARTESIAN_POINT('Ctrl Pts',(-3.2754266645425,3.94357305468675,27.4903873319116));
#35983=CARTESIAN_POINT('Ctrl Pts',(-4.76297133511717,1.89586189721181,27.6293337171967));
#35984=CARTESIAN_POINT('Ctrl Pts',(-5.08952103811793,-0.613973839021256,
27.7682801024819));
#35985=CARTESIAN_POINT('Ctrl Pts',(-4.17547786392657,-2.97415078304826,
27.9072264877669));
#35986=CARTESIAN_POINT('Ctrl Pts',(-2.24364380959848,-4.60936554507209,
28.0461728730521));
#35987=CARTESIAN_POINT('Ctrl Pts',(0.23508817644013,-5.12102741856997,28.1851192583372));
#35988=CARTESIAN_POINT('Ctrl Pts',(2.65651639754307,-4.38441659768233,28.3240656436223));
#35989=CARTESIAN_POINT('Ctrl Pts',(4.43040719886656,-2.57908517204815,28.4630120289075));
#35990=CARTESIAN_POINT('Ctrl Pts',(5.12436698648373,-0.145090524442568,
28.6019584141926));
#35991=CARTESIAN_POINT('Ctrl Pts',(4.5692400455193,2.3242705692045,28.7409047994777));
#35992=CARTESIAN_POINT('Ctrl Pts',(2.90034098097046,4.22708060800249,28.8798511847629));
#35993=CARTESIAN_POINT('Ctrl Pts',(0.524471194526165,5.09952137347807,29.018797570048));
#35994=CARTESIAN_POINT('Ctrl Pts',(-1.97924072546044,4.72893163654605,29.1577439553331));
#35995=CARTESIAN_POINT('Ctrl Pts',(-4.0005041148555,3.20564425653746,29.2966903406182));
#35996=CARTESIAN_POINT('Ctrl Pts',(-5.0466272360609,0.90096715406042,29.4356367259034));
#35997=CARTESIAN_POINT('Ctrl Pts',(-4.86261303078498,-1.62332460872357,
29.5745831111885));
#35998=CARTESIAN_POINT('Ctrl Pts',(-3.49331576147361,-3.75192394153818,
29.7135294964736));
#35999=CARTESIAN_POINT('Ctrl Pts',(-1.27250758985748,-4.96597550398736,
29.8524758817587));
#36000=CARTESIAN_POINT('Ctrl Pts',(1.25847983837766,-4.96954895024129,29.9914222670439));
#36001=CARTESIAN_POINT('Ctrl Pts',(3.48270733539568,-3.76177323724179,30.130368652329));
#36002=CARTESIAN_POINT('Ctrl Pts',(4.8580097800802,-1.63704894523421,30.2693150376141));
#36003=CARTESIAN_POINT('Ctrl Pts',(5.04915122309893,0.886713143426884,30.4082614228992));
#36004=CARTESIAN_POINT('Ctrl Pts',(4.00954010682405,3.19433504883518,30.5472078081844));
#36005=CARTESIAN_POINT('Ctrl Pts',(1.99258616003768,4.7233239003136,30.6861541934695));
#36006=CARTESIAN_POINT('Ctrl Pts',(-0.510069325031026,5.1009820187989,30.8251005787546));
#36007=CARTESIAN_POINT('Ctrl Pts',(-2.88839319485177,4.23525359623026,30.9640469640397));
#36008=CARTESIAN_POINT('Ctrl Pts',(-4.56265866758056,2.33716369893069,31.1029933493249));
#36009=CARTESIAN_POINT('Ctrl Pts',(-5.12475625620675,-0.13062000963517,
31.24193973461));
#36010=CARTESIAN_POINT('Ctrl Pts',(-4.43767223006419,-2.56656452304717,
31.3808861198952));
#36011=CARTESIAN_POINT('Ctrl Pts',(-2.66888630727981,-4.376897777109,31.5198325051802));
#36012=CARTESIAN_POINT('Ctrl Pts',(-0.249547745445644,-5.1203431716234,
31.6587788904654));
#36013=CARTESIAN_POINT('Ctrl Pts',(2.23061916412508,-4.61568265991991,31.7977252757505));
#36014=CARTESIAN_POINT('Ctrl Pts',(4.16706295593753,-2.98592943548579,31.9366716610356));
#36015=CARTESIAN_POINT('Ctrl Pts',(5.08776703801517,-0.62834293131509,32.0756180463208));
#36016=CARTESIAN_POINT('Ctrl Pts',(4.76830578805043,1.88240489377079,32.2145644316058));
#36017=CARTESIAN_POINT('Ctrl Pts',(3.28654927442038,3.9343083431849,32.353510816891));
#36018=CARTESIAN_POINT('Ctrl Pts',(1.00368208851879,5.02720703150705,32.4924572021761));
#36019=CARTESIAN_POINT('Ctrl Pts',(-1.52383696946585,4.89470215262752,32.6314035874613));
#36020=CARTESIAN_POINT('Ctrl Pts',(-3.67991414202303,3.56909234677198,32.7703499727464));
#36021=CARTESIAN_POINT('Ctrl Pts',(-4.93899624587321,1.37350076654429,32.9092963580315));
#36022=CARTESIAN_POINT('Ctrl Pts',(-4.99417654497228,-1.15688759613717,
33.0482427433167));
#36023=CARTESIAN_POINT('Ctrl Pts',(-3.83200460154611,-3.40527957826912,
33.1871891286017));
#36024=CARTESIAN_POINT('Ctrl Pts',(-1.73576487876693,-4.82361986044573,
33.3261355138869));
#36025=CARTESIAN_POINT('Ctrl Pts',(0.783575078582641,-5.06618183336047,
33.465081899172));
#36026=CARTESIAN_POINT('Ctrl Pts',(3.1119152043264,-4.07383996169826,33.6040282844571));
#36027=CARTESIAN_POINT('Ctrl Pts',(4.6817124715184,-2.08848189038745,33.7429746697423));
#36028=CARTESIAN_POINT('Ctrl Pts',(5.11032197237104,0.405952720337242,33.8819210550274));
#36029=CARTESIAN_POINT('Ctrl Pts',(4.29326827788569,2.80143459080304,34.0208674403125));
#36030=CARTESIAN_POINT('Ctrl Pts',(2.42971177782606,4.51405460192282,34.1598138255976));
#36031=CARTESIAN_POINT('Ctrl Pts',(-0.0260975300371019,5.126354181226,34.2987602108827));
#36032=CARTESIAN_POINT('Ctrl Pts',(-2.47554545150775,4.48908264459084,34.4377065961679));
#36033=CARTESIAN_POINT('Ctrl Pts',(-4.32156840797594,2.75757769929185,34.576652981453));
#36034=CARTESIAN_POINT('Ctrl Pts',(-5.11419027913967,0.353901202598625,
34.7155993667381));
#36035=CARTESIAN_POINT('Ctrl Pts',(-4.66020603837503,-2.13604025063673,
34.8545457520232));
#36036=CARTESIAN_POINT('Ctrl Pts',(-3.07027631783819,-4.1053126074112,34.9934921373084));
#36037=CARTESIAN_POINT('Ctrl Pts',(-0.731953398335376,-5.07389717033296,
35.1324385225935));
#36038=CARTESIAN_POINT('Ctrl Pts',(1.78478634381352,-4.80569724175214,35.2713849078787));
#36039=CARTESIAN_POINT('Ctrl Pts',(3.86647665619062,-3.36608772012562,35.4103312931637));
#36040=CARTESIAN_POINT('Ctrl Pts',(5.00569647604503,-1.10597968433321,35.5492776784489));
#36041=CARTESIAN_POINT('Ctrl Pts',(4.92475602009802,1.42371570720972,35.688224063734));
#36042=CARTESIAN_POINT('Ctrl Pts',(3.6433848763349,3.60637420622729,35.8271704490192));
#36043=CARTESIAN_POINT('Ctrl Pts',(1.47392283116901,4.90996331556623,35.9661168343042));
#36044=CARTESIAN_POINT('Ctrl Pts',(-1.05481431123771,5.01672752312256,36.1050632195895));
#36045=CARTESIAN_POINT('Ctrl Pts',(-3.32643588000179,3.90064258920041,36.2440096048745));
#36046=CARTESIAN_POINT('Ctrl Pts',(-4.78722424299679,1.83375906806513,36.3829559901597));
#36047=CARTESIAN_POINT('Ctrl Pts',(-5.08110588669488,-0.680111197262768,
36.5219023754447));
#36048=CARTESIAN_POINT('Ctrl Pts',(-4.13644588294086,-3.02820140181411,
36.6608487607299));
#36049=CARTESIAN_POINT('Ctrl Pts',(-2.18350921408743,-4.63815435108003,
36.799795146015));
#36050=CARTESIAN_POINT('Ctrl Pts',(0.30166731741563,-5.11753701521061,36.9387415313002));
#36051=CARTESIAN_POINT('Ctrl Pts',(2.71331112895062,-4.34949778594726,37.0776879165853));
#36052=CARTESIAN_POINT('Ctrl Pts',(4.46357355803887,-2.52124956408992,37.2166343018704));
#36053=CARTESIAN_POINT('Ctrl Pts',(5.12582052919834,-0.0784358011124148,
37.3555806871555));
#36054=CARTESIAN_POINT('Ctrl Pts',(4.53862646442101,2.38349702934671,37.4945270724407));
#36055=CARTESIAN_POINT('Ctrl Pts',(2.84512246952923,4.26444209783968,37.6334734577258));
#36056=CARTESIAN_POINT('Ctrl Pts',(0.458107504940694,5.10591086745201,37.7724198430109));
#36057=CARTESIAN_POINT('Ctrl Pts',(-2.04057315537071,4.70279166772542,37.911366228296));
#36058=CARTESIAN_POINT('Ctrl Pts',(-4.04185523868785,3.15334655595275,38.0503126135812));
#36059=CARTESIAN_POINT('Ctrl Pts',(-5.05791753762779,0.835259513567289,
38.1892589988663));
#36060=CARTESIAN_POINT('Ctrl Pts',(-4.84109045000053,-1.68642566612377,
38.3282053841514));
#36061=CARTESIAN_POINT('Ctrl Pts',(-3.44422652096274,-3.79703725880379,
38.4671517694365));
#36062=CARTESIAN_POINT('Ctrl Pts',(-1.20781740538567,-4.9821045139273,38.6060981547217));
#36063=CARTESIAN_POINT('Ctrl Pts',(1.32300245313715,-4.9527621365699,38.7450445400067));
#36064=CARTESIAN_POINT('Ctrl Pts',(3.53133471261537,-3.71616245876376,38.883990925292));
#36065=CARTESIAN_POINT('Ctrl Pts',(4.87888878517958,-1.57373202747361,39.022937310577));
#36066=CARTESIAN_POINT('Ctrl Pts',(5.03719250782395,0.952302426527237,39.1618836958622));
#36067=CARTESIAN_POINT('Ctrl Pts',(3.96765866000753,3.24620902440288,39.3008300811473));
#36068=CARTESIAN_POINT('Ctrl Pts',(1.93099076639979,4.74883806130785,39.4397764664324));
#36069=CARTESIAN_POINT('Ctrl Pts',(-0.57636452053578,5.09391717756727,39.5787228517175));
#36070=CARTESIAN_POINT('Ctrl Pts',(-2.94322845013388,4.19733183853384,39.7176692370027));
#36071=CARTESIAN_POINT('Ctrl Pts',(-4.59266765079613,2.2776286180539,39.8566156222878));
#36072=CARTESIAN_POINT('Ctrl Pts',(-5.12262414724796,-0.197256478929643,
39.995562007573));
#36073=CARTESIAN_POINT('Ctrl Pts',(-4.40391873975792,-2.62405945170006,
40.134508392858));
#36074=CARTESIAN_POINT('Ctrl Pts',(-2.61173899561465,-4.41123652633059,
40.2734547781432));
#36075=CARTESIAN_POINT('Ctrl Pts',(-0.182936518059435,-5.12315552202035,
40.4124011634283));
#36076=CARTESIAN_POINT('Ctrl Pts',(2.29045753099789,-4.58628308885772,40.5513475487134));
#36077=CARTESIAN_POINT('Ctrl Pts',(4.20554260025436,-2.93148421621083,40.6902939339986));
#36078=CARTESIAN_POINT('Ctrl Pts',(5.09550837920273,-0.562123322698978,
40.8292403192837));
#36079=CARTESIAN_POINT('Ctrl Pts',(4.74342184054261,1.94425757427114,40.9681867045688));
#36080=CARTESIAN_POINT('Ctrl Pts',(3.23510560859279,3.9767172358239,41.1071330898539));
#36081=CARTESIAN_POINT('Ctrl Pts',(0.938218321542545,5.03983478435249,41.2460794751391));
#36082=CARTESIAN_POINT('Ctrl Pts',(-1.58736375981927,4.87447069603047,41.3850258604242));
#36083=CARTESIAN_POINT('Ctrl Pts',(-3.72601902445393,3.52093318622417,41.5239722457093));
#36084=CARTESIAN_POINT('Ctrl Pts',(-4.95644095487116,1.30915290677719,41.6629186309945));
#36085=CARTESIAN_POINT('Ctrl Pts',(-4.97870885688693,-1.22173908458518,
41.8018650162796));
#36086=CARTESIAN_POINT('Ctrl Pts',(-3.78739483258627,-3.45482686317944,
41.9408114015646));
#36087=CARTESIAN_POINT('Ctrl Pts',(-1.6728868540352,-4.84578557573935,42.0797577868498));
#36088=CARTESIAN_POINT('Ctrl Pts',(0.849394567227056,-5.05556298958016,
42.218704172135));
#36089=CARTESIAN_POINT('Ctrl Pts',(3.16463237040904,-4.03302494817558,42.35765055742));
#36090=CARTESIAN_POINT('Ctrl Pts',(4.7084772766451,-2.02741954409147,42.4965969427052));
#36091=CARTESIAN_POINT('Ctrl Pts',(5.10461037894552,0.47237818705881,42.6355433279903));
#36092=CARTESIAN_POINT('Ctrl Pts',(4.25647251163379,2.85703168168524,42.7744897132754));
#36093=CARTESIAN_POINT('Ctrl Pts',(2.37080096672289,4.54527128438262,42.9134360985606));
#36094=CARTESIAN_POINT('Ctrl Pts',(-0.0927636196998844,5.12558125321486,
43.0523824838456));
#36095=CARTESIAN_POINT('Ctrl Pts',(-2.53371667057728,4.45650851067134,43.1913288691309));
#36096=CARTESIAN_POINT('Ctrl Pts',(-4.35706526893369,2.70114244620665,43.3302752544159));
#36097=CARTESIAN_POINT('Ctrl Pts',(-5.11836026782228,0.287361168611337,
43.4692216397011));
#36098=CARTESIAN_POINT('Ctrl Pts',(-4.63203270191418,-2.19646564299215,
43.6081680249862));
#36099=CARTESIAN_POINT('Ctrl Pts',(-3.01662702946576,-4.14489440607887,
43.7471144102713));
#36100=CARTESIAN_POINT('Ctrl Pts',(-0.665905405305666,-5.08298713982556,
43.8860607955565));
#36101=CARTESIAN_POINT('Ctrl Pts',(1.8471335560889,-4.78207966249181,44.0250071808416));
#36102=CARTESIAN_POINT('Ctrl Pts',(3.90992568369618,-3.31551947972265,44.1639535661266));
#36103=CARTESIAN_POINT('Ctrl Pts',(5.01965642945332,-1.04078701120603,44.3028999514119));
#36104=CARTESIAN_POINT('Ctrl Pts',(4.90582410008189,1.48764181559379,44.4418463366969));
#36105=CARTESIAN_POINT('Ctrl Pts',(3.59617582069531,3.65345148306281,44.5807927219821));
#36106=CARTESIAN_POINT('Ctrl Pts',(1.40994405243592,4.92871646997956,44.7197391072672));
#36107=CARTESIAN_POINT('Ctrl Pts',(-1.11996770763229,5.00258539220554,44.8586854925523));
#36108=CARTESIAN_POINT('Ctrl Pts',(-3.37688247046485,3.85705237883987,44.9976318778374));
#36109=CARTESIAN_POINT('Ctrl Pts',(-4.81066745181167,1.77134608152317,45.1365782631226));
#36110=CARTESIAN_POINT('Ctrl Pts',(-5.07183132980518,-0.746133523207451,
45.2755246484077));
#36111=CARTESIAN_POINT('Ctrl Pts',(-4.09671427390505,-3.0817398382131,45.4144710336929));
#36112=CARTESIAN_POINT('Ctrl Pts',(-2.12300530532106,-4.66615867132998,
45.5534174189779));
#36113=CARTESIAN_POINT('Ctrl Pts',(0.368195435139699,-5.11318104451468,
45.6923638042631));
#36114=CARTESIAN_POINT('Ctrl Pts',(2.7696469377403,-4.31384331110022,45.8313101895482));
#36115=CARTESIAN_POINT('Ctrl Pts',(4.49598495960815,-2.46298751832151,45.9702565748334));
#36116=CARTESIAN_POINT('Ctrl Pts',(5.12640710352584,-0.011767811352088,
46.1092029601185));
#36117=CARTESIAN_POINT('Ctrl Pts',(4.50724523145763,2.44232035080534,46.2481493454036));
#36118=CARTESIAN_POINT('Ctrl Pts',(2.78942274123745,4.30108231065426,46.3870957306888));
#36119=CARTESIAN_POINT('Ctrl Pts',(0.391666332192212,5.11143676053596,46.5260421159738));
#36120=CARTESIAN_POINT('Ctrl Pts',(-2.10156044784752,4.67585628049741,46.664988501259));
#36121=CARTESIAN_POINT('Ctrl Pts',(-4.08252273333974,3.10051550637416,46.803934886544));
#36122=CARTESIAN_POINT('Ctrl Pts',(-5.06835235565692,0.769410599168003,
46.9428812718293));
#36123=CARTESIAN_POINT('Ctrl Pts',(-4.81874905953264,-1.74924148531259,
47.0818276571143));
#36124=CARTESIAN_POINT('Ctrl Pts',(-3.39455473229958,-3.84150835555375,
47.2207740423995));
#36125=CARTESIAN_POINT('Ctrl Pts',(-1.14292293438725,-4.99739086165512,
47.3597204276846));
#36126=CARTESIAN_POINT('Ctrl Pts',(1.38730129989963,-4.93513762827236,47.4986668129698));
#36127=CARTESIAN_POINT('Ctrl Pts',(3.57936480620948,-3.66992313186164,47.6376131982548));
#36128=CARTESIAN_POINT('Ctrl Pts',(4.89894259229508,-1.510148944458,47.7765595835401));
#36129=CARTESIAN_POINT('Ctrl Pts',(5.0243818047371,1.01773066266865,47.915505968825));
#36130=CARTESIAN_POINT('Ctrl Pts',(3.92510615240954,3.29753389928866,48.0544523541103));
#36131=CARTESIAN_POINT('Ctrl Pts',(1.86906873270474,4.77354910373812,48.1933987393953));
#36132=CARTESIAN_POINT('Ctrl Pts',(-0.642562158693535,5.08599059227959,
48.3323451246805));
#36133=CARTESIAN_POINT('Ctrl Pts',(-2.99756603670477,4.15870048993547,48.4712915099656));
#36134=CARTESIAN_POINT('Ctrl Pts',(-4.62189956542536,2.21770765030908,48.6102378952508));
#36135=CARTESIAN_POINT('Ctrl Pts',(-5.11962615001036,-0.263858307003834,
48.7491842805358));
#36136=CARTESIAN_POINT('Ctrl Pts',(-4.3694193284947,-2.68111304807841,48.8881306658211));
#36137=CARTESIAN_POINT('Ctrl Pts',(-2.55415199717266,-4.44482430004468,
49.0270770511061));
#36138=CARTESIAN_POINT('Ctrl Pts',(-0.11629033496576,-5.12511086267891,
49.1660234363912));
#36139=CARTESIAN_POINT('Ctrl Pts',(2.34990065829377,-4.55608924149042,49.3049698216764));
#36140=CARTESIAN_POINT('Ctrl Pts',(4.24332623397428,-2.87657943442583,49.4439162069614));
#36141=CARTESIAN_POINT('Ctrl Pts',(5.10235796277362,-0.495737641055859,
49.5828625922466));
#36142=CARTESIAN_POINT('Ctrl Pts',(4.71779440725493,2.00564064112161,49.7218089775318));
#36143=CARTESIAN_POINT('Ctrl Pts',(3.18293456305578,4.01883138234242,49.8607609007809));
#36144=CARTESIAN_POINT('Ctrl Pts',(1.64272913283473,4.70685298774121,49.9533973622685));
#36145=CARTESIAN_POINT('Ctrl Pts',(0.836785021106394,4.84601823601536,49.9997183619944));
#36146=CARTESIAN_POINT('Ctrl Pts',(-2.29311987939507,4.72368461420244,-0.384448231563372));
#36147=CARTESIAN_POINT('Ctrl Pts',(-3.07862444090061,4.34236023028229,-0.338132769801664));
#36148=CARTESIAN_POINT('Ctrl Pts',(-4.45493794042212,3.18067190535823,-0.245501846278247));
#36149=CARTESIAN_POINT('Ctrl Pts',(-5.43361388965546,0.661144042220643,
-0.106555460993121));
#36150=CARTESIAN_POINT('Ctrl Pts',(-5.08774636704661,-2.01883410487796,
0.0323909242920052));
#36151=CARTESIAN_POINT('Ctrl Pts',(-3.50175917389135,-4.2070596791708,0.171337309577131));
#36152=CARTESIAN_POINT('Ctrl Pts',(-1.06218201400962,-5.36961982523882,
0.310283694862257));
#36153=CARTESIAN_POINT('Ctrl Pts',(1.63629588706826,-5.22340199091913,0.449230080147383));
#36154=CARTESIAN_POINT('Ctrl Pts',(3.93592505622498,-3.80391102861263,0.588176465432509));
#36155=CARTESIAN_POINT('Ctrl Pts',(5.27615256431546,-1.4572238740315,0.727122850717634));
#36156=CARTESIAN_POINT('Ctrl Pts',(5.33029639345207,1.24468005167587,0.866069236002761));
#36157=CARTESIAN_POINT('Ctrl Pts',(4.08515656621609,3.64318159744485,1.00501562128788));
#36158=CARTESIAN_POINT('Ctrl Pts',(1.84424244666043,5.1536449711362,1.14396200657301));
#36159=CARTESIAN_POINT('Ctrl Pts',(-0.846213980258722,5.4078833517554,1.28290839185814));
#36160=CARTESIAN_POINT('Ctrl Pts',(-3.33040197159187,4.34392749144419,1.42185477714326));
#36161=CARTESIAN_POINT('Ctrl Pts',(-5.00279005600775,2.221119994778,1.56080116242839));
#36162=CARTESIAN_POINT('Ctrl Pts',(-5.45572629105949,-0.443094936973425,
1.69974754771351));
#36163=CARTESIAN_POINT('Ctrl Pts',(-4.57880553997945,-2.99930366380419,
1.83869393299864));
#36164=CARTESIAN_POINT('Ctrl Pts',(-2.58578102761624,-4.82441902718766,
1.97764031828376));
#36165=CARTESIAN_POINT('Ctrl Pts',(0.0375388471149513,-5.47356131035378,
2.11658670356889));
#36166=CARTESIAN_POINT('Ctrl Pts',(2.65170846647585,-4.78849921548164,2.25553308885402));
#36167=CARTESIAN_POINT('Ctrl Pts',(4.61951261923543,-2.93621962894386,2.39447947413914));
#36168=CARTESIAN_POINT('Ctrl Pts',(5.46129049050343,-0.368223740149896,
2.53342585942427));
#36169=CARTESIAN_POINT('Ctrl Pts',(4.97185506423708,2.28952828394974,2.6723722447094));
#36170=CARTESIAN_POINT('Ctrl Pts',(3.27050835352976,4.38919783729295,2.81131862999452));
#36171=CARTESIAN_POINT('Ctrl Pts',(0.771961014684566,5.4189813374193,2.95026501527965));
#36172=CARTESIAN_POINT('Ctrl Pts',(-1.91475517717252,5.12786458050685,3.08921140056477));
#36173=CARTESIAN_POINT('Ctrl Pts',(-4.13474147116859,3.58680854112624,3.2281577858499));
#36174=CARTESIAN_POINT('Ctrl Pts',(-5.34686655783527,1.17145232805873,3.36710417113502));
#36175=CARTESIAN_POINT('Ctrl Pts',(-5.255669678202,-1.5294504823136,3.50605055642015));
#36176=CARTESIAN_POINT('Ctrl Pts',(-3.8833804681057,-3.85754308908115,3.64499694170528));
#36177=CARTESIAN_POINT('Ctrl Pts',(-1.56450038785265,-5.24534279915276,
3.7839433269904));
#36178=CARTESIAN_POINT('Ctrl Pts',(1.13573346282413,-5.35456740041784,3.92288971227553));
#36179=CARTESIAN_POINT('Ctrl Pts',(3.55912734490322,-4.15859292152604,4.06183609756065));
#36180=CARTESIAN_POINT('Ctrl Pts',(5.11496846513371,-1.9489433406052,4.20078248284578));
#36181=CARTESIAN_POINT('Ctrl Pts',(5.42401378721696,0.735769651645315,4.33972886813091));
#36182=CARTESIAN_POINT('Ctrl Pts',(4.41093217047509,3.24113559291651,4.47867525341603));
#36183=CARTESIAN_POINT('Ctrl Pts',(2.32266666285525,4.9564606441959,4.61762163870116));
#36184=CARTESIAN_POINT('Ctrl Pts',(-0.331758940468846,5.46362686771537,
4.75656802398628));
#36185=CARTESIAN_POINT('Ctrl Pts',(-2.90531685989736,4.63901029184008,4.89551440927141));
#36186=CARTESIAN_POINT('Ctrl Pts',(-4.77069116531186,2.68361479154843,5.03446079455654));
#36187=CARTESIAN_POINT('Ctrl Pts',(-5.47318876098439,0.0740765201418065,
5.17340717984166));
#36188=CARTESIAN_POINT('Ctrl Pts',(-4.84157280421231,-2.55351822506004,
5.31235356512679));
#36189=CARTESIAN_POINT('Ctrl Pts',(-3.02980243009377,-4.55868180275834,
5.45129995041191));
#36190=CARTESIAN_POINT('Ctrl Pts',(-0.479504543086973,-5.45264687444191,
5.59024633569704));
#36191=CARTESIAN_POINT('Ctrl Pts',(2.18767466070378,-5.0175055678212,5.72919272098216));
#36192=CARTESIAN_POINT('Ctrl Pts',(4.32159865612501,-3.35932546794452,5.86813910626729));
#36193=CARTESIAN_POINT('Ctrl Pts',(5.40211419312394,-0.88229518226665,6.00708549155243));
#36194=CARTESIAN_POINT('Ctrl Pts',(5.16584091255546,1.80979838942637,6.14603187683754));
#36195=CARTESIAN_POINT('Ctrl Pts',(3.6703714536382,4.06074573650209,6.28497826212267));
#36196=CARTESIAN_POINT('Ctrl Pts',(1.28023299778984,5.3218686582414,6.42392464740779));
#36197=CARTESIAN_POINT('Ctrl Pts',(-1.42196781644337,5.28576296036829,6.56287103269293));
#36198=CARTESIAN_POINT('Ctrl Pts',(-3.7775577941236,3.96122956369082,6.70181741797804));
#36199=CARTESIAN_POINT('Ctrl Pts',(-5.21235163844033,1.67112924139653,6.84076380326317));
#36200=CARTESIAN_POINT('Ctrl Pts',(-5.37661211279168,-1.02631609788793,
6.9797101885483));
#36201=CARTESIAN_POINT('Ctrl Pts',(-4.23030001251415,-3.47359242691553,
7.11865657383343));
#36202=CARTESIAN_POINT('Ctrl Pts',(-2.05283389506973,-5.07416550217421,
7.25760295911855));
#36203=CARTESIAN_POINT('Ctrl Pts',(0.62501940796803,-5.43788867887764,7.39654934440369));
#36204=CARTESIAN_POINT('Ctrl Pts',(3.15052151335387,-4.47610285159943,7.5354957296888));
#36205=CARTESIAN_POINT('Ctrl Pts',(4.9080703045409,-2.42324749662225,7.67444211497394));
#36206=CARTESIAN_POINT('Ctrl Pts',(5.46925562361168,0.220284969514861,7.81338850025905));
#36207=CARTESIAN_POINT('Ctrl Pts',(4.69728610956982,2.81012201675383,7.95233488554419));
#36208=CARTESIAN_POINT('Ctrl Pts',(2.78033268721492,4.71497960680705,8.09128127082931));
#36209=CARTESIAN_POINT('Ctrl Pts',(0.185661086243624,5.47054042168203,8.23022765611444));
#36210=CARTESIAN_POINT('Ctrl Pts',(-2.45426621156841,4.89263322832968,8.36917404139956));
#36211=CARTESIAN_POINT('Ctrl Pts',(-4.49595545161403,3.12212541729256,8.50812042668468));
#36212=CARTESIAN_POINT('Ctrl Pts',(-5.44173600640782,0.590585963909393,
8.64706681196982));
#36213=CARTESIAN_POINT('Ctrl Pts',(-5.06106975441018,-2.0849113854542,8.78601319725493));
#36214=CARTESIAN_POINT('Ctrl Pts',(-3.44674574930196,-4.25220252150235,
8.92495958254008));
#36215=CARTESIAN_POINT('Ctrl Pts',(-0.99226248479567,-5.38300080860752,
9.06390596782517));
#36216=CARTESIAN_POINT('Ctrl Pts',(1.70408907374516,-5.20166924870704,9.20285235311033));
#36217=CARTESIAN_POINT('Ctrl Pts',(3.98506151288443,-3.75240819777504,9.34179873839543));
#36218=CARTESIAN_POINT('Ctrl Pts',(5.29465788519347,-1.38848133691482,9.48074512368058));
#36219=CARTESIAN_POINT('Ctrl Pts',(5.31365838210577,1.31389388554757,9.61969150896568));
#36220=CARTESIAN_POINT('Ctrl Pts',(4.03743154990377,3.69600176191026,9.75863789425084));
#36221=CARTESIAN_POINT('Ctrl Pts',(1.7770632266955,5.17719314228556,9.89758427953593));
#36222=CARTESIAN_POINT('Ctrl Pts',(-0.916471982914659,5.39642118896724,
10.0365306648211));
#36223=CARTESIAN_POINT('Ctrl Pts',(-3.38661316278514,4.30024811259217,10.1754770501062));
#36224=CARTESIAN_POINT('Ctrl Pts',(-5.0312526626174,2.15587086559178,10.3144234353914));
#36225=CARTESIAN_POINT('Ctrl Pts',(-5.44950245507848,-0.514009276468483,
10.4533698206764));
#36226=CARTESIAN_POINT('Ctrl Pts',(-4.53941233512393,-3.05859742299095,
10.5923162059616));
#36227=CARTESIAN_POINT('Ctrl Pts',(-2.52282072565491,-4.85763915193463,
10.7312625912467));
#36228=CARTESIAN_POINT('Ctrl Pts',(0.108719402395609,-5.47261022143409,
10.8702089765319));
#36229=CARTESIAN_POINT('Ctrl Pts',(2.7137587035089,-4.75360876001925,11.0091553618169));
#36230=CARTESIAN_POINT('Ctrl Pts',(4.65730752393128,-2.87589449940974,11.1481017471021));
#36231=CARTESIAN_POINT('Ctrl Pts',(5.46561739007695,-0.297168453054067,
11.2870481323872));
#36232=CARTESIAN_POINT('Ctrl Pts',(4.94165925834944,2.35399369552495,11.4259945176723));
#36233=CARTESIAN_POINT('Ctrl Pts',(3.21315020100368,4.43135964800785,11.5649409029575));
#36234=CARTESIAN_POINT('Ctrl Pts',(0.701421814597499,5.42856242316589,11.7038872882426));
#36235=CARTESIAN_POINT('Ctrl Pts',(-1.98128118819784,5.10252950971334,11.8428336735277));
#36236=CARTESIAN_POINT('Ctrl Pts',(-4.1810382887395,3.53273284756947,11.9817800588128));
#36237=CARTESIAN_POINT('Ctrl Pts',(-5.3616491314251,1.10181719703885,12.120726444098));
#36238=CARTESIAN_POINT('Ctrl Pts',(-5.23533469123401,-1.59767118486996,
12.2596728293831));
#36239=CARTESIAN_POINT('Ctrl Pts',(-3.83288466205176,-3.90772027038919,
12.3986192146682));
#36240=CARTESIAN_POINT('Ctrl Pts',(-1.49615233494258,-5.26524555313881,
12.5375655999534));
#36241=CARTESIAN_POINT('Ctrl Pts',(1.2052736275839,-5.33934434428544,12.6765119852385));
#36242=CARTESIAN_POINT('Ctrl Pts',(3.61290890406165,-4.1119547413796,12.8154583705236));
#36243=CARTESIAN_POINT('Ctrl Pts',(5.13988192985733,-1.88225829559289,12.9544047558087));
#36244=CARTESIAN_POINT('Ctrl Pts',(5.4139863921806,0.806246791922473,13.0933511410939));
#36245=CARTESIAN_POINT('Ctrl Pts',(4.36840813680796,3.29822571915148,13.232297526379));
#36246=CARTESIAN_POINT('Ctrl Pts',(2.25801140861569,4.98624778994821,13.3712439116641));
#36247=CARTESIAN_POINT('Ctrl Pts',(-0.402785416003514,5.45885028672311,
13.5101902969492));
#36248=CARTESIAN_POINT('Ctrl Pts',(-2.96540154456344,4.60083429648395,13.6491366822344));
#36249=CARTESIAN_POINT('Ctrl Pts',(-4.80518815603382,2.6213449466475,13.7880830675195));
#36250=CARTESIAN_POINT('Ctrl Pts',(-5.47368926631531,0.00289137107776702,
13.9270294528046));
#36251=CARTESIAN_POINT('Ctrl Pts',(-4.80795482380209,-2.61626698876096,
14.0659758380897));
#36252=CARTESIAN_POINT('Ctrl Pts',(-2.97026049280476,-4.59769889717513,
14.2049222233749));
#36253=CARTESIAN_POINT('Ctrl Pts',(-0.408552254962224,-5.45842171320313,
14.34386860866));
#36254=CARTESIAN_POINT('Ctrl Pts',(2.25274237100424,-4.9886305088756,14.4828149939451));
#36255=CARTESIAN_POINT('Ctrl Pts',(4.36492125136605,-3.30283893242996,14.6217613792302));
#36256=CARTESIAN_POINT('Ctrl Pts',(5.41313160239223,-0.811966008761832,
14.7607077645154));
#36257=CARTESIAN_POINT('Ctrl Pts',(5.14186759444916,1.87682715915871,14.8996541498005));
#36258=CARTESIAN_POINT('Ctrl Pts',(3.61725100865776,4.10813554846558,15.0386005350856));
#36259=CARTESIAN_POINT('Ctrl Pts',(1.21091376531386,5.33806803976639,15.1775469203707));
#36260=CARTESIAN_POINT('Ctrl Pts',(-1.49058897216811,5.26682324178939,15.3164933056559));
#36261=CARTESIAN_POINT('Ctrl Pts',(-3.82875416809305,3.91176738374259,15.455439690941));
#36262=CARTESIAN_POINT('Ctrl Pts',(-5.23364389194872,1.60320122145348,15.5943860762261));
#36263=CARTESIAN_POINT('Ctrl Pts',(-5.36281016648893,-1.09615220768151,
15.7333324615112));
#36264=CARTESIAN_POINT('Ctrl Pts',(-4.18476815080863,-3.52831377121986,
15.8722788467964));
#36265=CARTESIAN_POINT('Ctrl Pts',(-1.98667070717921,-5.10043351544144,
16.0112252320815));
#36266=CARTESIAN_POINT('Ctrl Pts',(0.695686357383897,-5.42930041868675,
16.1501716173666));
#36267=CARTESIAN_POINT('Ctrl Pts',(3.20846684818567,-4.43475174370513,16.2891180026517));
#36268=CARTESIAN_POINT('Ctrl Pts',(4.93916959753494,-2.35921305332702,16.4280643879369));
#36269=CARTESIAN_POINT('Ctrl Pts',(5.46592828691201,0.291394074299996,16.567010773222));
#36270=CARTESIAN_POINT('Ctrl Pts',(4.66034319596094,2.87097262962618,16.7059571585071));
#36271=CARTESIAN_POINT('Ctrl Pts',(2.71877919247985,4.75073912636138,16.8449035437923));
#36272=CARTESIAN_POINT('Ctrl Pts',(0.114500942297094,5.47249230958027,16.9838499290774));
#36273=CARTESIAN_POINT('Ctrl Pts',(-2.51768741030621,4.8603017034118,17.1227963143625));
#36274=CARTESIAN_POINT('Ctrl Pts',(-4.53617851225878,3.06339142930247,17.2617426996476));
#36275=CARTESIAN_POINT('Ctrl Pts',(-5.44895638307774,0.519766177736342,
17.4006890849328));
#36276=CARTESIAN_POINT('Ctrl Pts',(-5.03352744890496,-2.15055433907689,
17.5396354702179));
#36277=CARTESIAN_POINT('Ctrl Pts',(-3.39115431831494,-4.29666788727916,
17.678581855503));
#36278=CARTESIAN_POINT('Ctrl Pts',(-0.92217258128593,-5.39544996033942,
17.8175282407881));
#36279=CARTESIAN_POINT('Ctrl Pts',(1.77159273111631,-5.1790676515429,17.9564746260733));
#36280=CARTESIAN_POINT('Ctrl Pts',(4.03352461419432,-3.70026508927276,18.0954210113584));
#36281=CARTESIAN_POINT('Ctrl Pts',(5.31226733882865,-1.31950682643796,18.2343673966435));
#36282=CARTESIAN_POINT('Ctrl Pts',(5.2961218071944,1.382886961238,18.3733137819286));
#36283=CARTESIAN_POINT('Ctrl Pts',(3.989023562812,3.74819604070184,18.5122601672138));
#36284=CARTESIAN_POINT('Ctrl Pts',(1.70958348470646,5.19986604183425,18.6512065524989));
#36285=CARTESIAN_POINT('Ctrl Pts',(-0.986574999356629,5.38404609144894,
18.790152937784));
#36286=CARTESIAN_POINT('Ctrl Pts',(-3.44225153868445,4.25584150182154,18.9290993230691));
#36287=CARTESIAN_POINT('Ctrl Pts',(-5.05886430198859,2.0902570459797,19.0680457083543));
#36288=CARTESIAN_POINT('Ctrl Pts',(-5.44235690079696,-0.584836651168256,
19.2069920936394));
#36289=CARTESIAN_POINT('Ctrl Pts',(-4.49925134710757,-3.11737387230869,
19.3459384789245));
#36290=CARTESIAN_POINT('Ctrl Pts',(-2.45943371931255,-4.89003766084787,
19.4848848642096));
#36291=CARTESIAN_POINT('Ctrl Pts',(0.179881568724695,-5.47073351255893,
19.6238312494948));
#36292=CARTESIAN_POINT('Ctrl Pts',(2.77534994244003,-4.71791428930203,19.7627776347799));
#36293=CARTESIAN_POINT('Ctrl Pts',(4.69431470323778,-2.81508294925169,19.901724020065));
#36294=CARTESIAN_POINT('Ctrl Pts',(5.46901984893268,-0.226062903154081,
20.0406704053501));
#36295=CARTESIAN_POINT('Ctrl Pts',(4.91062763261785,2.41806095828293,20.1796167906353));
#36296=CARTESIAN_POINT('Ctrl Pts',(3.15524858435129,4.47277194982611,20.3185631759204));
#36297=CARTESIAN_POINT('Ctrl Pts',(0.630763977781736,5.43722533545695,20.4575095612055));
#36298=CARTESIAN_POINT('Ctrl Pts',(-2.04747209030348,5.07633140994857,20.5964559464906));
#36299=CARTESIAN_POINT('Ctrl Pts',(-4.22662793601492,3.47805963644969,20.7354023317758));
#36300=CARTESIAN_POINT('Ctrl Pts',(-5.37552484916865,1.03199570743896,20.8743487170609));
#36301=CARTESIAN_POINT('Ctrl Pts',(-5.21411421292796,-1.66562166134591,
21.013295102346));
#36302=CARTESIAN_POINT('Ctrl Pts',(-3.78174057152866,-3.9572365097194,21.1522414876312));
#36303=CARTESIAN_POINT('Ctrl Pts',(-1.4275512265908,-5.28425775673948,21.2911878729163));
#36304=CARTESIAN_POINT('Ctrl Pts',(1.27460993539455,-5.3232182048828,21.4301342582014));
#36305=CARTESIAN_POINT('Ctrl Pts',(3.66607938489734,-4.06462107555339,21.5690806434865));
#36306=CARTESIAN_POINT('Ctrl Pts',(5.16392604788226,-1.81525489014774,21.7080270287717));
#36307=CARTESIAN_POINT('Ctrl Pts',(5.40304328910642,0.876587565645492,21.8469734140568));
#36308=CARTESIAN_POINT('Ctrl Pts',(4.32514524157863,3.35475799178598,21.9859197993419));
#36309=CARTESIAN_POINT('Ctrl Pts',(2.19297424000723,5.01519157429372,22.124866184627));
#36310=CARTESIAN_POINT('Ctrl Pts',(-0.47374376542617,5.45315040952677,22.2638125699122));
#36311=CARTESIAN_POINT('Ctrl Pts',(-3.02498466867256,4.56188012758973,22.4027589551973));
#36312=CARTESIAN_POINT('Ctrl Pts',(-4.83887240931995,2.55863173405716,22.5417053404824));
#36313=CARTESIAN_POINT('Ctrl Pts',(-5.47326396561445,-0.0682942670254661,
22.6806517257675));
#36314=CARTESIAN_POINT('Ctrl Pts',(-4.77352363800884,-2.67857324364538,
22.8195981110527));
#36315=CARTESIAN_POINT('Ctrl Pts',(-2.91021617312862,-4.63593834836731,
22.9585444963378));
#36316=CARTESIAN_POINT('Ctrl Pts',(-0.337530865336959,-5.4632733282481,
23.0974908816229));
#36317=CARTESIAN_POINT('Ctrl Pts',(2.31742905812749,-4.95891168551614,23.2364372669081));
#36318=CARTESIAN_POINT('Ctrl Pts',(4.4075055748079,-3.2457937630477,23.3753836521932));
#36319=CARTESIAN_POINT('Ctrl Pts',(5.42323344819965,-0.741499501369069,
23.5143300374783));
#36320=CARTESIAN_POINT('Ctrl Pts',(5.11702459379388,1.94353848706702,23.6532764227634));
#36321=CARTESIAN_POINT('Ctrl Pts',(3.56351875094202,4.15483052071765,23.7922228080486));
#36322=CARTESIAN_POINT('Ctrl Pts',(1.14138972192999,5.35336455389269,23.9311691933337));
#36323=CARTESIAN_POINT('Ctrl Pts',(-1.55895801342421,5.24699270597763,24.0701155786188));
#36324=CARTESIAN_POINT('Ctrl Pts',(-3.87930295621489,3.86164357730029,24.2090619639039));
#36325=CARTESIAN_POINT('Ctrl Pts',(-5.25405094009607,1.53500204008914,24.348008349189));
#36326=CARTESIAN_POINT('Ctrl Pts',(-5.34810116796638,-1.16580291704848,
24.4869547344742));
#36327=CARTESIAN_POINT('Ctrl Pts',(-4.13852848794609,-3.58243834540955,
24.6259011197593));
#36328=CARTESIAN_POINT('Ctrl Pts',(-1.92017149880326,-5.12583885421554,
24.7648475050444));
#36329=CARTESIAN_POINT('Ctrl Pts',(0.766235640159479,-5.41979386028211,
24.9037938903296));
#36330=CARTESIAN_POINT('Ctrl Pts',(3.26586951100659,-4.39265055305789,25.0427402756147));
#36331=CARTESIAN_POINT('Ctrl Pts',(4.96943349180918,-2.29477957867138,25.1816866608998));
#36332=CARTESIAN_POINT('Ctrl Pts',(5.46167645685312,0.362453893424401,25.3206330461849));
#36333=CARTESIAN_POINT('Ctrl Pts',(4.62261204362843,2.93133765341074,25.4595794314701));
#36334=CARTESIAN_POINT('Ctrl Pts',(2.65676585027213,4.78569511785174,25.5985258167552));
#36335=CARTESIAN_POINT('Ctrl Pts',(0.0433214319493474,5.47351859389697,
25.7374722020403));
#36336=CARTESIAN_POINT('Ctrl Pts',(-2.58068277372936,4.82714811929141,25.8764185873254));
#36337=CARTESIAN_POINT('Ctrl Pts',(-4.5756343350821,3.00413930699294,26.0153649726106));
#36338=CARTESIAN_POINT('Ctrl Pts',(-5.45525513697349,0.448858479619654,
26.1543113578957));
#36339=CARTESIAN_POINT('Ctrl Pts',(-5.00513378523042,-2.21583355334896,
26.2932577431808));
#36340=CARTESIAN_POINT('Ctrl Pts',(-3.33498931601805,-4.34040652545905,
26.4322041284659));
#36341=CARTESIAN_POINT('Ctrl Pts',(-0.851926703825804,-5.40698653923892,
26.5711505137511));
#36342=CARTESIAN_POINT('Ctrl Pts',(1.83879674574985,-5.15559007990567,26.7100968990362));
#36343=CARTESIAN_POINT('Ctrl Pts',(4.08130549529846,-3.64749612724247,26.8490432843213));
#36344=CARTESIAN_POINT('Ctrl Pts',(5.32897828893076,-1.25030913789616,26.9879896696064));
#36345=CARTESIAN_POINT('Ctrl Pts',(5.27768945956457,1.45164613890688,27.1269360548916));
#36346=CARTESIAN_POINT('Ctrl Pts',(3.93994088231041,3.79975635904478,27.2658824401767));
#36347=CARTESIAN_POINT('Ctrl Pts',(1.64181458806782,5.22165944912245,27.4048288254618));
#36348=CARTESIAN_POINT('Ctrl Pts',(-1.05651114898524,5.37076034991994,27.5437752107469));
#36349=CARTESIAN_POINT('Ctrl Pts',(-3.49730770081858,4.21071506872612,27.6827215960321));
#36350=CARTESIAN_POINT('Ctrl Pts',(-5.08562029777881,2.02428968554951,27.8216679813172));
#36351=CARTESIAN_POINT('Ctrl Pts',(-5.43429083996117,-0.655565108068201,
27.9606143666024));
#36352=CARTESIAN_POINT('Ctrl Pts',(-4.45832936703756,-3.1756230568524,28.0995607518874));
#36353=CARTESIAN_POINT('Ctrl Pts',(-2.3956307305383,-4.92160908109355,28.2385071371726));
#36354=CARTESIAN_POINT('Ctrl Pts',(0.251013310337818,-5.46793149758073,
28.3774535224577));
#36355=CARTESIAN_POINT('Ctrl Pts',(2.83647176566412,-4.68142184243126,28.5163999077429));
#36356=CARTESIAN_POINT('Ctrl Pts',(4.7305278979654,-2.75379526304575,28.6553462930279));
#36357=CARTESIAN_POINT('Ctrl Pts',(5.47149729153014,-0.15491911754329,28.7942926783131));
#36358=CARTESIAN_POINT('Ctrl Pts',(4.87876543568261,2.48171923629383,28.9332390635982));
#36359=CARTESIAN_POINT('Ctrl Pts',(3.0968132968913,4.51342773824943,29.0721854488833));
#36360=CARTESIAN_POINT('Ctrl Pts',(0.559999455133565,5.44496860913378,29.2111318341684));
#36361=CARTESIAN_POINT('Ctrl Pts',(-2.11331668813089,5.04927471226013,29.3500782194536));
#36362=CARTESIAN_POINT('Ctrl Pts',(-4.27150270207461,3.42279815507304,29.4890246047387));
#36363=CARTESIAN_POINT('Ctrl Pts',(-5.38849136416299,0.961999668681364,
29.6279709900239));
#36364=CARTESIAN_POINT('Ctrl Pts',(-5.1920118324616,-1.73329041876452,29.7669173753089));
#36365=CARTESIAN_POINT('Ctrl Pts',(-3.72995684691932,-4.00608343202207,
29.9058637605941));
#36366=CARTESIAN_POINT('Ctrl Pts',(-1.35870866581594,-5.30237619427732,
30.0448101458792));
#36367=CARTESIAN_POINT('Ctrl Pts',(1.34373065888744,-5.30619170974514,30.1837565311644));
#36368=CARTESIAN_POINT('Ctrl Pts',(3.71862979428907,-4.0165999299442,30.3227029164495));
#36369=CARTESIAN_POINT('Ctrl Pts',(5.18709675244689,-1.74794445705719,30.4616493017346));
#36370=CARTESIAN_POINT('Ctrl Pts',(5.39118632888328,0.946780075553036,30.6005956870197));
#36371=CARTESIAN_POINT('Ctrl Pts',(4.28115080216432,3.41072284909372,30.7395420723048));
#36372=CARTESIAN_POINT('Ctrl Pts',(2.12756615725283,5.04328710175364,30.87848845759));
#36373=CARTESIAN_POINT('Ctrl Pts',(-0.544621987020308,5.44652820018919,
31.0174348428751));
#36374=CARTESIAN_POINT('Ctrl Pts',(-3.08405615448515,4.52215437376749,31.1563812281602));
#36375=CARTESIAN_POINT('Ctrl Pts',(-4.87173822790043,2.49548576093229,31.2953276134453));
#36376=CARTESIAN_POINT('Ctrl Pts',(-5.4719129308161,-0.13946835400816,31.4342739987305));
#36377=CARTESIAN_POINT('Ctrl Pts',(-4.73828507043673,-2.74042645139009,
31.5732203840156));
#36378=CARTESIAN_POINT('Ctrl Pts',(-2.84967962681054,-4.67339368861035,
31.7121667693007));
#36379=CARTESIAN_POINT('Ctrl Pts',(-0.266452386590298,-5.46720089898684,
31.8511131545859));
#36380=CARTESIAN_POINT('Ctrl Pts',(2.38172378113,-4.92835412430985,31.990059539871));
#36381=CARTESIAN_POINT('Ctrl Pts',(4.44934442384521,-3.18819960827417,32.1290059251561));
#36382=CARTESIAN_POINT('Ctrl Pts',(5.43241802194542,-0.670907578616172,
32.2679523104412));
#36383=CARTESIAN_POINT('Ctrl Pts',(5.09131611247224,2.00992108976518,32.4068986957263));
#36384=CARTESIAN_POINT('Ctrl Pts',(3.50918376862985,4.20082275538816,32.5458450810115));
#36385=CARTESIAN_POINT('Ctrl Pts',(1.07167262676009,5.36775561340635,32.6847914662966));
#36386=CARTESIAN_POINT('Ctrl Pts',(-1.62706337644393,5.22627470702,32.8237378515817));
#36387=CARTESIAN_POINT('Ctrl Pts',(-3.92919560879436,3.81086662217839,32.9626842368669));
#36388=CARTESIAN_POINT('Ctrl Pts',(-5.27356933128557,1.46654323234143,33.101630622152));
#36389=CARTESIAN_POINT('Ctrl Pts',(-5.33248760506705,-1.23525644544303,
33.2405770074371));
#36390=CARTESIAN_POINT('Ctrl Pts',(-4.09158884478678,-3.63595699499023,
33.3795233927222));
#36391=CARTESIAN_POINT('Ctrl Pts',(-1.85334751745077,-5.15037722150147,
33.5184697780074));
#36392=CARTESIAN_POINT('Ctrl Pts',(0.83665532376664,-5.40937061157905,33.6574161632925));
#36393=CARTESIAN_POINT('Ctrl Pts',(3.32271979287475,-4.3498064005471,33.7963625485776));
#36394=CARTESIAN_POINT('Ctrl Pts',(4.9988568686048,-2.22995797077088,33.9353089338628));
#36395=CARTESIAN_POINT('Ctrl Pts',(5.4565008525788,0.433452408009289,34.0742553191479));
#36396=CARTESIAN_POINT('Ctrl Pts',(4.58409903432438,2.99120687811935,34.213201704433));
#36397=CARTESIAN_POINT('Ctrl Pts',(2.59430314937227,4.8198416689098,34.3521480897182));
#36398=CARTESIAN_POINT('Ctrl Pts',(-0.0278654056765308,5.473619101049,34.4910944750032));
#36399=CARTESIAN_POINT('Ctrl Pts',(-2.64324164696075,4.79317808348222,34.6300408602884));
#36400=CARTESIAN_POINT('Ctrl Pts',(-4.6143162466254,2.94437907211879,34.7689872455735));
#36401=CARTESIAN_POINT('Ctrl Pts',(-5.46063120273975,0.377874862708882,
34.9079336308586));
#36402=CARTESIAN_POINT('Ctrl Pts',(-4.97589356581932,-2.28073798710854,
35.0468800161437));
#36403=CARTESIAN_POINT('Ctrl Pts',(-3.2782602420183,-4.38341103819895,35.1858264014289));
#36404=CARTESIAN_POINT('Ctrl Pts',(-0.781536733626139,-5.41760859403806,
35.324772786714));
#36405=CARTESIAN_POINT('Ctrl Pts',(1.90568975092798,-5.13124050473276,35.4637191719991));
#36406=CARTESIAN_POINT('Ctrl Pts',(4.12839607465902,-3.59411023689345,35.6026655572843));
#36407=CARTESIAN_POINT('Ctrl Pts',(5.34478790905178,-1.18089997521211,35.7416119425694));
#36408=CARTESIAN_POINT('Ctrl Pts',(5.25836445681711,1.52015978880005,35.8805583278545));
#36409=CARTESIAN_POINT('Ctrl Pts',(3.89019181011998,3.85067399615672,36.0195047131396));
#36410=CARTESIAN_POINT('Ctrl Pts',(1.57376799904008,5.24256967806815,36.1584510984248));
#36411=CARTESIAN_POINT('Ctrl Pts',(-1.12626860297622,5.35656621149707,36.2973974837099));
#36412=CARTESIAN_POINT('Ctrl Pts',(-3.55177233712678,4.16487644587724,36.436343868995));
#36413=CARTESIAN_POINT('Ctrl Pts',(-5.11151612454633,1.9579799418546,36.5752902542801));
#36414=CARTESIAN_POINT('Ctrl Pts',(-5.42530563684426,-0.726182684335063,
36.7142366395653));
#36415=CARTESIAN_POINT('Ctrl Pts',(-4.4166533163547,-3.23333512450152,36.8531830248503));
#36416=CARTESIAN_POINT('Ctrl Pts',(-2.33142255080919,-4.95234807276109,
36.9921294101355));
#36417=CARTESIAN_POINT('Ctrl Pts',(0.32210259619121,-5.46420465042526,37.1310757954206));
#36418=CARTESIAN_POINT('Ctrl Pts',(2.89711383518983,-4.64413759164755,37.2700221807058));
#36419=CARTESIAN_POINT('Ctrl Pts',(4.76594098310544,-2.69204180683697,37.4089685659909));
#36420=CARTESIAN_POINT('Ctrl Pts',(5.47304929884092,-0.0837491293026769,
37.547914951276));
#36421=CARTESIAN_POINT('Ctrl Pts',(4.84607805663556,2.54495776255665,37.6868613365611));
#36422=CARTESIAN_POINT('Ctrl Pts',(3.03785422222122,4.55332013686002,37.8258077218463));
#36423=CARTESIAN_POINT('Ctrl Pts',(0.489140215586399,5.45179093451851,37.9647541071314));
#36424=CARTESIAN_POINT('Ctrl Pts',(-2.17880384489038,5.02136399294982,38.1037004924165));
#36425=CARTESIAN_POINT('Ctrl Pts',(-4.3156549969136,3.36695775022748,38.2426468777017));
#36426=CARTESIAN_POINT('Ctrl Pts',(-5.40054648328439,0.89184091971992,38.3815932629867));
#36427=CARTESIAN_POINT('Ctrl Pts',(-5.16903128817595,-1.80066601180235,
38.520539648272));
#36428=CARTESIAN_POINT('Ctrl Pts',(-3.67754224679271,-4.05425277545157,
38.659486033557));
#36429=CARTESIAN_POINT('Ctrl Pts',(-1.28963629647555,-5.3195978012454,38.7984324188422));
#36430=CARTESIAN_POINT('Ctrl Pts',(1.41262410715728,-5.28826773869103,38.9373788041273));
#36431=CARTESIAN_POINT('Ctrl Pts',(3.77055124399274,-3.96789942672782,39.0763251894124));
#36432=CARTESIAN_POINT('Ctrl Pts',(5.20939012451653,-1.68033838103866,39.2152715746975));
#36433=CARTESIAN_POINT('Ctrl Pts',(5.37841751696762,1.0168124494606,39.3542179599827));
#36434=CARTESIAN_POINT('Ctrl Pts',(4.23643225967382,3.46611082531952,39.4931643452678));
#36435=CARTESIAN_POINT('Ctrl Pts',(2.06179822331107,5.07052962032108,39.6321107305529));
#36436=CARTESIAN_POINT('Ctrl Pts',(-0.61540809262174,5.43898477877421,39.771057115838));
#36437=CARTESIAN_POINT('Ctrl Pts',(-3.14260601079868,4.48166375413128,39.9100035011232));
#36438=CARTESIAN_POINT('Ctrl Pts',(-4.90378005293337,2.43191770762393,40.0489498864083));
#36439=CARTESIAN_POINT('Ctrl Pts',(-5.4696363904309,-0.210618851664463,
40.1878962716934));
#36440=CARTESIAN_POINT('Ctrl Pts',(-4.70224508124829,-2.80181615029938,
40.3268426569785));
#36441=CARTESIAN_POINT('Ctrl Pts',(-2.78866109284938,-4.71005858280236,
40.4657890422636));
#36442=CARTESIAN_POINT('Ctrl Pts',(-0.195328840757133,-5.47020376111992,
40.6047354275488));
#36443=CARTESIAN_POINT('Ctrl Pts',(2.44561566536424,-4.89696299368569,40.7436818128338));
#36444=CARTESIAN_POINT('Ctrl Pts',(4.49043072196045,-3.13006620943965,40.8826281981191));
#36445=CARTESIAN_POINT('Ctrl Pts',(5.4406837701739,-0.600202180243085,41.0215745834041));
#36446=CARTESIAN_POINT('Ctrl Pts',(5.06474649875199,2.07596373946694,41.1605209686893));
#36447=CARTESIAN_POINT('Ctrl Pts',(3.45425525180338,4.24610447346635,41.2994673539744));
#36448=CARTESIAN_POINT('Ctrl Pts',(1.00177427157815,5.38123878423976,41.4384137392595));
#36449=CARTESIAN_POINT('Ctrl Pts',(-1.69489354205759,5.20467274910667,41.5773601245447));
#36450=CARTESIAN_POINT('Ctrl Pts',(-3.97842368711355,3.75944510666346,41.7163065098298));
#36451=CARTESIAN_POINT('Ctrl Pts',(-5.2921957642256,1.39783637716104,41.8552528951149));
#36452=CARTESIAN_POINT('Ctrl Pts',(-5.31597211862969,-1.30450104566994,
41.9941992804001));
#36453=CARTESIAN_POINT('Ctrl Pts',(-4.04395716058395,-3.6888606679521,42.1331456656852));
#36454=CARTESIAN_POINT('Ctrl Pts',(-1.7862100655618,-5.17404446694148,42.2720920509703));
#36455=CARTESIAN_POINT('Ctrl Pts',(0.906933497597219,-5.39803243553966,
42.4110384362554));
#36456=CARTESIAN_POINT('Ctrl Pts',(3.37900807827648,-4.30622653272497,42.5499848215406));
#36457=CARTESIAN_POINT('Ctrl Pts',(5.02743475132581,-2.16475919338935,42.6889312068257));
#36458=CARTESIAN_POINT('Ctrl Pts',(5.45040234947773,0.504377609544291,42.8278775921108));
#36459=CARTESIAN_POINT('Ctrl Pts',(4.54481068204241,3.05057017762177,42.9668239773959));
#36460=CARTESIAN_POINT('Ctrl Pts',(2.53140165456461,4.8531730040737,43.105770362681));
#36461=CARTESIAN_POINT('Ctrl Pts',(-0.0990475302177512,5.47279381403684,
43.2447167479662));
#36462=CARTESIAN_POINT('Ctrl Pts',(-2.70535344894986,4.75839734159067,43.3836631332513));
#36463=CARTESIAN_POINT('Ctrl Pts',(-4.65221770432746,2.88412083237583,43.5226095185365));
#36464=CARTESIAN_POINT('Ctrl Pts',(-5.46508367108224,0.306827332994467,
43.6615559038215));
#36465=CARTESIAN_POINT('Ctrl Pts',(-4.94581173628886,-2.34525666258288,
43.8005022891067));
#36466=CARTESIAN_POINT('Ctrl Pts',(-3.2209766913287,-4.42567415182356,43.9394486743917));
#36467=CARTESIAN_POINT('Ctrl Pts',(-0.711014576269677,-5.42731432814925,
44.078395059677));
#36468=CARTESIAN_POINT('Ctrl Pts',(1.97226043253588,-5.10602304445011,44.217341444962));
#36469=CARTESIAN_POINT('Ctrl Pts',(4.17478838749362,-3.54011644778115,44.3562878302472));
#36470=CARTESIAN_POINT('Ctrl Pts',(5.35969352519225,-1.11129107807733,44.4952342155323));
#36471=CARTESIAN_POINT('Ctrl Pts',(5.2381500675345,1.58841632269079,44.6341806008175));
#36472=CARTESIAN_POINT('Ctrl Pts',(3.83978476067387,3.90094033995637,44.7731269861025));
#36473=CARTESIAN_POINT('Ctrl Pts',(1.50545522685244,5.26259319196769,44.9120733713877));
#36474=CARTESIAN_POINT('Ctrl Pts',(-1.19583556272895,5.34146607694132,45.0510197566728));
#36475=CARTESIAN_POINT('Ctrl Pts',(-3.60563623559729,4.11833338630442,45.189966141958));
#36476=CARTESIAN_POINT('Ctrl Pts',(-5.13654740233609,1.89133903035833,45.328912527243));
#36477=CARTESIAN_POINT('Ctrl Pts',(-5.41540281118094,-0.796677435889682,
45.4678589125282));
#36478=CARTESIAN_POINT('Ctrl Pts',(-4.37423024404137,-3.29050031398198,
45.6068052978133));
#36479=CARTESIAN_POINT('Ctrl Pts',(-2.26682004013511,-4.982249436735,45.7457516830984));
#36480=CARTESIAN_POINT('Ctrl Pts',(0.393137402421516,-5.45955360144152,
45.8846980683836));
#36481=CARTESIAN_POINT('Ctrl Pts',(2.95726589417037,-4.60606784311644,46.0236444536686));
#36482=CARTESIAN_POINT('Ctrl Pts',(4.80054796897683,-2.62983302544764,46.1625908389539));
#36483=CARTESIAN_POINT('Ctrl Pts',(5.47367560836416,-0.0125649759491998,
46.3015372242389));
#36484=CARTESIAN_POINT('Ctrl Pts',(4.81257102413439,2.60776584107418,46.4404836095241));
#36485=CARTESIAN_POINT('Ctrl Pts',(2.97838133253723,4.59244239834222,46.5794299948092));
#36486=CARTESIAN_POINT('Ctrl Pts',(0.418198244080788,5.45769115773086,46.7183763800943));
#36487=CARTESIAN_POINT('Ctrl Pts',(-2.24392248422375,4.99260397270669,46.8573227653795));
#36488=CARTESIAN_POINT('Ctrl Pts',(-4.35907735277298,3.31054786673546,46.9962691506646));
#36489=CARTESIAN_POINT('Ctrl Pts',(-5.41168816746401,0.82153132680118,47.1352155359497));
#36490=CARTESIAN_POINT('Ctrl Pts',(-5.14517646713044,-1.8677370442759,47.2741619212348));
#36491=CARTESIAN_POINT('Ctrl Pts',(-3.62450563605566,-4.10173639363517,
47.41310830652));
#36492=CARTESIAN_POINT('Ctrl Pts',(-1.22034580201261,-5.3359196631282,47.5520546918051));
#36493=CARTESIAN_POINT('Ctrl Pts',(1.48127862913772,-5.26944932664737,47.6910010770902));
#36494=CARTESIAN_POINT('Ctrl Pts',(3.82183494941533,-3.91852779651975,47.8299474623754));
#36495=CARTESIAN_POINT('Ctrl Pts',(5.23080239877533,-1.61244810943541,47.9688938476604));
#36496=CARTESIAN_POINT('Ctrl Pts',(5.36473900264045,1.08667286690954,48.1078402329456));
#36497=CARTESIAN_POINT('Ctrl Pts',(4.190997198,3.52091250417398,48.2467866182307));
#36498=CARTESIAN_POINT('Ctrl Pts',(1.99568152235226,5.09691461618197,48.3857330035158));
#36499=CARTESIAN_POINT('Ctrl Pts',(-0.686090032233244,5.43052123780479,
48.5246793888009));
#36500=CARTESIAN_POINT('Ctrl Pts',(-3.20062448577036,4.44041547511814,48.6636257740861));
#36501=CARTESIAN_POINT('Ctrl Pts',(-4.9349921698918,2.36793762704299,48.8025721593712));
#36502=CARTESIAN_POINT('Ctrl Pts',(-5.46643530553421,-0.281732361465787,
48.9415185446563));
#36503=CARTESIAN_POINT('Ctrl Pts',(-4.66540864158968,-2.86273462059622,
49.0804649299415));
#36504=CARTESIAN_POINT('Ctrl Pts',(-2.72717308724132,-4.7459216295728,49.2194113152266));
#36505=CARTESIAN_POINT('Ctrl Pts',(-0.124167971278091,-5.47229155872411,
49.3583577005117));
#36506=CARTESIAN_POINT('Ctrl Pts',(2.50908553605409,-4.86472378159826,49.4973040857969));
#36507=CARTESIAN_POINT('Ctrl Pts',(4.53077386094875,-3.07144211682079,49.6362504710819));
#36508=CARTESIAN_POINT('Ctrl Pts',(5.44799735213535,-0.529319458871882,
49.7751968563671));
#36509=CARTESIAN_POINT('Ctrl Pts',(5.03738303470027,2.14150496336914,49.9141432416522));
#36510=CARTESIAN_POINT('Ctrl Pts',(3.39855008175896,4.29107147899482,50.0530951649014));
#36511=CARTESIAN_POINT('Ctrl Pts',(1.75400942686783,5.02570043128944,50.145731626389));
#36512=CARTESIAN_POINT('Ctrl Pts',(0.893469766832245,5.17429288788272,50.1920526261149));
#36513=CARTESIAN_POINT('Ctrl Pts',(-2.43860316501687,5.02337115222,-0.192113967442929));
#36514=CARTESIAN_POINT('Ctrl Pts',(-3.27394279424196,4.61785425888989,-0.14579850568122));
#36515=CARTESIAN_POINT('Ctrl Pts',(-4.73757427995125,3.38246449519804,-0.0531675821578035));
#36516=CARTESIAN_POINT('Ctrl Pts',(-5.77834074348035,0.703089257730629,
0.0857788031273231));
#36517=CARTESIAN_POINT('Ctrl Pts',(-5.41053021473772,-2.14691577271492,
0.224725188412448));
#36518=CARTESIAN_POINT('Ctrl Pts',(-3.72392262668397,-4.47396978292609,
0.363671573697576));
#36519=CARTESIAN_POINT('Ctrl Pts',(-1.1295704356595,-5.71028667904572,0.5026179589827));
#36520=CARTESIAN_POINT('Ctrl Pts',(1.74010803576541,-5.55479229048019,0.641564344267827));
#36521=CARTESIAN_POINT('Ctrl Pts',(4.18563346191538,-4.04524401762382,0.780510729552951));
#36522=CARTESIAN_POINT('Ctrl Pts',(5.61088953877353,-1.54967508819847,0.919457114838079));
#36523=CARTESIAN_POINT('Ctrl Pts',(5.66846843566637,1.3236467664529,1.05840350012321));
#36524=CARTESIAN_POINT('Ctrl Pts',(4.34433272393584,3.87431736739548,1.19734988540833));
#36525=CARTESIAN_POINT('Ctrl Pts',(1.96124742883955,5.48060964928763,1.33629627069346));
#36526=CARTESIAN_POINT('Ctrl Pts',(-0.899900658959379,5.75097777317752,
1.47524265597859));
#36527=CARTESIAN_POINT('Ctrl Pts',(-3.5416939435564,4.61952095240389,1.61418904126371));
#36528=CARTESIAN_POINT('Ctrl Pts',(-5.32018398781385,2.36203536405459,1.75313542654884));
#36529=CARTESIAN_POINT('Ctrl Pts',(-5.80185603046317,-0.471206379315615,
1.89208181183396));
#36530=CARTESIAN_POINT('Ctrl Pts',(-4.86930045922241,-3.18958963860582,
2.03102819711909));
#36531=CARTESIAN_POINT('Ctrl Pts',(-2.74983172691733,-5.13049649727467,
2.16997458240422));
#36532=CARTESIAN_POINT('Ctrl Pts',(0.0399204386165095,-5.8208225637395,
2.30892096768934));
#36533=CARTESIAN_POINT('Ctrl Pts',(2.81994182561266,-5.09229781115264,2.44786735297447));
#36534=CARTESIAN_POINT('Ctrl Pts',(4.91259013334905,-3.12250333908225,2.58681373825959));
#36535=CARTESIAN_POINT('Ctrl Pts',(5.80777324155042,-0.391585100383275,
2.72576012354472));
#36536=CARTESIAN_POINT('Ctrl Pts',(5.28728637547375,2.43478370660165,2.86470650882985));
#36537=CARTESIAN_POINT('Ctrl Pts',(3.47800047166986,4.66766340219916,3.00365289411497));
#36538=CARTESIAN_POINT('Ctrl Pts',(0.820936833959134,5.76277985261022,3.1425992794001));
#36539=CARTESIAN_POINT('Ctrl Pts',(-2.03623372560755,5.45319366342964,3.28154566468522));
#36540=CARTESIAN_POINT('Ctrl Pts',(-4.39706346306589,3.81436781360389,3.42049204997035));
#36541=CARTESIAN_POINT('Ctrl Pts',(-5.68608986735551,1.24577322822909,3.55943843525547));
#36542=CARTESIAN_POINT('Ctrl Pts',(-5.58910714904596,-1.62648399694239,
3.6983848205406));
#36543=CARTESIAN_POINT('Ctrl Pts',(-4.12975526730215,-4.10227867751238,
3.83733120582573));
#36544=CARTESIAN_POINT('Ctrl Pts',(-1.66375758710614,-5.57812509784119,
3.97627759111085));
#36545=CARTESIAN_POINT('Ctrl Pts',(1.20778823730278,-5.69427927745301,4.11522397639598));
#36546=CARTESIAN_POINT('Ctrl Pts',(3.78493042861267,-4.42242813015308,4.2541703616811));
#36547=CARTESIAN_POINT('Ctrl Pts',(5.43947937485367,-2.07259090182936,4.39311674696624));
#36548=CARTESIAN_POINT('Ctrl Pts',(5.76813157805406,0.782449368368389,4.53206313225135));
#36549=CARTESIAN_POINT('Ctrl Pts',(4.69077663503258,3.44676420371884,4.67100951753648));
#36550=CARTESIAN_POINT('Ctrl Pts',(2.47002449641317,5.2709152813267,4.80995590282161));
#36551=CARTESIAN_POINT('Ctrl Pts',(-0.35280685040481,5.81025784643955,4.94890228810673));
#36552=CARTESIAN_POINT('Ctrl Pts',(-3.08963999378505,4.93332480428855,5.08784867339187));
#36553=CARTESIAN_POINT('Ctrl Pts',(-5.07335995801337,2.85387239592652,5.22679505867698));
#36554=CARTESIAN_POINT('Ctrl Pts',(-5.82042637857731,0.0787761852724543,
5.36574144396212));
#36555=CARTESIAN_POINT('Ctrl Pts',(-5.14873856796628,-2.71552206298188,
5.50468782924723));
#36556=CARTESIAN_POINT('Ctrl Pts',(-3.22202334984397,-4.84790000400844,
5.64363421453237));
#36557=CARTESIAN_POINT('Ctrl Pts',(-0.509925934059868,-5.79858124523387,
5.78258059981748));
#36558=CARTESIAN_POINT('Ctrl Pts',(2.32646814479965,-5.33583310149757,5.92152698510262));
#36559=CARTESIAN_POINT('Ctrl Pts',(4.59577550020591,-3.57245244440173,6.06047337038773));
#36560=CARTESIAN_POINT('Ctrl Pts',(5.74484259959826,-0.938270974530154,
6.19941975567287));
#36561=CARTESIAN_POINT('Ctrl Pts',(5.49357934250451,1.9246181240476,6.33836614095799));
#36562=CARTESIAN_POINT('Ctrl Pts',(3.90323224008275,4.31837318857267,6.47731252624312));
#36563=CARTESIAN_POINT('Ctrl Pts',(1.36145531178806,5.65950601641247,6.61625891152824));
#36564=CARTESIAN_POINT('Ctrl Pts',(-1.51218226700198,5.62110965087584,6.75520529681338));
#36565=CARTESIAN_POINT('Ctrl Pts',(-4.01721884475313,4.21254337297139,6.89415168209848));
#36566=CARTESIAN_POINT('Ctrl Pts',(-5.5430408662431,1.7771513359767,7.03309806738364));
#36567=CARTESIAN_POINT('Ctrl Pts',(-5.71772258098449,-1.09142906444016,
7.17204445266874));
#36568=CARTESIAN_POINT('Ctrl Pts',(-4.49868456166763,-3.69396888595697,
7.31099083795388));
#36569=CARTESIAN_POINT('Ctrl Pts',(-2.18307262465992,-5.39608773383692,
7.449937223239));
#36570=CARTESIAN_POINT('Ctrl Pts',(0.664672754426577,-5.78288673979767,
7.58888360852413));
#36571=CARTESIAN_POINT('Ctrl Pts',(3.35040126028876,-4.7600819647208,7.72782999380925));
#36572=CARTESIAN_POINT('Ctrl Pts',(5.21945489475937,-2.57698651866424,7.86677637909439));
#36573=CARTESIAN_POINT('Ctrl Pts',(5.816243709659,0.234260593478593,8.0057227643795));
#36574=CARTESIAN_POINT('Ctrl Pts',(4.99529783711454,2.98840566763009,8.14466914966463));
#36575=CARTESIAN_POINT('Ctrl Pts',(2.95672640221087,5.01411386969561,8.28361553494976));
#36576=CARTESIAN_POINT('Ctrl Pts',(0.197440053876959,5.817610019667,8.42256192023489));
#36577=CARTESIAN_POINT('Ctrl Pts',(-2.60997316586149,5.20303843819049,8.56150830552));
#36578=CARTESIAN_POINT('Ctrl Pts',(-4.78119408086637,3.320203619794,8.70045469080513));
#36579=CARTESIAN_POINT('Ctrl Pts',(-5.78697815480668,0.628054736145685,
8.83940107609027));
#36580=CARTESIAN_POINT('Ctrl Pts',(-5.38216114751552,-2.21718521959242,
8.97834746137538));
#36581=CARTESIAN_POINT('Ctrl Pts',(-3.6654189642599,-4.52197663994948,9.11729384666053));
#36582=CARTESIAN_POINT('Ctrl Pts',(-1.05521497488759,-5.7245165972838,9.25624023194561));
#36583=CARTESIAN_POINT('Ctrl Pts',(1.81220225163365,-5.53168074955333,9.39518661723079));
#36584=CARTESIAN_POINT('Ctrl Pts',(4.23788730167498,-3.99047367289983,9.53413300251587));
#36585=CARTESIAN_POINT('Ctrl Pts',(5.63056889983452,-1.47657129188572,9.67307938780103));
#36586=CARTESIAN_POINT('Ctrl Pts',(5.65077485257319,1.3972517601818,9.81202577308613));
#36587=CARTESIAN_POINT('Ctrl Pts',(4.29357987107567,3.93048862185081,9.95097215837128));
#36588=CARTESIAN_POINT('Ctrl Pts',(1.8898061318093,5.5056517961074,10.0899185436564));
#36589=CARTESIAN_POINT('Ctrl Pts',(-0.974616067073906,5.73878841199136,
10.2288649289416));
#36590=CARTESIAN_POINT('Ctrl Pts',(-3.60147136295125,4.5730704059359,10.3678113142267));
#36591=CARTESIAN_POINT('Ctrl Pts',(-5.35045235851118,2.29264660929394,10.5067576995118));
#36592=CARTESIAN_POINT('Ctrl Pts',(-5.79523733326456,-0.546619764499533,
10.6457040847969));
#36593=CARTESIAN_POINT('Ctrl Pts',(-4.82740801613472,-3.25264519453983,
10.7846504700821));
#36594=CARTESIAN_POINT('Ctrl Pts',(-2.68287701032666,-5.16582421916052,
10.9235968553672));
#36595=CARTESIAN_POINT('Ctrl Pts',(0.115616929216404,-5.81981113452004,
11.0625432406523));
#36596=CARTESIAN_POINT('Ctrl Pts',(2.88592873967612,-5.05519378711798,11.2014896259374));
#36597=CARTESIAN_POINT('Ctrl Pts',(4.95278287470592,-3.05835097917565,11.3404360112226));
#36598=CARTESIAN_POINT('Ctrl Pts',(5.81237465427617,-0.316021825405791,
11.4793823965077));
#36599=CARTESIAN_POINT('Ctrl Pts',(5.25517484547065,2.50333902205377,11.6183287817928));
#36600=CARTESIAN_POINT('Ctrl Pts',(3.41700332383366,4.71250010087157,11.757275167078));
#36601=CARTESIAN_POINT('Ctrl Pts',(0.745922388296798,5.77296879486129,11.8962215523631));
#36602=CARTESIAN_POINT('Ctrl Pts',(-2.10698037191245,5.42625125000498,12.0351679376482));
#36603=CARTESIAN_POINT('Ctrl Pts',(-4.44629750742316,3.75686137504265,12.1741143229333));
#36604=CARTESIAN_POINT('Ctrl Pts',(-5.70181029744169,1.17172020883517,12.3130607082185));
#36605=CARTESIAN_POINT('Ctrl Pts',(-5.56748204168621,-1.69903285174431,
12.4520070935035));
#36606=CARTESIAN_POINT('Ctrl Pts',(-4.07605583642212,-4.15563926901433,
12.5909534787887));
#36607=CARTESIAN_POINT('Ctrl Pts',(-1.5910733024131,-5.59929054989586,12.7298998640738));
#36608=CARTESIAN_POINT('Ctrl Pts',(1.28174026545566,-5.67809041912107,12.868846249359));
#36609=CARTESIAN_POINT('Ctrl Pts',(3.84212407189394,-4.37283106602324,13.0077926346441));
#36610=CARTESIAN_POINT('Ctrl Pts',(5.46597343409255,-2.00167513188312,13.1467390199292));
#36611=CARTESIAN_POINT('Ctrl Pts',(5.75746801114147,0.857397816936438,13.2856854052143));
#36612=CARTESIAN_POINT('Ctrl Pts',(4.64555473275797,3.50747632076895,13.4246317904995));
#36613=CARTESIAN_POINT('Ctrl Pts',(2.40126729403563,5.30259222441247,13.5635781757846));
#36614=CARTESIAN_POINT('Ctrl Pts',(-0.428339485918187,5.80517822298404,
13.7025245610697));
#36615=CARTESIAN_POINT('Ctrl Pts',(-3.15353665418747,4.89272679459021,13.8414709463548));
#36616=CARTESIAN_POINT('Ctrl Pts',(-5.1100455545729,2.78765194132884,13.98041733164));
#36617=CARTESIAN_POINT('Ctrl Pts',(-5.82095863766027,0.00307480944400744,
14.1193637169251));
#36618=CARTESIAN_POINT('Ctrl Pts',(-5.11298774910743,-2.78225182060899,
14.2583101022102));
#36619=CARTESIAN_POINT('Ctrl Pts',(-3.15870387054901,-4.88939247493832,
14.3972564874954));
#36620=CARTESIAN_POINT('Ctrl Pts',(-0.434472192656758,-5.80472245930956,
14.5362028727805));
#36621=CARTESIAN_POINT('Ctrl Pts',(2.39566397084646,-5.30512611109228,14.6751492580656));
#36622=CARTESIAN_POINT('Ctrl Pts',(4.6418466275032,-3.51238221191002,14.8140956433507));
#36623=CARTESIAN_POINT('Ctrl Pts',(5.75655899059612,-0.863479880247238,
14.9530420286359));
#36624=CARTESIAN_POINT('Ctrl Pts',(5.46808507596602,1.99589942577334,15.091988413921));
#36625=CARTESIAN_POINT('Ctrl Pts',(3.8467416543003,4.36876957058571,15.2309347992061));
#36626=CARTESIAN_POINT('Ctrl Pts',(1.28773823261074,5.67673314152403,15.3698811844912));
#36627=CARTESIAN_POINT('Ctrl Pts',(-1.58515698107652,5.60096833245369,15.5088275697763));
#36628=CARTESIAN_POINT('Ctrl Pts',(-4.07166328994811,4.15994314493526,15.6477739550615));
#36629=CARTESIAN_POINT('Ctrl Pts',(-5.5656839723722,1.7049137325636,15.7867203403466));
#36630=CARTESIAN_POINT('Ctrl Pts',(-5.70304499249917,-1.16569581338135,
15.9256667256317));
#36631=CARTESIAN_POINT('Ctrl Pts',(-4.45026400456468,-3.75216193753426,
16.0646131109168));
#36632=CARTESIAN_POINT('Ctrl Pts',(-2.11271182021736,-5.42402227876312,
16.203559496202));
#36633=CARTESIAN_POINT('Ctrl Pts',(0.739823054267452,-5.77375361131554,
16.3425058814871));
#36634=CARTESIAN_POINT('Ctrl Pts',(3.41202284326333,-4.71610740259953,16.4814522667722));
#36635=CARTESIAN_POINT('Ctrl Pts',(5.2525272321485,-2.50888951357832,16.6203986520574));
#36636=CARTESIAN_POINT('Ctrl Pts',(5.81270527545858,0.309881100521729,16.7593450373425));
#36637=CARTESIAN_POINT('Ctrl Pts',(4.95601114004255,3.05311684931627,16.8982914226276));
#36638=CARTESIAN_POINT('Ctrl Pts',(2.89126774545787,5.05214209418933,17.0372378079127));
#36639=CARTESIAN_POINT('Ctrl Pts',(0.121765269575306,5.81968574193917,17.1761841931979));
#36640=CARTESIAN_POINT('Ctrl Pts',(-2.67741802007991,5.1686556919141,17.315130578483));
#36641=CARTESIAN_POINT('Ctrl Pts',(-4.82396902860301,3.25774334883577,17.4540769637681));
#36642=CARTESIAN_POINT('Ctrl Pts',(-5.79465661660804,0.552741903066509,
17.5930233490532));
#36643=CARTESIAN_POINT('Ctrl Pts',(-5.35287146493922,-2.28699278434459,
17.7319697343384));
#36644=CARTESIAN_POINT('Ctrl Pts',(-3.60630062475619,-4.56926303901273,
17.8709161196235));
#36645=CARTESIAN_POINT('Ctrl Pts',(-0.980678330697991,-5.73775556533251,
18.0098625049086));
#36646=CARTESIAN_POINT('Ctrl Pts',(1.88398856947714,-5.5076452305758,18.1488088901936));
#36647=CARTESIAN_POINT('Ctrl Pts',(4.28942506614282,-3.93502242912927,18.2877552754789));
#36648=CARTESIAN_POINT('Ctrl Pts',(5.64929555680298,-1.40322080503777,18.426701660764));
#36649=CARTESIAN_POINT('Ctrl Pts',(5.63212569800144,1.47062199008331,18.5656480460491));
#36650=CARTESIAN_POINT('Ctrl Pts',(4.24210071745844,3.985994282327,18.7045944313342));
#36651=CARTESIAN_POINT('Ctrl Pts',(1.81804524662069,5.52976314113405,18.8435408166194));
#36652=CARTESIAN_POINT('Ctrl Pts',(-1.04916665612453,5.72562819640615,18.9824872019045));
#36653=CARTESIAN_POINT('Ctrl Pts',(-3.66063962571136,4.52584648949526,19.1214335871896));
#36654=CARTESIAN_POINT('Ctrl Pts',(-5.37981577372854,2.22287002691262,19.2603799724748));
#36655=CARTESIAN_POINT('Ctrl Pts',(-5.78763844083714,-0.621940667547248,
19.3993263577599));
#36656=CARTESIAN_POINT('Ctrl Pts',(-4.78469907912408,-3.31515062071602,
19.538272743045));
#36657=CARTESIAN_POINT('Ctrl Pts',(-2.61546851778496,-5.20027819912362,
19.6772191283301));
#36658=CARTESIAN_POINT('Ctrl Pts',(0.191293864207407,-5.8178153608826,19.8161655136153));
#36659=CARTESIAN_POINT('Ctrl Pts',(2.9514275352447,-5.01723473837972,19.9551118989004));
#36660=CARTESIAN_POINT('Ctrl Pts',(4.99213791470887,-2.99368133847456,20.0940582841855));
#36661=CARTESIAN_POINT('Ctrl Pts',(5.81599297663645,-0.24040509878175,20.2330046694706));
#36662=CARTESIAN_POINT('Ctrl Pts',(5.22217446838412,2.57147092878024,20.3719510547558));
#36663=CARTESIAN_POINT('Ctrl Pts',(3.35542823266775,4.75653973926645,20.5108974400409));
#36664=CARTESIAN_POINT('Ctrl Pts',(0.670781779190222,5.78218131162548,20.649843825326));
#36665=CARTESIAN_POINT('Ctrl Pts',(-2.1773706488537,5.3983910541304,20.7887902106111));
#36666=CARTESIAN_POINT('Ctrl Pts',(-4.49477951620812,3.69871951038204,20.9277365958963));
#36667=CARTESIAN_POINT('Ctrl Pts',(-5.71656633767768,1.09746900764223,21.0666829811814));
#36668=CARTESIAN_POINT('Ctrl Pts',(-5.54491526442117,-1.77129433640875,
21.2056293664665));
#36669=CARTESIAN_POINT('Ctrl Pts',(-4.02166699171225,-4.20829698614261,
21.3445757517516));
#36670=CARTESIAN_POINT('Ctrl Pts',(-1.51811990758472,-5.61950895203485,
21.4835221370368));
#36671=CARTESIAN_POINT('Ctrl Pts',(1.35547550328467,-5.66094118285996,21.6224685223219));
#36672=CARTESIAN_POINT('Ctrl Pts',(3.89866786797563,-4.32249439224843,21.761414907607));
#36673=CARTESIAN_POINT('Ctrl Pts',(5.49154299233608,-1.93042080364079,21.9003612928921));
#36674=CARTESIAN_POINT('Ctrl Pts',(5.74583064057415,0.932201247394659,22.0393076781773));
#36675=CARTESIAN_POINT('Ctrl Pts',(4.59954709304317,3.56759519209829,22.1782540634624));
#36676=CARTESIAN_POINT('Ctrl Pts',(2.33210394734911,5.33337230038963,22.3172004487475));
#36677=CARTESIAN_POINT('Ctrl Pts',(-0.503799673168457,5.79911672628859,
22.4561468340326));
#36678=CARTESIAN_POINT('Ctrl Pts',(-3.21689993333379,4.85130124139101,22.5950932193178));
#36679=CARTESIAN_POINT('Ctrl Pts',(-5.14586685088318,2.72095999029507,22.7340396046029));
#36680=CARTESIAN_POINT('Ctrl Pts',(-5.82050635444362,-0.0726270864499248,
22.872985989888));
#36681=CARTESIAN_POINT('Ctrl Pts',(-5.07637213236399,-2.84851099516275,
23.0119323751731));
#36682=CARTESIAN_POINT('Ctrl Pts',(-3.0948501360281,-4.9300579663257,23.1508787604583));
#36683=CARTESIAN_POINT('Ctrl Pts',(-0.358944965720083,-5.80988187723202,
23.2898251457433));
#36684=CARTESIAN_POINT('Ctrl Pts',(2.46445460031621,-5.2735218250032,23.4287715310286));
#36685=CARTESIAN_POINT('Ctrl Pts',(4.68713264453987,-3.45171790392748,23.5677179163136));
#36686=CARTESIAN_POINT('Ctrl Pts',(5.76730173168865,-0.788542739149756,
23.7066643015988));
#36687=CARTESIAN_POINT('Ctrl Pts',(5.44166595127444,2.06684314609144,23.8456106868839));
#36688=CARTESIAN_POINT('Ctrl Pts',(3.7896004403121,4.41842702990455,23.984557072169));
#36689=CARTESIAN_POINT('Ctrl Pts',(1.21380334862841,5.69300011827361,24.1235034574541));
#36690=CARTESIAN_POINT('Ctrl Pts',(-1.65786358568728,5.5798796803387,24.2624498427393));
#36691=CARTESIAN_POINT('Ctrl Pts',(-4.12541906425775,4.10663931458115,24.4013962280244));
#36692=CARTESIAN_POINT('Ctrl Pts',(-5.58738571271641,1.63238776433096,24.5403426133096));
#36693=CARTESIAN_POINT('Ctrl Pts',(-5.68740280533154,-1.23976539946543,
24.6792889985946));
#36694=CARTESIAN_POINT('Ctrl Pts',(-4.40109074100391,-3.80972035788119,
24.8182353838798));
#36695=CARTESIAN_POINT('Ctrl Pts',(-2.04199367701263,-5.45103941820688,
24.9571817691649));
#36696=CARTESIAN_POINT('Ctrl Pts',(0.814848222298178,-5.76364392467321,
25.0961281544501));
#36697=CARTESIAN_POINT('Ctrl Pts',(3.47306732527811,-4.671335169937,25.2350745397351));
#36698=CARTESIAN_POINT('Ctrl Pts',(5.28471117029584,-2.44036816123203,25.3740209250203));
#36699=CARTESIAN_POINT('Ctrl Pts',(5.80818369491154,0.385449195055016,25.5129673103054));
#36700=CARTESIAN_POINT('Ctrl Pts',(4.91588619571472,3.11731163449957,25.6519136955906));
#36701=CARTESIAN_POINT('Ctrl Pts',(2.82532006695232,5.08931581207938,25.7908600808756));
#36702=CARTESIAN_POINT('Ctrl Pts',(0.0460698902024037,5.82077713720612,
25.9298064661608));
#36703=CARTESIAN_POINT('Ctrl Pts',(-2.7444100225502,5.13339873221737,26.0687528514459));
#36704=CARTESIAN_POINT('Ctrl Pts',(-4.86592806235428,3.19473207136341,26.2076992367311));
#36705=CARTESIAN_POINT('Ctrl Pts',(-5.80135498476745,0.477335580612477,
26.3466456220161));
#36706=CARTESIAN_POINT('Ctrl Pts',(-5.32267641115013,-2.35641353289075,
26.4855920073013));
#36707=CARTESIAN_POINT('Ctrl Pts',(-3.54657232463761,-4.6157766044209,26.6245383925864));
#36708=CARTESIAN_POINT('Ctrl Pts',(-0.905975817042736,-5.75002406383996,
26.7634847778716));
#36709=CARTESIAN_POINT('Ctrl Pts',(1.95545623423369,-5.48267816234013,26.9024311631566));
#36710=CARTESIAN_POINT('Ctrl Pts',(4.34023732804627,-3.87890562556482,27.0413775484418));
#36711=CARTESIAN_POINT('Ctrl Pts',(5.66706670613347,-1.32963298095314,27.1803239337269));
#36712=CARTESIAN_POINT('Ctrl Pts',(5.61252393985844,1.5437434826812,27.3192703190121));
#36713=CARTESIAN_POINT('Ctrl Pts',(4.18990406559815,4.04082576175822,27.4582167042971));
#36714=CARTESIAN_POINT('Ctrl Pts',(1.74597686183295,5.55293919593477,27.5971630895823));
#36715=CARTESIAN_POINT('Ctrl Pts',(-1.12353979176645,5.7114995624724,27.7361094748674));
#36716=CARTESIAN_POINT('Ctrl Pts',(-3.71918873709466,4.47785708276549,27.8750558601526));
#36717=CARTESIAN_POINT('Ctrl Pts',(-5.40826926044047,2.15271747388722,28.0140022454376));
#36718=CARTESIAN_POINT('Ctrl Pts',(-5.7790606418044,-0.697156377115153,
28.1529486307229));
#36719=CARTESIAN_POINT('Ctrl Pts',(-4.74118087014855,-3.37709533065652,
28.2918950160079));
#36720=CARTESIAN_POINT('Ctrl Pts',(-2.5476176514781,-5.23385261711504,28.4308414012931));
#36721=CARTESIAN_POINT('Ctrl Pts',(0.266938444235501,-5.81483557659147,
28.5697877865781));
#36722=CARTESIAN_POINT('Ctrl Pts',(3.01642713378518,-4.97842708718019,28.7087341718633));
#36723=CARTESIAN_POINT('Ctrl Pts',(5.03064859706422,-2.92850535404333,28.8476805571484));
#36724=CARTESIAN_POINT('Ctrl Pts',(5.81862759657655,-0.16474771064401,28.9866269424335));
#36725=CARTESIAN_POINT('Ctrl Pts',(5.1882908258459,2.63916790338318,29.1255733277187));
#36726=CARTESIAN_POINT('Ctrl Pts',(3.29328561281214,4.79977486849638,29.2645197130038));
#36727=CARTESIAN_POINT('Ctrl Pts',(0.595527715740968,5.79041584478949,29.4034660982889));
#36728=CARTESIAN_POINT('Ctrl Pts',(-2.24739265080135,5.36961778797418,29.542412483574));
#36729=CARTESIAN_POINT('Ctrl Pts',(-4.54250128929371,3.63995205360863,29.6813588688592));
#36730=CARTESIAN_POINT('Ctrl Pts',(-5.73035549226509,1.0230321833023,29.8203052541443));
#36731=CARTESIAN_POINT('Ctrl Pts',(-5.52141063413822,-1.84325622880545,
29.9592516394294));
#36732=CARTESIAN_POINT('Ctrl Pts',(-3.96659793236503,-4.26024292250597,
30.0981980247146));
#36733=CARTESIAN_POINT('Ctrl Pts',(-1.44490974177441,-5.63877688456727,
30.2371444099997));
#36734=CARTESIAN_POINT('Ctrl Pts',(1.42898147939723,-5.64283446924899,30.3760907952848));
#36735=CARTESIAN_POINT('Ctrl Pts',(3.95455225318248,-4.27142662264661,30.5150371805699));
#36736=CARTESIAN_POINT('Ctrl Pts',(5.51618372481357,-1.85883996888017,30.6539835658551));
#36737=CARTESIAN_POINT('Ctrl Pts',(5.73322143466762,1.00684700767919,30.7929299511402));
#36738=CARTESIAN_POINT('Ctrl Pts',(4.55276149750459,3.62711064935227,30.9318763364253));
#36739=CARTESIAN_POINT('Ctrl Pts',(2.26254615446798,5.36325030319366,31.0708227217104));
#36740=CARTESIAN_POINT('Ctrl Pts',(-0.579174649009589,5.79207438157948,
31.2097691069956));
#36741=CARTESIAN_POINT('Ctrl Pts',(-3.27971911411854,4.8090551513047,31.3487154922807));
#36742=CARTESIAN_POINT('Ctrl Pts',(-5.18081778822028,2.6538078229339,31.4876618775658));
#36743=CARTESIAN_POINT('Ctrl Pts',(-5.81906960542543,-0.148316698381154,
31.626608262851));
#36744=CARTESIAN_POINT('Ctrl Pts',(-5.03889791080926,-2.91428837973299,
31.7655546481361));
#36745=CARTESIAN_POINT('Ctrl Pts',(-3.03047294634127,-4.9698896001117,31.9045010334212));
#36746=CARTESIAN_POINT('Ctrl Pts',(-0.283357027734952,-5.81405862635028,
32.0434474187063));
#36747=CARTESIAN_POINT('Ctrl Pts',(2.53282839813492,-5.2410255886998,32.1823938039914));
#36748=CARTESIAN_POINT('Ctrl Pts',(4.7316258917529,-3.39046978106256,32.3213401892766));
#36749=CARTESIAN_POINT('Ctrl Pts',(5.77706900587568,-0.713472225917252,
32.4602865745617));
#36750=CARTESIAN_POINT('Ctrl Pts',(5.41432643689403,2.13743728575958,32.5992329598468));
#36751=CARTESIAN_POINT('Ctrl Pts',(3.73181826283932,4.46733716759143,32.7381793451319));
#36752=CARTESIAN_POINT('Ctrl Pts',(1.13966316500139,5.70830419530563,32.8771257304171));
#36753=CARTESIAN_POINT('Ctrl Pts',(-1.73028978342203,5.55784726141247,33.0160721157022));
#36754=CARTESIAN_POINT('Ctrl Pts',(-4.17847707556568,4.05264089758481,33.1550185009873));
#36755=CARTESIAN_POINT('Ctrl Pts',(-5.60814241669793,1.55958569813855,33.2939648862725));
#36756=CARTESIAN_POINT('Ctrl Pts',(-5.67079866516178,-1.31362529474889,
33.4329112715576));
#36757=CARTESIAN_POINT('Ctrl Pts',(-4.35117308802745,-3.86663441171134,
33.5718576568427));
#36758=CARTESIAN_POINT('Ctrl Pts',(-1.97093015613459,-5.47713458255719,
33.7108040421278));
#36759=CARTESIAN_POINT('Ctrl Pts',(0.889735568950635,-5.75255938979764,
33.8497504274129));
#36760=CARTESIAN_POINT('Ctrl Pts',(3.53352438142312,-4.62577283939593,33.9886968126981));
#36761=CARTESIAN_POINT('Ctrl Pts',(5.31600126569122,-2.37143405115432,34.1276431979832));
#36762=CARTESIAN_POINT('Ctrl Pts',(5.80267973278655,0.460952095681341,34.2665895832684));
#36763=CARTESIAN_POINT('Ctrl Pts',(4.87492979076306,3.18097916543565,34.4055359685534));
#36764=CARTESIAN_POINT('Ctrl Pts',(2.75889452091848,5.12562873589677,34.5444823538386));
#36765=CARTESIAN_POINT('Ctrl Pts',(-0.0296332813159625,5.82088402087201,
34.6834287391237));
#36766=CARTESIAN_POINT('Ctrl Pts',(-2.81093784241375,5.0972735223736,34.8223751244088));
#36767=CARTESIAN_POINT('Ctrl Pts',(-4.90706408527485,3.13118044494573,34.961321509694));
#36768=CARTESIAN_POINT('Ctrl Pts',(-5.80707212633982,0.401848522819139,
35.1002678949791));
#36769=CARTESIAN_POINT('Ctrl Pts',(-5.29158109326361,-2.42543572358036,
35.2392142802642));
#36770=CARTESIAN_POINT('Ctrl Pts',(-3.48624416619839,-4.66150946898669,
35.3781606655493));
#36771=CARTESIAN_POINT('Ctrl Pts',(-0.831120068916907,-5.76132001774319,
35.5171070508345));
#36772=CARTESIAN_POINT('Ctrl Pts',(2.02659315804246,-5.45678376771338,35.6560534361196));
#36773=CARTESIAN_POINT('Ctrl Pts',(4.39031549312739,-3.8221327536613,35.7949998214048));
#36774=CARTESIAN_POINT('Ctrl Pts',(5.68387934205856,-1.255820266091,35.9339462066898));
#36775=CARTESIAN_POINT('Ctrl Pts',(5.59197289353619,1.61660387039037,36.072892591975));
#36776=CARTESIAN_POINT('Ctrl Pts',(4.13699874390506,4.09497378608617,36.2118389772602));
#36777=CARTESIAN_POINT('Ctrl Pts',(1.67361316691114,5.57517604057006,36.3507853625452));
#36778=CARTESIAN_POINT('Ctrl Pts',(-1.19772289471474,5.69640489987157,36.4897317478304));
#36779=CARTESIAN_POINT('Ctrl Pts',(-3.77710879425175,4.42911030255408,36.6286781331154));
#36780=CARTESIAN_POINT('Ctrl Pts',(-5.43580800609587,2.08220081564407,36.7676245184007));
#36781=CARTESIAN_POINT('Ctrl Pts',(-5.76950538699365,-0.772254171407353,
36.9065709036857));
#36782=CARTESIAN_POINT('Ctrl Pts',(-4.69686074976853,-3.43846884718893,
37.0455172889708));
#36783=CARTESIAN_POINT('Ctrl Pts',(-2.47933588753095,-5.26654179444213,
37.184463674256));
#36784=CARTESIAN_POINT('Ctrl Pts',(0.342537874966791,-5.81087228563992,
37.3234100595411));
#36785=CARTESIAN_POINT('Ctrl Pts',(3.08091654142906,-4.93877739734782,37.4623564448262));
#36786=CARTESIAN_POINT('Ctrl Pts',(5.06830840817201,-2.86283404958403,37.6013028301114));
#36787=CARTESIAN_POINT('Ctrl Pts',(5.8202780684835,-0.0890624574929409,
37.7402492153965));
#36788=CARTESIAN_POINT('Ctrl Pts',(5.1535296488501,2.7064184957666,37.8791956006816));
#36789=CARTESIAN_POINT('Ctrl Pts',(3.2305859749132,4.84219817588035,38.0181419859667));
#36790=CARTESIAN_POINT('Ctrl Pts',(0.520172926232102,5.79767100158503,38.1570883712518));
#36791=CARTESIAN_POINT('Ctrl Pts',(-2.31703453441006,5.3399363181742,38.296034756537));
#36792=CARTESIAN_POINT('Ctrl Pts',(-4.58945475513934,3.58056894450221,38.4349811418222));
#36793=CARTESIAN_POINT('Ctrl Pts',(-5.74317542894098,0.948422325872549,
38.5739275271072));
#36794=CARTESIAN_POINT('Ctrl Pts',(-5.49697212635136,-1.91490635748093,
38.7128739123924));
#36795=CARTESIAN_POINT('Ctrl Pts',(-3.91085797262269,-4.31146829209936,
38.8518202976775));
#36796=CARTESIAN_POINT('Ctrl Pts',(-1.37145518756544,-5.6570910885635,38.9907666829627));
#36797=CARTESIAN_POINT('Ctrl Pts',(1.50224576117741,-5.62377334081214,39.1297130682477));
#36798=CARTESIAN_POINT('Ctrl Pts',(4.00976777537009,-4.21963639469189,39.2686594535329));
#36799=CARTESIAN_POINT('Ctrl Pts',(5.5398914638535,-1.78694473460368,39.407605838818));
#36800=CARTESIAN_POINT('Ctrl Pts',(5.71964252611128,1.08132247239395,39.5465522241031));
#36801=CARTESIAN_POINT('Ctrl Pts',(4.5052058593401,3.68601262623616,39.6854986093882));
#36802=CARTESIAN_POINT('Ctrl Pts',(2.19260568022234,5.39222117933431,39.8244449946734));
#36803=CARTESIAN_POINT('Ctrl Pts',(-0.654451664707701,5.78405237998118,
39.9633913799585));
#36804=CARTESIAN_POINT('Ctrl Pts',(-3.34198357146349,4.76599566972871,40.1023377652437));
#36805=CARTESIAN_POINT('Ctrl Pts',(-5.21489245507062,2.58620679719397,40.2412841505287));
#36806=CARTESIAN_POINT('Ctrl Pts',(-5.81664863361382,-0.223981224399285,
40.3802305358138));
#36807=CARTESIAN_POINT('Ctrl Pts',(-5.00057142273866,-2.9795728488987,40.519176921099));
#36808=CARTESIAN_POINT('Ctrl Pts',(-2.96558319008412,-5.00888063927413,
40.6581233063842));
#36809=CARTESIAN_POINT('Ctrl Pts',(-0.207721163454829,-5.81725200021949,
40.7970696916693));
#36810=CARTESIAN_POINT('Ctrl Pts',(2.60077379973059,-5.20764289851364,40.9360160769543));
#36811=CARTESIAN_POINT('Ctrl Pts',(4.77531884366656,-3.32864820266846,41.0749624622396));
#36812=CARTESIAN_POINT('Ctrl Pts',(5.78585916114505,-0.63828103778719,41.2139088475246));
#36813=CARTESIAN_POINT('Ctrl Pts',(5.38607115696136,2.20766990466273,41.3528552328098));
#36814=CARTESIAN_POINT('Ctrl Pts',(3.67340489501397,4.51549171110879,41.4918016180949));
#36815=CARTESIAN_POINT('Ctrl Pts',(1.06533022161374,5.72264278412703,41.6307480033799));
#36816=CARTESIAN_POINT('Ctrl Pts',(-1.80242332429591,5.53487480218286,41.7696943886652));
#36817=CARTESIAN_POINT('Ctrl Pts',(-4.23082834977319,3.99795702710274,41.9086407739503));
#36818=CARTESIAN_POINT('Ctrl Pts',(-5.62795057358003,1.48651984754489,42.0475871592354));
#36819=CARTESIAN_POINT('Ctrl Pts',(-5.65323538037245,-1.38726300675469,
42.1865335445205));
#36820=CARTESIAN_POINT('Ctrl Pts',(-4.30051948858164,-3.92289447272474,
42.3254799298057));
#36821=CARTESIAN_POINT('Ctrl Pts',(-1.8995332770884,-5.50230335814362,42.4644263150907));
#36822=CARTESIAN_POINT('Ctrl Pts',(0.964472427967387,-5.74050188149918,
42.603372700376));
#36823=CARTESIAN_POINT('Ctrl Pts',(3.59338378614392,-4.57942811727434,42.7423190856609));
#36824=CARTESIAN_POINT('Ctrl Pts',(5.3463922260065,-2.30209884268725,42.8812654709462));
#36825=CARTESIAN_POINT('Ctrl Pts',(5.79619432000995,0.536377032029781,43.0202118562312));
#36826=CARTESIAN_POINT('Ctrl Pts',(4.83314885245102,3.24410867355829,43.1591582415163));
#36827=CARTESIAN_POINT('Ctrl Pts',(2.69200234240633,5.16107472376478,43.2981046268015));
#36828=CARTESIAN_POINT('Ctrl Pts',(-0.105331440735626,5.82000637485882,
43.4370510120867));
#36829=CARTESIAN_POINT('Ctrl Pts',(-2.87699022732243,5.06028617251001,43.5759973973718));
#36830=CARTESIAN_POINT('Ctrl Pts',(-4.94737013972126,3.06709921854501,43.7149437826568));
#36831=CARTESIAN_POINT('Ctrl Pts',(-5.81180707434219,0.326293497377598,
43.853890167942));
#36832=CARTESIAN_POINT('Ctrl Pts',(-5.25959077066355,-2.49404768217361,
43.9928365532272));
#36833=CARTESIAN_POINT('Ctrl Pts',(-3.42532635319164,-4.70645389756827,
44.1317829385122));
#36834=CARTESIAN_POINT('Ctrl Pts',(-0.756123747233696,-5.77164151647293,
44.2707293237974));
#36835=CARTESIAN_POINT('Ctrl Pts',(2.09738730898287,-5.42996642640841,44.4096757090826));
#36836=CARTESIAN_POINT('Ctrl Pts',(4.43965109129104,-3.76471341583966,44.5486220943676));
#36837=CARTESIAN_POINT('Ctrl Pts',(5.69973062093118,-1.18179514494863,44.6875684796528));
#36838=CARTESIAN_POINT('Ctrl Pts',(5.57047603498711,1.68919082978778,44.8265148649379));
#36839=CARTESIAN_POINT('Ctrl Pts',(4.08339370065241,4.14842919684994,44.965461250223));
#36840=CARTESIAN_POINT('Ctrl Pts',(1.60096640126895,5.59646991395581,45.1044076355082));
#36841=CARTESIAN_POINT('Ctrl Pts',(-1.27170341782562,5.68034676167709,45.2433540207932));
#36842=CARTESIAN_POINT('Ctrl Pts',(-3.83439000072971,4.37961439376897,45.3823004060785));
#36843=CARTESIAN_POINT('Ctrl Pts',(-5.46242735286052,2.01133197919349,45.5212467913633));
#36844=CARTESIAN_POINT('Ctrl Pts',(-5.75897429255667,-0.84722134857191,
45.6601931766487));
#36845=CARTESIAN_POINT('Ctrl Pts',(-4.65174621417769,-3.49926078975088,
45.7991395619337));
#36846=CARTESIAN_POINT('Ctrl Pts',(-2.41063477494917,-5.29834020214,45.938085947219));
#36847=CARTESIAN_POINT('Ctrl Pts',(0.418079369703333,-5.80592615836837,
46.0770323325039));
#36848=CARTESIAN_POINT('Ctrl Pts',(3.14488485060045,-4.89829237513266,46.2159787177892));
#36849=CARTESIAN_POINT('Ctrl Pts',(5.10511097834549,-2.79667853257378,46.3549251030743));
#36850=CARTESIAN_POINT('Ctrl Pts',(5.82094411320247,-0.0133621405463012,
46.4938714883593));
#36851=CARTESIAN_POINT('Ctrl Pts',(5.11789681681116,2.77321133134302,46.6328178736445));
#36852=CARTESIAN_POINT('Ctrl Pts',(3.167339923837,4.8838024860302,46.7717642589297));
#36853=CARTESIAN_POINT('Ctrl Pts',(0.444730155969368,5.80394555492573,46.9107106442148));
#36854=CARTESIAN_POINT('Ctrl Pts',(-2.38628452059998,5.30935166491599,47.0496570294999));
#36855=CARTESIAN_POINT('Ctrl Pts',(-4.63563197220621,3.52058022709674,47.188603414785));
#36856=CARTESIAN_POINT('Ctrl Pts',(-5.75502397927113,0.873652054434358,
47.3275498000702));
#36857=CARTESIAN_POINT('Ctrl Pts',(-5.47160387472823,-1.98623260323923,
47.4664961853552));
#36858=CARTESIAN_POINT('Ctrl Pts',(-3.85445653981176,-4.36196443171659,
47.6054425706403));
#36859=CARTESIAN_POINT('Ctrl Pts',(-1.29776866963795,-5.67444846460127,
47.7443889559256));
#36860=CARTESIAN_POINT('Ctrl Pts',(1.57525595837582,-5.60376102502237,47.8833353412107));
#36861=CARTESIAN_POINT('Ctrl Pts',(4.06430509262118,-4.16713246117787,48.0222817264957));
#36862=CARTESIAN_POINT('Ctrl Pts',(5.5626622052556,-1.71474727441282,48.161228111781));
#36863=CARTESIAN_POINT('Ctrl Pts',(5.70509620054379,1.15561507115043,48.300174497066));
#36864=CARTESIAN_POINT('Ctrl Pts',(4.45688824359047,3.74429110905929,48.4391208823512));
#36865=CARTESIAN_POINT('Ctrl Pts',(2.12229431199977,5.42028012862584,48.5780672676363));
#36866=CARTESIAN_POINT('Ctrl Pts',(-0.729617905772954,5.77505188332996,
48.7170136529215));
#36867=CARTESIAN_POINT('Ctrl Pts',(-3.40368293483593,4.72213046030083,48.8559600382065));
#36868=CARTESIAN_POINT('Ctrl Pts',(-5.24808477435825,2.51816760377688,48.9949064234917));
#36869=CARTESIAN_POINT('Ctrl Pts',(-5.81324446105805,-0.29960641592774,
49.1338528087768));
#36870=CARTESIAN_POINT('Ctrl Pts',(-4.96139795468468,-3.04435619311404,
49.272799194062));
#36871=CARTESIAN_POINT('Ctrl Pts',(-2.90019417731,-5.04701895910092,49.4117455793471));
#36872=CARTESIAN_POINT('Ctrl Pts',(-0.132045607590425,-5.81947225476929,
49.5506919646322));
#36873=CARTESIAN_POINT('Ctrl Pts',(2.66827041381441,-5.17335832170609,49.6896383499173));
#36874=CARTESIAN_POINT('Ctrl Pts',(4.81822148792321,-3.26630479921574,49.8285847352024));
#36875=CARTESIAN_POINT('Ctrl Pts',(5.79363674149707,-0.562901276687905,
49.9675311204876));
#36876=CARTESIAN_POINT('Ctrl Pts',(5.35697166214563,2.27736928561665,50.1064775057727));
#36877=CARTESIAN_POINT('Ctrl Pts',(3.61416560046215,4.56331157564723,50.2454294290219));
#36878=CARTESIAN_POINT('Ctrl Pts',(1.86528972090092,5.34454787483767,50.3380658905095));
#36879=CARTESIAN_POINT('Ctrl Pts',(0.950154512558094,5.50256753975008,50.3843868902353));
#36880=CARTESIAN_POINT('Ctrl Pts',(-2.58408645063866,5.32305769023755,0.000220296677514235));
#36881=CARTESIAN_POINT('Ctrl Pts',(-3.4692611475833,4.8933482874975,0.0465357584392229));
#36882=CARTESIAN_POINT('Ctrl Pts',(-5.02021061948039,3.58425708503786,0.13916668196264));
#36883=CARTESIAN_POINT('Ctrl Pts',(-6.12306759730524,0.745034473240605,
0.278113067247767));
#36884=CARTESIAN_POINT('Ctrl Pts',(-5.73331406242883,-2.27499744055186,
0.417059452532892));
#36885=CARTESIAN_POINT('Ctrl Pts',(-3.9460860794766,-4.7408798866814,0.556005837818019));
#36886=CARTESIAN_POINT('Ctrl Pts',(-1.19695885730938,-6.05095353285258,
0.694952223103144));
#36887=CARTESIAN_POINT('Ctrl Pts',(1.84392018446255,-5.88618259004128,0.83389860838827));
#36888=CARTESIAN_POINT('Ctrl Pts',(4.43534186760578,-4.286577006635,0.972844993673396));
#36889=CARTESIAN_POINT('Ctrl Pts',(5.94562651323158,-1.64212630236546,1.11179137895852));
#36890=CARTESIAN_POINT('Ctrl Pts',(6.00664047788067,1.40261348122994,1.25073776424365));
#36891=CARTESIAN_POINT('Ctrl Pts',(4.60350888165559,4.10545313734612,1.38968414952877));
#36892=CARTESIAN_POINT('Ctrl Pts',(2.07825241101868,5.80757432743904,1.5286305348139));
#36893=CARTESIAN_POINT('Ctrl Pts',(-0.953587337660047,6.09407219459964,
1.66757692009903));
#36894=CARTESIAN_POINT('Ctrl Pts',(-3.75298591552093,4.8951144133636,1.80652330538415));
#36895=CARTESIAN_POINT('Ctrl Pts',(-5.63757791961995,2.50295073333117,1.94546969066928));
#36896=CARTESIAN_POINT('Ctrl Pts',(-6.14798576986681,-0.499317821657796,
2.08441607595441));
#36897=CARTESIAN_POINT('Ctrl Pts',(-5.1597953784654,-3.37987561340746,2.22336246123953));
#36898=CARTESIAN_POINT('Ctrl Pts',(-2.9138824262184,-5.43657396736167,2.36230884652466));
#36899=CARTESIAN_POINT('Ctrl Pts',(0.0423020301180563,-6.16808381712523,
2.50125523180978));
#36900=CARTESIAN_POINT('Ctrl Pts',(2.98817518474946,-5.39609640682365,2.64020161709491));
#36901=CARTESIAN_POINT('Ctrl Pts',(5.20566764746265,-3.30878704922065,2.77914800238003));
#36902=CARTESIAN_POINT('Ctrl Pts',(6.15425599259743,-0.414946460616659,
2.91809438766516));
#36903=CARTESIAN_POINT('Ctrl Pts',(5.60271768671038,2.58003912925357,3.05704077295029));
#36904=CARTESIAN_POINT('Ctrl Pts',(3.68549258980999,4.94612896710534,3.19598715823541));
#36905=CARTESIAN_POINT('Ctrl Pts',(0.869912653233688,6.10657836780115,3.33493354352054));
#36906=CARTESIAN_POINT('Ctrl Pts',(-2.15771227404257,5.77852274635241,3.47387992880566));
#36907=CARTESIAN_POINT('Ctrl Pts',(-4.6593854549632,4.04192708608156,3.61282631409079));
#36908=CARTESIAN_POINT('Ctrl Pts',(-6.02531317687573,1.32009412839944,3.75177269937591));
#36909=CARTESIAN_POINT('Ctrl Pts',(-5.92254461988993,-1.72351751157118,
3.89071908466104));
#36910=CARTESIAN_POINT('Ctrl Pts',(-4.3761300664986,-4.34701426594362,4.02966546994617));
#36911=CARTESIAN_POINT('Ctrl Pts',(-1.76301478635964,-5.91090739652963,
4.16861185523129));
#36912=CARTESIAN_POINT('Ctrl Pts',(1.27984301178143,-6.03399115448819,4.30755824051643));
#36913=CARTESIAN_POINT('Ctrl Pts',(4.01073351232212,-4.6862633387801,4.44650462580154));
#36914=CARTESIAN_POINT('Ctrl Pts',(5.76399028457363,-2.19623846305353,4.58545101108668));
#36915=CARTESIAN_POINT('Ctrl Pts',(6.11224936889116,0.829129085091465,4.72439739637179));
#36916=CARTESIAN_POINT('Ctrl Pts',(4.97062109959005,3.65239281452117,4.86334378165692));
#36917=CARTESIAN_POINT('Ctrl Pts',(2.61738232997109,5.58536991845751,5.00229016694205));
#36918=CARTESIAN_POINT('Ctrl Pts',(-0.373854760340773,6.15688882516372,
5.14123655222717));
#36919=CARTESIAN_POINT('Ctrl Pts',(-3.27396312767273,5.22763931673701,5.2801829375123));
#36920=CARTESIAN_POINT('Ctrl Pts',(-5.37602875071488,3.0241300003046,5.41912932279743));
#36921=CARTESIAN_POINT('Ctrl Pts',(-6.16766399617026,0.0834758504031012,
5.55807570808255));
#36922=CARTESIAN_POINT('Ctrl Pts',(-5.45590433172023,-2.87752590090372,
5.69702209336768));
#36923=CARTESIAN_POINT('Ctrl Pts',(-3.41424426959418,-5.13711820525854,
5.83596847865281));
#36924=CARTESIAN_POINT('Ctrl Pts',(-0.540347325032756,-6.14451561602582,
5.97491486393793));
#36925=CARTESIAN_POINT('Ctrl Pts',(2.46526162889552,-5.65416063517396,6.11386124922306));
#36926=CARTESIAN_POINT('Ctrl Pts',(4.86995234428682,-3.78557942085893,6.25280763450818));
#36927=CARTESIAN_POINT('Ctrl Pts',(6.08757100607258,-0.994246766793666,
6.39175401979331));
#36928=CARTESIAN_POINT('Ctrl Pts',(5.82131777245357,2.03943785866883,6.53070040507843));
#36929=CARTESIAN_POINT('Ctrl Pts',(4.13609302652729,4.57600064064325,6.66964679036356));
#36930=CARTESIAN_POINT('Ctrl Pts',(1.44267762578629,5.99714337458352,6.80859317564868));
#36931=CARTESIAN_POINT('Ctrl Pts',(-1.6023967175606,5.95645634138339,6.94753956093381));
#36932=CARTESIAN_POINT('Ctrl Pts',(-4.25687989538264,4.46385718225195,7.08648594621893));
#36933=CARTESIAN_POINT('Ctrl Pts',(-5.87373009404587,1.88317343055689,7.22543233150407));
#36934=CARTESIAN_POINT('Ctrl Pts',(-6.05883304917731,-1.1565420309924,7.36437871678918));
#36935=CARTESIAN_POINT('Ctrl Pts',(-4.7670691108211,-3.91434534499841,7.50332510207432));
#36936=CARTESIAN_POINT('Ctrl Pts',(-2.31331135425011,-5.71800996549961,
7.64227148735944));
#36937=CARTESIAN_POINT('Ctrl Pts',(0.704326100885125,-6.12788480071773,
7.78121787264457));
#36938=CARTESIAN_POINT('Ctrl Pts',(3.55028100722364,-5.04406107784218,7.92016425792969));
#36939=CARTESIAN_POINT('Ctrl Pts',(5.53083948497785,-2.73072554070624,8.05911064321483));
#36940=CARTESIAN_POINT('Ctrl Pts',(6.16323179570631,0.248236217442325,8.19805702849994));
#36941=CARTESIAN_POINT('Ctrl Pts',(5.29330956465926,3.16668931850635,8.33700341378508));
#36942=CARTESIAN_POINT('Ctrl Pts',(3.13312011720682,5.31324813258417,8.4759497990702));
#36943=CARTESIAN_POINT('Ctrl Pts',(0.209219021510298,6.16467961765197,8.61489618435532));
#36944=CARTESIAN_POINT('Ctrl Pts',(-2.76568012015457,5.51344364805129,8.75384256964046));
#36945=CARTESIAN_POINT('Ctrl Pts',(-5.06643271011871,3.51828182229544,8.89278895492557));
#36946=CARTESIAN_POINT('Ctrl Pts',(-6.13222030320556,0.665523508381978,
9.03173534021072));
#36947=CARTESIAN_POINT('Ctrl Pts',(-5.70325254062085,-2.34945905373065,
9.17068172549582));
#36948=CARTESIAN_POINT('Ctrl Pts',(-3.88409217921783,-4.7917507583966,9.30962811078097));
#36949=CARTESIAN_POINT('Ctrl Pts',(-1.11816746497952,-6.06603238596007,
9.44857449606607));
#36950=CARTESIAN_POINT('Ctrl Pts',(1.92031542952214,-5.86169225039958,9.58752088135123));
#36951=CARTESIAN_POINT('Ctrl Pts',(4.49071309046551,-4.22853914802464,9.72646726663632));
#36952=CARTESIAN_POINT('Ctrl Pts',(5.96647991447557,-1.56466124685663,9.86541365192148));
#36953=CARTESIAN_POINT('Ctrl Pts',(5.98789132304063,1.48060963481603,10.0043600372065));
#36954=CARTESIAN_POINT('Ctrl Pts',(4.54972819224755,4.16497548179135,10.1433064224917));
#36955=CARTESIAN_POINT('Ctrl Pts',(2.0025490369231,5.83411044992925,10.2822528077768));
#36956=CARTESIAN_POINT('Ctrl Pts',(-1.03276015123316,6.08115563501546,10.421199193062));
#36957=CARTESIAN_POINT('Ctrl Pts',(-3.81632956311736,4.84589269927964,10.560145578347));
#36958=CARTESIAN_POINT('Ctrl Pts',(-5.66965205440495,2.4294223529961,10.6990919636322));
#36959=CARTESIAN_POINT('Ctrl Pts',(-6.14097221145061,-0.57923025253058,
10.8380383489173));
#36960=CARTESIAN_POINT('Ctrl Pts',(-5.11540369714552,-3.44669296608871,
10.9769847342025));
#36961=CARTESIAN_POINT('Ctrl Pts',(-2.84293329499841,-5.47400928638642,
11.1159311194876));
#36962=CARTESIAN_POINT('Ctrl Pts',(0.122514456037195,-6.16701204760598,
11.2548775047727));
#36963=CARTESIAN_POINT('Ctrl Pts',(3.05809877584333,-5.35677881421669,11.3938238900578));
#36964=CARTESIAN_POINT('Ctrl Pts',(5.24825822548055,-3.24080745894155,11.532770275343));
#36965=CARTESIAN_POINT('Ctrl Pts',(6.15913191847538,-0.334875197757514,
11.6717166606281));
#36966=CARTESIAN_POINT('Ctrl Pts',(5.56869043259187,2.65268434858258,11.8106630459132));
#36967=CARTESIAN_POINT('Ctrl Pts',(3.62085644666365,4.9936405537353,11.9496094311983));
#36968=CARTESIAN_POINT('Ctrl Pts',(0.7904229619961,6.1173751665567,12.0885558164834));
#36969=CARTESIAN_POINT('Ctrl Pts',(-2.23267955562705,5.7499729902966,12.2275022017686));
#36970=CARTESIAN_POINT('Ctrl Pts',(-4.7115567261068,3.98098990251583,12.3664485870537));
#36971=CARTESIAN_POINT('Ctrl Pts',(-6.04197146345827,1.24162322063148,12.5053949723388));
#36972=CARTESIAN_POINT('Ctrl Pts',(-5.89962939213839,-1.80039451861864,
12.644341357624));
#36973=CARTESIAN_POINT('Ctrl Pts',(-4.31922701079247,-4.40355826763949,
12.7832877429091));
#36974=CARTESIAN_POINT('Ctrl Pts',(-1.68599426988362,-5.93333554665289,
12.9222341281942));
#36975=CARTESIAN_POINT('Ctrl Pts',(1.35820690332742,-6.0168364939567,13.0611805134793));
#36976=CARTESIAN_POINT('Ctrl Pts',(4.07133923972621,-4.63370739066687,13.2001268987645));
#36977=CARTESIAN_POINT('Ctrl Pts',(5.79206493832777,-2.12109196817337,13.3390732840496));
#36978=CARTESIAN_POINT('Ctrl Pts',(6.10094963010233,0.908548841950409,13.4780196693347));
#36979=CARTESIAN_POINT('Ctrl Pts',(4.92270132870797,3.71672692238643,13.6169660546198));
#36980=CARTESIAN_POINT('Ctrl Pts',(2.54452317945555,5.61893665887672,13.755912439905));
#36981=CARTESIAN_POINT('Ctrl Pts',(-0.453893555832864,6.15150615924497,
13.8948588251901));
#36982=CARTESIAN_POINT('Ctrl Pts',(-3.34167176381149,5.18461929269647,14.0338052104752));
#36983=CARTESIAN_POINT('Ctrl Pts',(-5.41490295311199,2.95395893601018,14.1727515957603));
#36984=CARTESIAN_POINT('Ctrl Pts',(-6.16822800900523,0.00325824781025046,
14.3116979810455));
#36985=CARTESIAN_POINT('Ctrl Pts',(-5.41802067441278,-2.94823665245703,
14.4506443663306));
#36986=CARTESIAN_POINT('Ctrl Pts',(-3.34714724829327,-5.18108605270152,
14.5895907516157));
#36987=CARTESIAN_POINT('Ctrl Pts',(-0.46039213035129,-6.15102320541598,
14.7285371369008));
#36988=CARTESIAN_POINT('Ctrl Pts',(2.53858557068867,-5.62162171330895,14.867483522186));
#36989=CARTESIAN_POINT('Ctrl Pts',(4.91877200364035,-3.72192549139007,15.0064299074711));
#36990=CARTESIAN_POINT('Ctrl Pts',(6.0999863788,-0.914993751732644,15.1453762927562));
#36991=CARTESIAN_POINT('Ctrl Pts',(5.7943025574829,2.11497169238796,15.2843226780413));
#36992=CARTESIAN_POINT('Ctrl Pts',(4.07623229994285,4.62940359270587,15.4232690633265));
#36993=CARTESIAN_POINT('Ctrl Pts',(1.36456269990763,6.01539824328165,15.5622154486116));
#36994=CARTESIAN_POINT('Ctrl Pts',(-1.67972498998492,5.935113423118,15.7011618338967));
#36995=CARTESIAN_POINT('Ctrl Pts',(-4.31457241180318,4.40811890612791,15.8401082191819));
#36996=CARTESIAN_POINT('Ctrl Pts',(-5.89772405279568,1.80662624367373,15.979054604467));
#36997=CARTESIAN_POINT('Ctrl Pts',(-6.04327981850941,-1.2352394190812,16.1180009897521));
#36998=CARTESIAN_POINT('Ctrl Pts',(-4.71575985832071,-3.97601010384864,
16.2569473750372));
#36999=CARTESIAN_POINT('Ctrl Pts',(-2.23875293325552,-5.7476110420848,16.3958937603224));
#37000=CARTESIAN_POINT('Ctrl Pts',(0.783959751151009,-6.11820680394433,
16.5348401456075));
#37001=CARTESIAN_POINT('Ctrl Pts',(3.61557883834099,-4.99746306149393,16.6737865308926));
#37002=CARTESIAN_POINT('Ctrl Pts',(5.56588486676205,-2.6585659738296,16.8127329161777));
#37003=CARTESIAN_POINT('Ctrl Pts',(6.15948226400517,0.328368126743459,16.9516793014629));
#37004=CARTESIAN_POINT('Ctrl Pts',(5.25167908412416,3.23526106900636,17.090625686748));
#37005=CARTESIAN_POINT('Ctrl Pts',(3.0637562984359,5.3535450620173,17.2295720720331));
#37006=CARTESIAN_POINT('Ctrl Pts',(0.129029596853515,6.16687917429807,17.3685184573182));
#37007=CARTESIAN_POINT('Ctrl Pts',(-2.83714862985361,5.4770096804164,17.5074648426033));
#37008=CARTESIAN_POINT('Ctrl Pts',(-5.11175954494723,3.45209526836909,17.6464112278885));
#37009=CARTESIAN_POINT('Ctrl Pts',(-6.14035685013834,0.585717628396678,
17.7853576131736));
#37010=CARTESIAN_POINT('Ctrl Pts',(-5.67221548097349,-2.42343122961229,
17.9243039984588));
#37011=CARTESIAN_POINT('Ctrl Pts',(-3.82144693119744,-4.84185819074629,
18.0632503837439));
#37012=CARTESIAN_POINT('Ctrl Pts',(-1.03918408011006,-6.0800611703256,18.202196769029));
#37013=CARTESIAN_POINT('Ctrl Pts',(1.99638440783797,-5.8362228096087,18.3411431543141));
#37014=CARTESIAN_POINT('Ctrl Pts',(4.54532551809133,-4.16977976898578,18.4800895395992));
#37015=CARTESIAN_POINT('Ctrl Pts',(5.9863237747773,-1.48693478363758,18.6190359248844));
#37016=CARTESIAN_POINT('Ctrl Pts',(5.96812958880847,1.55835701892862,18.7579823101695));
#37017=CARTESIAN_POINT('Ctrl Pts',(4.49517787210488,4.22379252395216,18.8969286954546));
#37018=CARTESIAN_POINT('Ctrl Pts',(1.92650700853492,5.85966024043385,19.0358750807397));
#37019=CARTESIAN_POINT('Ctrl Pts',(-1.11175831289245,6.06721030136336,19.1748214660249));
#37020=CARTESIAN_POINT('Ctrl Pts',(-3.87902771273827,4.79585147716898,19.31376785131));
#37021=CARTESIAN_POINT('Ctrl Pts',(-5.70076724546849,2.35548300784553,19.4527142365951));
#37022=CARTESIAN_POINT('Ctrl Pts',(-6.13291998087729,-0.659044683926238,
19.5916606218803));
#37023=CARTESIAN_POINT('Ctrl Pts',(-5.07014681114061,-3.51292736912334,
19.7306070071654));
#37024=CARTESIAN_POINT('Ctrl Pts',(-2.77150331625738,-5.51051873739938,
19.8695533924505));
#37025=CARTESIAN_POINT('Ctrl Pts',(0.202706159690122,-6.16489720920625,
20.0084997777356));
#37026=CARTESIAN_POINT('Ctrl Pts',(3.12750512804936,-5.31655518745741,20.1474461630208));
#37027=CARTESIAN_POINT('Ctrl Pts',(5.28996112617996,-3.17227972769742,20.2863925483059));
#37028=CARTESIAN_POINT('Ctrl Pts',(6.16296610434022,-0.25474729440942,20.425338933591));
#37029=CARTESIAN_POINT('Ctrl Pts',(5.53372130415038,2.72488089927755,20.5642853188761));
#37030=CARTESIAN_POINT('Ctrl Pts',(3.55560788098422,5.04030752870678,20.7032317041613));
#37031=CARTESIAN_POINT('Ctrl Pts',(0.710799580598698,6.12713728779403,20.8421780894464));
#37032=CARTESIAN_POINT('Ctrl Pts',(-2.30726920740392,5.72045069831224,20.9811244747315));
#37033=CARTESIAN_POINT('Ctrl Pts',(-4.76293109640132,3.9193793843144,21.1200708600166));
#37034=CARTESIAN_POINT('Ctrl Pts',(-6.0576078261867,1.1629423078455,21.2590172453017));
#37035=CARTESIAN_POINT('Ctrl Pts',(-5.8757163159144,-1.87696701147159,21.3979636305869));
#37036=CARTESIAN_POINT('Ctrl Pts',(-4.26159341189583,-4.45935746256581,
21.536910015872));
#37037=CARTESIAN_POINT('Ctrl Pts',(-1.60868858857865,-5.95476014733023,
21.6758564011572));
#37038=CARTESIAN_POINT('Ctrl Pts',(1.43634107117479,-5.99866416083712,21.8148027864422));
#37039=CARTESIAN_POINT('Ctrl Pts',(4.1312563510539,-4.58036770894347,21.9537491717274));
#37040=CARTESIAN_POINT('Ctrl Pts',(5.81915993678993,-2.04558671713384,22.0926955570125));
#37041=CARTESIAN_POINT('Ctrl Pts',(6.08861799204188,0.987814929143823,22.2316419422977));
#37042=CARTESIAN_POINT('Ctrl Pts',(4.87394894450772,3.78043239241062,22.3705883275827));
#37043=CARTESIAN_POINT('Ctrl Pts',(2.471233654691,5.65155302648554,22.5095347128679));
#37044=CARTESIAN_POINT('Ctrl Pts',(-0.533855580910739,6.14508304305042,
22.648481098153));
#37045=CARTESIAN_POINT('Ctrl Pts',(-3.40881519799501,5.14072235519228,22.7874274834382));
#37046=CARTESIAN_POINT('Ctrl Pts',(-5.45286129244639,2.88328824653298,22.9263738687233));
#37047=CARTESIAN_POINT('Ctrl Pts',(-6.16774874327281,-0.0769599058743887,
23.0653202540084));
#37048=CARTESIAN_POINT('Ctrl Pts',(-5.37922062671915,-3.0184487466801,23.2042666392935));
#37049=CARTESIAN_POINT('Ctrl Pts',(-3.27948409892758,-5.22417758428409,
23.3432130245786));
#37050=CARTESIAN_POINT('Ctrl Pts',(-0.380359066103212,-6.15649042621594,
23.4821594098638));
#37051=CARTESIAN_POINT('Ctrl Pts',(2.61148014250494,-5.58813196449027,23.6211057951489));
#37052=CARTESIAN_POINT('Ctrl Pts',(4.96675971427183,-3.65764204480724,23.760052180434));
#37053=CARTESIAN_POINT('Ctrl Pts',(6.11137001517765,-0.835585976930445,
23.8989985657192));
#37054=CARTESIAN_POINT('Ctrl Pts',(5.766307308755,2.19014780511587,24.0379449510043));
#37055=CARTESIAN_POINT('Ctrl Pts',(4.01568212968219,4.68202353909146,24.1768913362894));
#37056=CARTESIAN_POINT('Ctrl Pts',(1.28621697532681,6.03263568265451,24.3158377215745));
#37057=CARTESIAN_POINT('Ctrl Pts',(-1.75676915795036,5.91276665469978,24.4547841068596));
#37058=CARTESIAN_POINT('Ctrl Pts',(-4.37153517230061,4.351635051862,24.5937304921448));
#37059=CARTESIAN_POINT('Ctrl Pts',(-5.92072048533674,1.72977348857279,24.7326768774299));
#37060=CARTESIAN_POINT('Ctrl Pts',(-6.02670444269671,-1.31372788188239,
24.871623262715));
#37061=CARTESIAN_POINT('Ctrl Pts',(-4.66365299406171,-4.03700237035283,
25.0105696480002));
#37062=CARTESIAN_POINT('Ctrl Pts',(-2.163815855222,-5.77623998219821,25.1495160332853));
#37063=CARTESIAN_POINT('Ctrl Pts',(0.863460804436876,-6.10749398906431,
25.2884624185704));
#37064=CARTESIAN_POINT('Ctrl Pts',(3.68026513954963,-4.95001978681612,25.4274088038556));
#37065=CARTESIAN_POINT('Ctrl Pts',(5.59998884878251,-2.58595674379267,25.5663551891406));
#37066=CARTESIAN_POINT('Ctrl Pts',(6.15469093296995,0.408444496685631,25.7053015744258));
#37067=CARTESIAN_POINT('Ctrl Pts',(5.209160347801,3.3032856155884,25.8442479597109));
#37068=CARTESIAN_POINT('Ctrl Pts',(2.99387428363253,5.39293650630704,25.983194344996));
#37069=CARTESIAN_POINT('Ctrl Pts',(0.0488183484554523,6.16803568051526,
26.1221407302812));
#37070=CARTESIAN_POINT('Ctrl Pts',(-2.90813727137102,5.43964934514331,26.2610871155663));
#37071=CARTESIAN_POINT('Ctrl Pts',(-5.15622178962649,3.38532483573388,26.4000335008514));
#37072=CARTESIAN_POINT('Ctrl Pts',(-6.1474548325614,0.505812681605302,26.5389798861365));
#37073=CARTESIAN_POINT('Ctrl Pts',(-5.64021903706985,-2.49699351243254,
26.6779262714217));
#37074=CARTESIAN_POINT('Ctrl Pts',(-3.75815533325717,-4.89114668338274,
26.8168726567068));
#37075=CARTESIAN_POINT('Ctrl Pts',(-0.960024930259674,-6.09306158844103,
26.9558190419919));
#37076=CARTESIAN_POINT('Ctrl Pts',(2.07211572271754,-5.80976624477457,27.0947654272771));
#37077=CARTESIAN_POINT('Ctrl Pts',(4.5991691607941,-4.11031512388719,27.2337118125622));
#37078=CARTESIAN_POINT('Ctrl Pts',(6.00515512333616,-1.40895682401013,27.3726581978473));
#37079=CARTESIAN_POINT('Ctrl Pts',(5.94735842015232,1.63584082645554,27.5116045831324));
#37080=CARTESIAN_POINT('Ctrl Pts',(4.43986724888588,4.28189516447166,27.6505509684176));
#37081=CARTESIAN_POINT('Ctrl Pts',(1.85013913559806,5.8842189427471,27.7894973537027));
#37082=CARTESIAN_POINT('Ctrl Pts',(-1.19056843454766,6.05223877502484,27.9284437389878));
#37083=CARTESIAN_POINT('Ctrl Pts',(-3.94106977337074,4.74499909680486,28.0673901242729));
#37084=CARTESIAN_POINT('Ctrl Pts',(-5.73091822310212,2.28114526222492,28.206336509558));
#37085=CARTESIAN_POINT('Ctrl Pts',(-6.12383044364763,-0.738747646162098,
28.3452828948432));
#37086=CARTESIAN_POINT('Ctrl Pts',(-5.02403237325955,-3.57856760446066,
28.4842292801283));
#37087=CARTESIAN_POINT('Ctrl Pts',(-2.69960457241791,-5.54609615313651,
28.6231756654135));
#37088=CARTESIAN_POINT('Ctrl Pts',(0.282863578133191,-6.16173965560222,
28.7621220506985));
#37089=CARTESIAN_POINT('Ctrl Pts',(3.19638250190623,-5.27543233192912,28.9010684359837));
#37090=CARTESIAN_POINT('Ctrl Pts',(5.33076929616305,-3.10321544504092,29.0400148212688));
#37091=CARTESIAN_POINT('Ctrl Pts',(6.16575790162297,-0.174576303744733,
29.178961206554));
#37092=CARTESIAN_POINT('Ctrl Pts',(5.4978162160092,2.79661657047253,29.3179075918391));
#37093=CARTESIAN_POINT('Ctrl Pts',(3.48975792873298,5.08612199874332,29.4568539771242));
#37094=CARTESIAN_POINT('Ctrl Pts',(0.631055976348368,6.13586308044519,29.5958003624093));
#37095=CARTESIAN_POINT('Ctrl Pts',(-2.38146861347181,5.68996086368824,29.7347467476945));
#37096=CARTESIAN_POINT('Ctrl Pts',(-4.81349987651282,3.85710595214422,29.8736931329796));
#37097=CARTESIAN_POINT('Ctrl Pts',(-6.07221962036718,1.08406469792324,30.0126395182647));
#37098=CARTESIAN_POINT('Ctrl Pts',(-5.85080943581484,-1.95322203884639,
30.1515859035498));
#37099=CARTESIAN_POINT('Ctrl Pts',(-4.20323901781073,-4.51440241298987,
30.290532288835));
#37100=CARTESIAN_POINT('Ctrl Pts',(-1.53111081773288,-5.97517757485722,
30.42947867412));
#37101=CARTESIAN_POINT('Ctrl Pts',(1.514232299907,-5.97947722875285,30.5684250594052));
#37102=CARTESIAN_POINT('Ctrl Pts',(4.19047471207587,-4.52625331534901,30.7073714446903));
#37103=CARTESIAN_POINT('Ctrl Pts',(5.84527069718027,-1.96973548070316,30.8463178299755));
#37104=CARTESIAN_POINT('Ctrl Pts',(6.07525654045197,1.06691393980534,30.9852642152606));
#37105=CARTESIAN_POINT('Ctrl Pts',(4.82437219284485,3.84349844961081,31.1242106005457));
#37106=CARTESIAN_POINT('Ctrl Pts',(2.39752615168313,5.6832135046337,31.2631569858308));
#37107=CARTESIAN_POINT('Ctrl Pts',(-0.613727310998874,6.13762056296976,
31.402103371116));
#37108=CARTESIAN_POINT('Ctrl Pts',(-3.47538207375193,5.09595592884191,31.5410497564011));
#37109=CARTESIAN_POINT('Ctrl Pts',(-5.48989734854015,2.81212988493551,31.6799961416862));
#37110=CARTESIAN_POINT('Ctrl Pts',(-6.16622628003476,-0.157165042754142,
31.8189425269713));
#37111=CARTESIAN_POINT('Ctrl Pts',(-5.33951075118179,-3.08815030807591,
31.9578889122565));
#37112=CARTESIAN_POINT('Ctrl Pts',(-3.21126626587201,-5.26638551161304,
32.0968352975416));
#37113=CARTESIAN_POINT('Ctrl Pts',(-0.300261668879607,-6.16091635371372,
32.2357816828267));
#37114=CARTESIAN_POINT('Ctrl Pts',(2.68393301513983,-5.55369705308975,32.3747280681118));
#37115=CARTESIAN_POINT('Ctrl Pts',(5.01390735966058,-3.59273995385092,32.513674453397));
#37116=CARTESIAN_POINT('Ctrl Pts',(6.12171998980593,-0.756036873218341,
32.652620838682));
#37117=CARTESIAN_POINT('Ctrl Pts',(5.73733676131583,2.26495348175397,32.7915672239672));
#37118=CARTESIAN_POINT('Ctrl Pts',(3.95445275704879,4.73385157979469,32.9305136092523));
#37119=CARTESIAN_POINT('Ctrl Pts',(1.20765370324269,6.04885277720492,33.0694599945375));
#37120=CARTESIAN_POINT('Ctrl Pts',(-1.83351619040011,5.88941981580495,33.2084063798226));
#37121=CARTESIAN_POINT('Ctrl Pts',(-4.427758542337,4.29441517299123,33.3473527651077));
#37122=CARTESIAN_POINT('Ctrl Pts',(-5.9427155021103,1.65262816393567,33.4862991503928));
#37123=CARTESIAN_POINT('Ctrl Pts',(-6.00910972525653,-1.39199414405475,
33.625245535678));
#37124=CARTESIAN_POINT('Ctrl Pts',(-4.61075733126812,-4.09731182843245,
33.764191920963));
#37125=CARTESIAN_POINT('Ctrl Pts',(-2.08851279481842,-5.80389194361292,
33.9031383062483));
#37126=CARTESIAN_POINT('Ctrl Pts',(0.942815814134629,-6.09574816801622,
34.0420846915333));
#37127=CARTESIAN_POINT('Ctrl Pts',(3.74432896997149,-4.90173927824479,34.1810310768185));
#37128=CARTESIAN_POINT('Ctrl Pts',(5.63314566277761,-2.51291013153774,34.3199774621036));
#37129=CARTESIAN_POINT('Ctrl Pts',(6.14885861299432,0.488451783353388,34.4589238473887));
#37130=CARTESIAN_POINT('Ctrl Pts',(5.16576054720173,3.37075145275196,34.5978702326739));
#37131=CARTESIAN_POINT('Ctrl Pts',(2.92348589246469,5.43141580288374,34.736816617959));
#37132=CARTESIAN_POINT('Ctrl Pts',(-0.0314011569553952,6.16814894069502,
34.8757630032441));
#37133=CARTESIAN_POINT('Ctrl Pts',(-2.97863403786675,5.40136896126499,35.0147093885292));
#37134=CARTESIAN_POINT('Ctrl Pts',(-5.19981192392431,3.31798181777267,35.1536557738144));
#37135=CARTESIAN_POINT('Ctrl Pts',(-6.1535130499399,0.425822182929395,35.2926021590995));
#37136=CARTESIAN_POINT('Ctrl Pts',(-5.60726862070789,-2.57013346005217,
35.4315485443846));
#37137=CARTESIAN_POINT('Ctrl Pts',(-3.69422809037848,-4.93960789977443,
35.5704949296698));
#37138=CARTESIAN_POINT('Ctrl Pts',(-0.880703404207672,-6.10503144144831,
35.7094413149548));
#37139=CARTESIAN_POINT('Ctrl Pts',(2.14749656515694,-5.78232703069399,35.84838770024));
#37140=CARTESIAN_POINT('Ctrl Pts',(4.65223491159577,-4.05015527042914,35.9873340855251));
#37141=CARTESIAN_POINT('Ctrl Pts',(6.02297077506532,-1.3307405569699,36.1262804708102));
#37142=CARTESIAN_POINT('Ctrl Pts',(5.92558133025528,1.71304795198071,36.2652268560954));
#37143=CARTESIAN_POINT('Ctrl Pts',(4.38380567769012,4.3392735760156,36.4041732413805));
#37144=CARTESIAN_POINT('Ctrl Pts',(1.77345833478221,5.90778240307198,36.5431196266656));
#37145=CARTESIAN_POINT('Ctrl Pts',(-1.26917718645326,6.03624358824607,36.6820660119508));
#37146=CARTESIAN_POINT('Ctrl Pts',(-4.00244525137675,4.69334415923093,36.8210123972359));
#37147=CARTESIAN_POINT('Ctrl Pts',(-5.7600998876454,2.20642168943353,36.959958782521));
#37148=CARTESIAN_POINT('Ctrl Pts',(-6.11370513714305,-0.818325658479648,
37.0989051678061));
#37149=CARTESIAN_POINT('Ctrl Pts',(-4.97706818318234,-3.64360256987634,
37.2378515530912));
#37150=CARTESIAN_POINT('Ctrl Pts',(-2.62724922425273,-5.58073551612318,
37.3767979383764));
#37151=CARTESIAN_POINT('Ctrl Pts',(0.362973153742378,-6.15753992085458,
37.5157443236615));
#37152=CARTESIAN_POINT('Ctrl Pts',(3.26471924766826,-5.23341720304809,37.6546907089466));
#37153=CARTESIAN_POINT('Ctrl Pts',(5.37067583323858,-3.03362629233108,37.7936370942318));
#37154=CARTESIAN_POINT('Ctrl Pts',(6.16750683812607,-0.0943757856832029,
37.9325834795169));
#37155=CARTESIAN_POINT('Ctrl Pts',(5.46098124106467,2.86787922897654,38.071529864802));
#37156=CARTESIAN_POINT('Ctrl Pts',(3.42331772760518,5.13107621490068,38.2104762500871));
#37157=CARTESIAN_POINT('Ctrl Pts',(0.551205636877804,6.14355106865155,38.3494226353723));
#37158=CARTESIAN_POINT('Ctrl Pts',(-2.45526522392973,5.65850864339859,38.4883690206574));
#37159=CARTESIAN_POINT('Ctrl Pts',(-4.8632545133651,3.79418013877694,38.6273154059425));
#37160=CARTESIAN_POINT('Ctrl Pts',(-6.08580437459756,1.00500373202518,38.7662617912276));
#37161=CARTESIAN_POINT('Ctrl Pts',(-5.82491296452679,-2.02914670315951,
38.9052081765128));
#37162=CARTESIAN_POINT('Ctrl Pts',(-4.14417369845267,-4.56868380874715,
39.0441545617979));
#37163=CARTESIAN_POINT('Ctrl Pts',(-1.45327407865533,-5.99458437588159,
39.183100947083));
#37164=CARTESIAN_POINT('Ctrl Pts',(1.59186741519754,-5.95927894293327,39.3220473323681));
#37165=CARTESIAN_POINT('Ctrl Pts',(4.24898430674745,-4.47137336265596,39.4609937176533));
#37166=CARTESIAN_POINT('Ctrl Pts',(5.87039280319046,-1.89355108816871,39.5999401029384));
#37167=CARTESIAN_POINT('Ctrl Pts',(6.06086753525496,1.14583249532731,39.7388864882236));
#37168=CARTESIAN_POINT('Ctrl Pts',(4.7739794590064,3.90591442715279,39.8778328735086));
#37169=CARTESIAN_POINT('Ctrl Pts',(2.32341313713361,5.71391273834754,40.0167792587938));
#37170=CARTESIAN_POINT('Ctrl Pts',(-0.693495236793662,6.12911998118813,
40.1557256440789));
#37171=CARTESIAN_POINT('Ctrl Pts',(-3.5413611321283,5.05032758532616,40.294672029364));
#37172=CARTESIAN_POINT('Ctrl Pts',(-5.52600485720787,2.74049588676401,40.4336184146491));
#37173=CARTESIAN_POINT('Ctrl Pts',(-6.16366087679677,-0.237343597134103,
40.5725647999343));
#37174=CARTESIAN_POINT('Ctrl Pts',(-5.29889776422902,-3.15732954749802,
40.7115111852194));
#37175=CARTESIAN_POINT('Ctrl Pts',(-3.14250528731887,-5.3077026957459,40.8504575705046));
#37176=CARTESIAN_POINT('Ctrl Pts',(-0.220113486152523,-6.16430023931905,
40.9894039557896));
#37177=CARTESIAN_POINT('Ctrl Pts',(2.75593193409692,-5.51832280334161,41.1283503410748));
#37178=CARTESIAN_POINT('Ctrl Pts',(5.06020696537266,-3.52723019589728,41.2672967263599));
#37179=CARTESIAN_POINT('Ctrl Pts',(6.1310345521162,-0.676359895331296,41.406243111645));
#37180=CARTESIAN_POINT('Ctrl Pts',(5.70739581517076,2.33937606985853,41.5451894969302));
#37181=CARTESIAN_POINT('Ctrl Pts',(3.89255453822456,4.78487894875124,41.6841358822153));
#37182=CARTESIAN_POINT('Ctrl Pts',(1.12888617164935,6.06404678401431,41.8230822675004));
#37183=CARTESIAN_POINT('Ctrl Pts',(-1.90995310653424,5.86507685525906,41.9620286527856));
#37184=CARTESIAN_POINT('Ctrl Pts',(-4.4832330124328,4.23646894754202,42.1009750380707));
#37185=CARTESIAN_POINT('Ctrl Pts',(-5.96370538293448,1.57520331792875,42.2399214233557));
#37186=CARTESIAN_POINT('Ctrl Pts',(-5.9904986421152,-1.47002496783944,42.3788678086409));
#37187=CARTESIAN_POINT('Ctrl Pts',(-4.55708181657933,-4.15692827749739,
42.517814193926));
#37188=CARTESIAN_POINT('Ctrl Pts',(-2.01285648861499,-5.83056224934576,
42.6567605792111));
#37189=CARTESIAN_POINT('Ctrl Pts',(1.02201135833755,-6.08297132745868,42.7957069644963));
#37190=CARTESIAN_POINT('Ctrl Pts',(3.80775949401135,-4.85262970182371,42.9346533497814));
#37191=CARTESIAN_POINT('Ctrl Pts',(5.6653497006872,-2.43943849198514,43.0735997350666));
#37192=CARTESIAN_POINT('Ctrl Pts',(6.14198629054217,0.568376454515263,43.2125461203516));
#37193=CARTESIAN_POINT('Ctrl Pts',(5.12148702285964,3.43764716949481,43.3514925056368));
#37194=CARTESIAN_POINT('Ctrl Pts',(2.85260303024805,5.46897644345585,43.4904388909219));
#37195=CARTESIAN_POINT('Ctrl Pts',(-0.111615351253502,6.16721893568081,
43.6293852762071));
#37196=CARTESIAN_POINT('Ctrl Pts',(-3.04862700569499,5.36217500342934,43.7683316614921));
#37197=CARTESIAN_POINT('Ctrl Pts',(-5.24252257511504,3.25007760471418,43.9072780467774));
#37198=CARTESIAN_POINT('Ctrl Pts',(-6.15853047760213,0.345759661760731,
44.0462244320624));
#37199=CARTESIAN_POINT('Ctrl Pts',(-5.57336980503824,-2.64283870176434,
44.1851708173476));
#37200=CARTESIAN_POINT('Ctrl Pts',(-3.62967601505457,-4.98723364331296,
44.3241172026326));
#37201=CARTESIAN_POINT('Ctrl Pts',(-0.801232918197713,-6.11596870479661,
44.4630635879178));
#37202=CARTESIAN_POINT('Ctrl Pts',(2.22251418542987,-5.7539098083667,44.6020099732029));
#37203=CARTESIAN_POINT('Ctrl Pts',(4.70451379508847,-3.98931038389815,44.7409563584881));
#37204=CARTESIAN_POINT('Ctrl Pts',(6.03976771667011,-1.25229921181993,44.8799027437731));
#37205=CARTESIAN_POINT('Ctrl Pts',(5.90280200243972,1.78996533688478,45.0188491290584));
#37206=CARTESIAN_POINT('Ctrl Pts',(4.32700264063096,4.39591805374351,45.1577955143434));
#37207=CARTESIAN_POINT('Ctrl Pts',(1.69647757568547,5.93034663594394,45.2967418996286));
#37208=CARTESIAN_POINT('Ctrl Pts',(-1.34757127292229,6.01922744641287,45.4356882849136));
#37209=CARTESIAN_POINT('Ctrl Pts',(-4.06314376586214,4.64089540123354,45.5746346701989));
#37210=CARTESIAN_POINT('Ctrl Pts',(-5.78830730338494,2.13132492802865,45.7135810554838));
#37211=CARTESIAN_POINT('Ctrl Pts',(-6.10254577393243,-0.897765261254136,
45.8525274407692));
#37212=CARTESIAN_POINT('Ctrl Pts',(-4.92926218431401,-3.70802126551977,
45.9914738260541));
#37213=CARTESIAN_POINT('Ctrl Pts',(-2.55444950976324,-5.61443096754502,
46.1304202113394));
#37214=CARTESIAN_POINT('Ctrl Pts',(0.443021336985154,-6.15229871529521,
46.2693665966244));
#37215=CARTESIAN_POINT('Ctrl Pts',(3.33250380703052,-5.19051690714888,46.4083129819096));
#37216=CARTESIAN_POINT('Ctrl Pts',(5.40967398771416,-2.96352403969991,46.5472593671947));
#37217=CARTESIAN_POINT('Ctrl Pts',(6.16821261804079,-0.0141593051434131,
46.6862057524798));
#37218=CARTESIAN_POINT('Ctrl Pts',(5.42322260948793,2.93865682161187,46.8251521377649));
#37219=CARTESIAN_POINT('Ctrl Pts',(3.35629851513677,5.17516257371816,46.9640985230501));
#37220=CARTESIAN_POINT('Ctrl Pts',(0.471262067857944,6.15019995212064,47.1030449083352));
#37221=CARTESIAN_POINT('Ctrl Pts',(-2.52864655697621,5.62609935712526,47.2419912936204));
#37222=CARTESIAN_POINT('Ctrl Pts',(-4.91218659163945,3.73061258745804,47.3809376789054));
#37223=CARTESIAN_POINT('Ctrl Pts',(-6.09835979107824,0.925772782067534,
47.5198840641906));
#37224=CARTESIAN_POINT('Ctrl Pts',(-5.79803128232603,-2.10472816220254,
47.6588304494757));
#37225=CARTESIAN_POINT('Ctrl Pts',(-4.08440744356784,-4.62219246979801,
47.7977768347608));
#37226=CARTESIAN_POINT('Ctrl Pts',(-1.3751915372633,-6.01297726607435,47.9367232200459));
#37227=CARTESIAN_POINT('Ctrl Pts',(1.66923328761391,-5.93807272339738,48.0756696053311));
#37228=CARTESIAN_POINT('Ctrl Pts',(4.30677523582703,-4.41573712583598,48.2146159906162));
#37229=CARTESIAN_POINT('Ctrl Pts',(5.89452201173586,-1.81704643939022,48.3535623759014));
#37230=CARTESIAN_POINT('Ctrl Pts',(6.04545339844714,1.22455727539131,48.4925087611865));
#37231=CARTESIAN_POINT('Ctrl Pts',(4.72277928918092,3.9676697139446,48.6314551464715));
#37232=CARTESIAN_POINT('Ctrl Pts',(2.24890710164729,5.7436456410697,48.7704015317568));
#37233=CARTESIAN_POINT('Ctrl Pts',(-0.773145779312667,6.11958252885515,
48.9093479170418));
#37234=CARTESIAN_POINT('Ctrl Pts',(-3.60674138390151,5.0038454454835,49.0482943023269));
#37235=CARTESIAN_POINT('Ctrl Pts',(-5.56117737882469,2.66839758051078,49.1872406876122));
#37236=CARTESIAN_POINT('Ctrl Pts',(-6.16005361658189,-0.317480470389693,
49.3261870728971));
#37237=CARTESIAN_POINT('Ctrl Pts',(-5.25738726777968,-3.22597776563184,
49.4651334581824));
#37238=CARTESIAN_POINT('Ctrl Pts',(-3.07321526737865,-5.34811628862904,
49.6040798434674));
#37239=CARTESIAN_POINT('Ctrl Pts',(-0.139923243902764,-6.16665295081448,
49.7430262287525));
#37240=CARTESIAN_POINT('Ctrl Pts',(2.82745529157474,-5.48199286181392,49.8819726140377));
#37241=CARTESIAN_POINT('Ctrl Pts',(5.10566911489767,-3.46116748161068,50.0209189993228));
#37242=CARTESIAN_POINT('Ctrl Pts',(6.13927613085879,-0.596483094503927,
50.159865384608));
#37243=CARTESIAN_POINT('Ctrl Pts',(5.67656028959098,2.41323360786418,50.2988117698931));
#37244=CARTESIAN_POINT('Ctrl Pts',(3.82978111916535,4.83555167229963,50.4377636931423));
#37245=CARTESIAN_POINT('Ctrl Pts',(1.97657001493401,5.6633953183859,50.5304001546298));
#37246=CARTESIAN_POINT('Ctrl Pts',(1.00683925828395,5.83084219161743,50.5767211543557));
#37247=CARTESIAN_POINT('',(-2.85720427747916,-4.00332290438391,-6.57838495879084E-5));
#37248=CARTESIAN_POINT('Ctrl Pts',(-2.85727392025667,-4.0034136718698,-1.90440111597079E-16));
#37249=CARTESIAN_POINT('Ctrl Pts',(-2.96392441703552,-3.94219184122042,
-3.79761926524811E-15));
#37250=CARTESIAN_POINT('Ctrl Pts',(-3.06811942088831,-3.87701250322895,
-4.52675719847336E-15));
#37251=CARTESIAN_POINT('Ctrl Pts',(-3.1696245436634,-3.8080049793148,-3.87190279838023E-15));
#37252=CARTESIAN_POINT('Ctrl Pts',(-3.28894064367922,-3.7268887912833,-2.80322714571153E-15));
#37253=CARTESIAN_POINT('Ctrl Pts',(-3.40454111778736,-3.64048431718383,
-1.35958250046822E-15));
#37254=CARTESIAN_POINT('Ctrl Pts',(-3.51620782247888,-3.54916472775186,
-2.47718512369488E-15));
#37255=CARTESIAN_POINT('Ctrl Pts',(-3.62942802187464,-3.45657471040703,
-3.61033570959694E-15));
#37256=CARTESIAN_POINT('Ctrl Pts',(-3.73860485228503,-3.35893149262313,
-9.2527721805512E-15));
#37257=CARTESIAN_POINT('Ctrl Pts',(-3.84348814314742,-3.25657606743181,
-3.27515792264421E-15));
#37258=CARTESIAN_POINT('Ctrl Pts',(-3.85907125732511,-3.24136853280597,
-2.38702936827464E-15));
#37259=CARTESIAN_POINT('Ctrl Pts',(-3.87455954225653,-3.22605689833688,
-1.45446846519406E-15));
#37260=CARTESIAN_POINT('Ctrl Pts',(-3.88995212208754,-3.2106422018724,-1.17961196366423E-15));
#37261=CARTESIAN_POINT('Ctrl Pts',(-3.90663484725527,-3.1939355063422,-9.37983998556092E-16));
#37262=CARTESIAN_POINT('Ctrl Pts',(-3.92319901111119,-3.17711387554321,
-2.16429627180207E-15));
#37263=CARTESIAN_POINT('Ctrl Pts',(-3.93964133836745,-3.16018139905906,
-1.87350135405495E-15));
#37264=CARTESIAN_POINT('Ctrl Pts',(-4.04344251084588,-3.05328589183402,
-1.39830370429894E-15));
#37265=CARTESIAN_POINT('Ctrl Pts',(-4.14242071302894,-2.9419456343137,-1.86698229125925E-15));
#37266=CARTESIAN_POINT('Ctrl Pts',(-4.23634450385737,-2.82655565829915,
-2.41473507855972E-15));
#37267=CARTESIAN_POINT('Ctrl Pts',(-4.33083320912257,-2.71047165723798,
-1.95593090836767E-15));
#37268=CARTESIAN_POINT('Ctrl Pts',(-4.42020713177466,-2.59028858558435,
-3.66802097409348E-15));
#37269=CARTESIAN_POINT('Ctrl Pts',(-4.50420315680805,-2.46636346404815,
-3.10862446895044E-15));
#37270=CARTESIAN_POINT('Ctrl Pts',(-4.56394529362918,-2.37822177444499,
-3.71351768609898E-15));
#37271=CARTESIAN_POINT('Ctrl Pts',(-4.62096632907673,-2.28818610926391,
-4.00301393197316E-15));
#37272=CARTESIAN_POINT('Ctrl Pts',(-4.6751605977512,-2.19637326218911,-2.13717932240343E-15));
#37273=CARTESIAN_POINT('Ctrl Pts',(-4.69349550832276,-2.16531129970469,
-2.68638171010596E-15));
#37274=CARTESIAN_POINT('Ctrl Pts',(-4.71151113780902,-2.13403784574948,
-3.5495951981545E-15));
#37275=CARTESIAN_POINT('Ctrl Pts',(-4.7291814375198,-2.10259654657166,-3.27515792264421E-15));
#37276=CARTESIAN_POINT('Ctrl Pts',(-4.76374095187582,-2.04110375651751,
-2.73841439717669E-15));
#37277=CARTESIAN_POINT('Ctrl Pts',(-4.79699068953928,-1.97895180212665,
-2.25062029132347E-15));
#37278=CARTESIAN_POINT('Ctrl Pts',(-4.82890821417569,-1.91618085442916,
-1.47104550762833E-15));
#37279=CARTESIAN_POINT('Ctrl Pts',(-4.89653151535774,-1.78318875212848,
-3.27759312618307E-16));
#37280=CARTESIAN_POINT('Ctrl Pts',(-4.95817727267847,-1.647420621107,-2.18395141942288E-15));
#37281=CARTESIAN_POINT('Ctrl Pts',(-5.01386176575433,-1.50932773275128,
-2.88657986402541E-15));
#37282=CARTESIAN_POINT('Ctrl Pts',(-5.07040880353274,-1.36909580563034,
-4.46478699491984E-15));
#37283=CARTESIAN_POINT('Ctrl Pts',(-5.12080880180208,-1.22646596455888,
-1.93984784978018E-15));
#37284=CARTESIAN_POINT('Ctrl Pts',(-5.1650385546073,-1.08187495549977,-8.88178419700125E-16));
#37285=CARTESIAN_POINT('Ctrl Pts',(-5.20789090131116,-0.941786809908098,
1.14310558333649E-15));
#37286=CARTESIAN_POINT('Ctrl Pts',(-5.24495133489085,-0.799856998147732,
-7.25711619033519E-17));
#37287=CARTESIAN_POINT('Ctrl Pts',(-5.27615924986373,-0.656459529145883,
6.38378239159465E-16));
#37288=CARTESIAN_POINT('Ctrl Pts',(-5.2995651860934,-0.548911427394497,
1.17159028995658E-15));
#37289=CARTESIAN_POINT('Ctrl Pts',(-5.31967830443972,-0.44053724444289,
-1.8825369533321E-16));
#37290=CARTESIAN_POINT('Ctrl Pts',(-5.33645757909966,-0.33148943554366,
8.32667268468867E-17));
#37291=CARTESIAN_POINT('Ctrl Pts',(-5.34173742775273,-0.297175918505209,
1.68704671238542E-16));
#37292=CARTESIAN_POINT('Ctrl Pts',(-5.34668707696921,-0.262795679428468,
-5.27690249084824E-16));
#37293=CARTESIAN_POINT('Ctrl Pts',(-5.35130496264844,-0.228353414454299,
-1.22124532708767E-15));
#37294=CARTESIAN_POINT('Ctrl Pts',(-5.35416327631062,-0.207034827687464,
-1.65053225461906E-15));
#37295=CARTESIAN_POINT('Ctrl Pts',(-5.3568934937129,-0.18569960650873,-1.7557947277759E-15));
#37296=CARTESIAN_POINT('Ctrl Pts',(-5.35949458805709,-0.164356971876369,
-1.55431223447522E-15));
#37297=CARTESIAN_POINT('Ctrl Pts',(-5.36550318946691,-0.115054882996834,
-1.08888198354834E-15));
#37298=CARTESIAN_POINT('Ctrl Pts',(-5.37082454994926,-0.0657002470660596,
-2.6297948742482E-15));
#37299=CARTESIAN_POINT('Ctrl Pts',(-5.37545897566846,-0.0163081375275379,
-2.55351295663786E-15));
#37300=CARTESIAN_POINT('Ctrl Pts',(-5.39010486966895,0.139782745052889,
-2.31244384750334E-15));
#37301=CARTESIAN_POINT('Ctrl Pts',(-5.39789366413514,0.296245517049997,
-1.69829426269487E-16));
#37302=CARTESIAN_POINT('Ctrl Pts',(-5.3988048329656,0.45261913524857,-4.44089209850063E-16));
#37303=CARTESIAN_POINT('Ctrl Pts',(-5.39920138612075,0.520675075713029,
-5.63450824156723E-16));
#37304=CARTESIAN_POINT('Ctrl Pts',(-5.39829465303725,0.588714457569937,
-4.03889576939982E-16));
#37305=CARTESIAN_POINT('Ctrl Pts',(-5.39608014451778,0.656700546464023,
-8.88178419700125E-16));
#37306=CARTESIAN_POINT('Ctrl Pts',(-5.39103330518352,0.81164005769026,-2.2239734044486E-15));
#37307=CARTESIAN_POINT('Ctrl Pts',(-5.37919775368595,0.966302252665731,
-2.50379637210522E-15));
#37308=CARTESIAN_POINT('Ctrl Pts',(-5.36076192524352,1.12029164381784,-1.55431223447522E-15));
#37309=CARTESIAN_POINT('Ctrl Pts',(-5.34439112180454,1.25703245056332,-7.11181249930206E-16));
#37310=CARTESIAN_POINT('Ctrl Pts',(-5.32281505665169,1.3932432519743,-1.27921867688379E-15));
#37311=CARTESIAN_POINT('Ctrl Pts',(-5.29613177430492,1.52864937240809,-9.99200722162641E-16));
#37312=CARTESIAN_POINT('Ctrl Pts',(-5.28279013313154,1.59635243262499,-8.59191744802064E-16));
#37313=CARTESIAN_POINT('Ctrl Pts',(-5.26817119586974,1.66385431563014,-1.01692553827192E-15));
#37314=CARTESIAN_POINT('Ctrl Pts',(-5.25228430581433,1.73112039267501,-6.66133814775094E-16));
#37315=CARTESIAN_POINT('Ctrl Pts',(-5.24284045247573,1.77110625296983,-4.57608069487945E-16));
#37316=CARTESIAN_POINT('Ctrl Pts',(-5.23294851526294,1.8110087825455,1.63983992970298E-15));
#37317=CARTESIAN_POINT('Ctrl Pts',(-5.22261013722243,1.85082063743615,7.7715611723761E-16));
#37318=CARTESIAN_POINT('Ctrl Pts',(-5.21644087173432,1.87457773951079,2.62363037458145E-16));
#37319=CARTESIAN_POINT('Ctrl Pts',(-5.21011245680572,1.89830284226968,-2.1845483731124E-15));
#37320=CARTESIAN_POINT('Ctrl Pts',(-5.20363101472144,1.9219741450254,-2.99760216648792E-15));
#37321=CARTESIAN_POINT('Ctrl Pts',(-5.2027022220642,1.92536625003855,-3.11411302678728E-15));
#37322=CARTESIAN_POINT('Ctrl Pts',(-5.20177026797345,1.9287573266952,-2.51008778115122E-15));
#37323=CARTESIAN_POINT('Ctrl Pts',(-5.2008351599293,1.93214735386067,-2.55351295663786E-15));
#37324=CARTESIAN_POINT('Ctrl Pts',(-5.15837246026862,2.08608646952665,-3.29752994359241E-15));
#37325=CARTESIAN_POINT('Ctrl Pts',(-5.10939283443341,2.2379254056552,-9.6917886872663E-16));
#37326=CARTESIAN_POINT('Ctrl Pts',(-5.05412742134996,2.38725197436616,-1.4432899320127E-15));
#37327=CARTESIAN_POINT('Ctrl Pts',(-4.99560914757004,2.54536773869149,1.84033906423277E-16));
#37328=CARTESIAN_POINT('Ctrl Pts',(-4.93004375984936,2.70066753913477,-2.81809918376493E-16));
#37329=CARTESIAN_POINT('Ctrl Pts',(-4.85764295714644,2.85266553503319,-8.88178419700125E-16));
#37330=CARTESIAN_POINT('Ctrl Pts',(-4.78524215444354,3.00466353093158,-1.1729133274605E-16));
#37331=CARTESIAN_POINT('Ctrl Pts',(-4.70600574477678,3.15336070488546,-8.50437032510622E-16));
#37332=CARTESIAN_POINT('Ctrl Pts',(-4.62008381109869,3.29826043492649,4.44089209850063E-16));
#37333=CARTESIAN_POINT('Ctrl Pts',(-4.55853244340741,3.40206136421584,1.38317739444463E-15));
#37334=CARTESIAN_POINT('Ctrl Pts',(-4.4935489092733,3.50391333587595,-2.37538502008119E-15));
#37335=CARTESIAN_POINT('Ctrl Pts',(-4.42526788724923,3.60369937507567,1.11022302462516E-16));
#37336=CARTESIAN_POINT('Ctrl Pts',(-4.39539494011371,3.64735576722555,1.16321000706569E-15));
#37337=CARTESIAN_POINT('Ctrl Pts',(-4.36489064048442,3.69061662547834,-4.70458545952692E-16));
#37338=CARTESIAN_POINT('Ctrl Pts',(-4.33376540259314,3.73347163408685,-1.60982338570648E-15));
#37339=CARTESIAN_POINT('Ctrl Pts',(-4.3144372096508,3.76008379614724,-1.89151283622047E-15));
#37340=CARTESIAN_POINT('Ctrl Pts',(-4.29486956173448,3.78653944869874,-2.67178752123484E-15));
#37341=CARTESIAN_POINT('Ctrl Pts',(-4.2750648569809,3.8128360516663,-1.49880108324396E-15));
#37342=CARTESIAN_POINT('Ctrl Pts',(-4.25977487047579,3.83313803089331,-5.93210869670195E-16));
#37343=CARTESIAN_POINT('Ctrl Pts',(-4.24434478058479,3.85334347519376,-6.91837681892335E-16));
#37344=CARTESIAN_POINT('Ctrl Pts',(-4.22878820767209,3.87343556296813,-7.7715611723761E-16));
#37345=CARTESIAN_POINT('Ctrl Pts',(-4.12984945342294,4.00121988576316,-1.31977561029168E-15));
#37346=CARTESIAN_POINT('Ctrl Pts',(-4.02566840201076,4.12459437000251,-1.20137809397138E-15));
#37347=CARTESIAN_POINT('Ctrl Pts',(-3.91664624574708,4.24332609595032,-7.21644966006352E-16));
#37348=CARTESIAN_POINT('Ctrl Pts',(-3.80538717710434,4.36449395485185,-2.32068692305071E-16));
#37349=CARTESIAN_POINT('Ctrl Pts',(-3.68908600787891,4.48082719185148,-2.27264911948676E-15));
#37350=CARTESIAN_POINT('Ctrl Pts',(-3.56811826615625,4.59205972744533,-9.99200722162641E-16));
#37351=CARTESIAN_POINT('Ctrl Pts',(-3.44670691496372,4.70370017183738,2.78917628988849E-16));
#37352=CARTESIAN_POINT('Ctrl Pts',(-3.32059424074317,4.81020303581451,2.41120170451567E-16));
#37353=CARTESIAN_POINT('Ctrl Pts',(-3.19011516755566,4.91127172518233,-3.33066907387547E-16));
#37354=CARTESIAN_POINT('Ctrl Pts',(-3.06067297799998,5.01153724767336,-9.02691068215667E-16));
#37355=CARTESIAN_POINT('Ctrl Pts',(-2.92693298103373,5.10645516017338,-1.40885470584828E-15));
#37356=CARTESIAN_POINT('Ctrl Pts',(-2.78918574631266,5.19570037385525,-7.7715611723761E-16));
#37357=CARTESIAN_POINT('Ctrl Pts',(-2.72171518373931,5.23941395392303,-4.67741127988239E-16));
#37358=CARTESIAN_POINT('Ctrl Pts',(-2.65328270595906,5.28176595923915,-2.19182071710708E-16));
#37359=CARTESIAN_POINT('Ctrl Pts',(-2.583919816344,5.32271443393357,-4.44089209850063E-16));
#37360=CARTESIAN_POINT('Ctrl Pts',(-2.85714359587721,-4.00323788139524,
-6.57838495876639E-5));
#37361=CARTESIAN_POINT('Ctrl Pts',(-2.85654553762487,-4.00366472045808,
-4.38558997250773E-5));
#37362=CARTESIAN_POINT('Ctrl Pts',(-2.85594738372198,-4.00409142550178,
-2.19279498625866E-5));
#37363=CARTESIAN_POINT('Ctrl Pts',(-2.85534913422859,-4.00451799648348,
0.));
#37364=CARTESIAN_POINT('Origin',(0.959402651837398,0.906858060794113,49.9999999999962));
#37365=CARTESIAN_POINT('Origin',(-2.88675134594813,-5.,-12.));
#37366=CARTESIAN_POINT('',(-2.88675134594813,-5.,-12.));
#37367=CARTESIAN_POINT('',(2.88675134594813,-5.,-12.));
#37368=CARTESIAN_POINT('',(-1.44337567297407,-5.,-12.));
#37369=CARTESIAN_POINT('',(-2.88675134594813,-5.,-6.));
#37370=CARTESIAN_POINT('',(-2.88675134594813,-5.,-12.));
#37371=CARTESIAN_POINT('',(2.88675134594813,-5.,-6.));
#37372=CARTESIAN_POINT('',(-2.88675134594813,-5.,-6.));
#37373=CARTESIAN_POINT('',(2.88675134594813,-5.,-12.));
#37374=CARTESIAN_POINT('Origin',(-5.77350269189626,7.07050159149938E-16,
-12.));
#37375=CARTESIAN_POINT('',(-5.77350269189626,7.07050159149938E-16,-12.));
#37376=CARTESIAN_POINT('',(-5.05181485540923,-1.25,-12.));
#37377=CARTESIAN_POINT('',(-5.77350269189626,1.11022302462516E-15,-6.));
#37378=CARTESIAN_POINT('',(-5.77350269189626,7.07050159149938E-16,-12.));
#37379=CARTESIAN_POINT('',(-5.77350269189626,7.07050159149938E-16,-6.));
#37380=CARTESIAN_POINT('Origin',(-2.88675134594813,5.,-12.));
#37381=CARTESIAN_POINT('',(-2.88675134594813,5.,-12.));
#37382=CARTESIAN_POINT('',(-3.60843918243516,3.75,-12.));
#37383=CARTESIAN_POINT('',(-2.88675134594813,5.,-6.));
#37384=CARTESIAN_POINT('',(-2.88675134594813,5.,-12.));
#37385=CARTESIAN_POINT('',(-2.88675134594813,5.,-6.));
#37386=CARTESIAN_POINT('Origin',(2.88675134594813,5.,-12.));
#37387=CARTESIAN_POINT('',(2.88675134594813,5.,-12.));
#37388=CARTESIAN_POINT('',(1.44337567297407,5.,-12.));
#37389=CARTESIAN_POINT('',(2.88675134594813,5.,-6.));
#37390=CARTESIAN_POINT('',(2.88675134594813,5.,-12.));
#37391=CARTESIAN_POINT('',(2.88675134594813,5.,-6.));
#37392=CARTESIAN_POINT('Origin',(5.77350269189626,0.,-12.));
#37393=CARTESIAN_POINT('',(5.77350269189626,0.,-12.));
#37394=CARTESIAN_POINT('',(5.05181485540923,1.25,-12.));
#37395=CARTESIAN_POINT('',(5.77350269189626,0.,-6.));
#37396=CARTESIAN_POINT('',(5.77350269189626,0.,-12.));
#37397=CARTESIAN_POINT('',(5.77350269189626,0.,-6.));
#37398=CARTESIAN_POINT('Origin',(2.88675134594813,-5.,-12.));
#37399=CARTESIAN_POINT('',(3.60843918243516,-3.75,-12.));
#37400=CARTESIAN_POINT('',(2.88675134594813,-5.,-6.));
#37401=CARTESIAN_POINT('Origin',(0.,0.,-6.));
#37402=CARTESIAN_POINT('Origin',(0.,0.,0.));
#37403=CARTESIAN_POINT('',(-9.,-1.10218211923262E-15,0.));
#37404=CARTESIAN_POINT('Origin',(0.,0.,0.));
#37405=CARTESIAN_POINT('Origin',(0.,0.,-12.));
#37406=CARTESIAN_POINT('',(-9.,-1.10218211923262E-15,-12.));
#37407=CARTESIAN_POINT('',(-9.,-1.10218211923262E-15,-12.));
#37408=CARTESIAN_POINT('Origin',(0.,0.,-12.));
#37409=CARTESIAN_POINT('Origin',(0.,0.,-12.));
#37410=CARTESIAN_POINT('Origin',(0.,0.,50.));
#37411=CARTESIAN_POINT('',(0.,0.,0.));
#37412=CARTESIAN_POINT('Origin',(55.,0.,25.));
#37413=CARTESIAN_POINT('',(55.,10.,20.));
#37414=CARTESIAN_POINT('',(60.,10.,25.));
#37415=CARTESIAN_POINT('Origin',(55.,10.,25.));
#37416=CARTESIAN_POINT('',(60.,0.,25.));
#37417=CARTESIAN_POINT('',(60.,0.,25.));
#37418=CARTESIAN_POINT('',(55.,0.,20.));
#37419=CARTESIAN_POINT('Origin',(55.,0.,25.));
#37420=CARTESIAN_POINT('',(55.,0.,20.));
#37421=CARTESIAN_POINT('Origin',(60.,0.,20.));
#37422=CARTESIAN_POINT('',(0.,0.,20.));
#37423=CARTESIAN_POINT('',(60.,0.,20.));
#37424=CARTESIAN_POINT('',(0.,10.,20.));
#37425=CARTESIAN_POINT('',(0.,0.,20.));
#37426=CARTESIAN_POINT('',(60.,10.,20.));
#37427=CARTESIAN_POINT('Origin',(24.,0.,37.));
#37428=CARTESIAN_POINT('',(60.,0.,36.0323593997502));
#37429=CARTESIAN_POINT('',(60.,0.,40.));
#37430=CARTESIAN_POINT('',(56.1361480780321,0.,40.9015654484592));
#37431=CARTESIAN_POINT('Origin',(55.,0.,36.0323593997502));
#37432=CARTESIAN_POINT('',(0.,0.,54.));
#37433=CARTESIAN_POINT('',(0.,0.,54.));
#37434=CARTESIAN_POINT('',(0.,0.,30.));
#37435=CARTESIAN_POINT('Origin',(4.44089209850063E-15,0.,42.));
#37436=CARTESIAN_POINT('',(0.,0.,20.));
#37437=CARTESIAN_POINT('',(9.79717439317883E-16,0.,34.));
#37438=CARTESIAN_POINT('Origin',(0.,0.,42.));
#37439=CARTESIAN_POINT('Origin',(55.,0.,36.0323593997502));
#37440=CARTESIAN_POINT('',(60.,10.,36.0323593997502));
#37441=CARTESIAN_POINT('',(56.1361480780321,10.,40.9015654484592));
#37442=CARTESIAN_POINT('Origin',(55.,10.,36.0323593997502));
#37443=CARTESIAN_POINT('',(56.1361480780321,0.,40.9015654484592));
#37444=CARTESIAN_POINT('',(60.,0.,36.0323593997502));
#37445=CARTESIAN_POINT('Origin',(0.,0.,54.));
#37446=CARTESIAN_POINT('',(0.,10.,54.));
#37447=CARTESIAN_POINT('',(0.,10.,54.));
#37448=CARTESIAN_POINT('',(0.,0.,54.));
#37449=CARTESIAN_POINT('Origin',(0.,5.,42.));
#37450=CARTESIAN_POINT('',(9.79717439317883E-16,10.,34.));
#37451=CARTESIAN_POINT('Origin',(0.,10.,42.));
#37452=CARTESIAN_POINT('',(9.79717439317883E-16,5.,34.));
#37453=CARTESIAN_POINT('Origin',(60.,0.,40.));
#37454=CARTESIAN_POINT('',(60.,10.,40.));
#37455=CARTESIAN_POINT('Origin',(4.44089209850063E-15,0.,42.));
#37456=CARTESIAN_POINT('',(0.,10.,30.));
#37457=CARTESIAN_POINT('Origin',(4.44089209850063E-15,10.,42.));
#37458=CARTESIAN_POINT('',(0.,0.,30.));
#37459=CARTESIAN_POINT('Origin',(0.,0.,20.));
#37460=CARTESIAN_POINT('',(0.,10.,20.));
#37461=CARTESIAN_POINT('Origin',(24.,10.,37.));
#37462=CARTESIAN_POINT('',(0.,0.,0.));
#37463=CARTESIAN_POINT('Origin',(60.,3.,30.));
#37464=CARTESIAN_POINT('',(60.,3.,30.));
#37465=CARTESIAN_POINT('',(30.,3.,30.));
#37466=CARTESIAN_POINT('',(60.,3.,30.));
#37467=CARTESIAN_POINT('',(30.,3.,40.));
#37468=CARTESIAN_POINT('',(30.,3.,30.));
#37469=CARTESIAN_POINT('',(60.,3.,40.));
#37470=CARTESIAN_POINT('',(60.,3.,40.));
#37471=CARTESIAN_POINT('',(60.,3.,30.));
#37472=CARTESIAN_POINT('Origin',(60.,-3.,30.));
#37473=CARTESIAN_POINT('',(60.,-3.,30.));
#37474=CARTESIAN_POINT('',(60.,-3.,30.));
#37475=CARTESIAN_POINT('',(60.,-3.,40.));
#37476=CARTESIAN_POINT('',(60.,-3.,40.));
#37477=CARTESIAN_POINT('',(60.,-3.,30.));
#37478=CARTESIAN_POINT('Origin',(30.,-3.,30.));
#37479=CARTESIAN_POINT('',(30.,-3.,30.));
#37480=CARTESIAN_POINT('',(30.,-3.,30.));
#37481=CARTESIAN_POINT('',(30.,-3.,40.));
#37482=CARTESIAN_POINT('',(30.,-3.,40.));
#37483=CARTESIAN_POINT('',(30.,-3.,30.));
#37484=CARTESIAN_POINT('Origin',(30.,3.,30.));
#37485=CARTESIAN_POINT('',(30.,3.,30.));
#37486=CARTESIAN_POINT('',(30.,3.,40.));
#37487=CARTESIAN_POINT('Origin',(45.,0.,40.));
#37488=CARTESIAN_POINT('Origin',(45.,0.,30.));
#37489=CARTESIAN_POINT('',(0.,0.,0.));
#37490=CARTESIAN_POINT('Origin',(0.,0.,0.));
#37491=CARTESIAN_POINT('',(-6.,-7.34788079488412E-16,0.));
#37492=CARTESIAN_POINT('Origin',(0.,0.,0.));
#37493=CARTESIAN_POINT('',(-6.,-7.34788079488412E-16,10.));
#37494=CARTESIAN_POINT('',(-6.,-7.34788079488412E-16,0.));
#37495=CARTESIAN_POINT('Origin',(0.,0.,10.));
#37496=CARTESIAN_POINT('Origin',(0.,0.,0.));
#37497=CARTESIAN_POINT('',(-8.,-9.79717439317883E-16,10.));
#37498=CARTESIAN_POINT('Origin',(0.,0.,10.));
#37499=CARTESIAN_POINT('',(-8.,-9.79717439317883E-16,0.));
#37500=CARTESIAN_POINT('',(-8.,-9.79717439317883E-16,0.));
#37501=CARTESIAN_POINT('Origin',(0.,0.,0.));
#37502=CARTESIAN_POINT('Origin',(0.,0.,10.));
#37503=CARTESIAN_POINT('Origin',(0.,0.,0.));
#37504=CARTESIAN_POINT('',(0.,0.,0.));
#37505=CARTESIAN_POINT('Origin',(70.,10.,10.));
#37506=CARTESIAN_POINT('',(70.,10.,10.));
#37507=CARTESIAN_POINT('',(50.,10.,10.));
#37508=CARTESIAN_POINT('',(70.,10.,10.));
#37509=CARTESIAN_POINT('',(50.,10.,30.));
#37510=CARTESIAN_POINT('',(50.,10.,10.));
#37511=CARTESIAN_POINT('',(70.,10.,30.));
#37512=CARTESIAN_POINT('',(70.,10.,30.));
#37513=CARTESIAN_POINT('',(70.,10.,10.));
#37514=CARTESIAN_POINT('Origin',(70.,-10.,10.));
#37515=CARTESIAN_POINT('',(70.,-10.,10.));
#37516=CARTESIAN_POINT('',(70.,-10.,10.));
#37517=CARTESIAN_POINT('',(70.,-10.,30.));
#37518=CARTESIAN_POINT('',(70.,-10.,30.));
#37519=CARTESIAN_POINT('',(70.,-10.,10.));
#37520=CARTESIAN_POINT('Origin',(50.,-10.,10.));
#37521=CARTESIAN_POINT('',(50.,-10.,10.));
#37522=CARTESIAN_POINT('',(50.,-10.,10.));
#37523=CARTESIAN_POINT('',(50.,-10.,30.));
#37524=CARTESIAN_POINT('',(50.,-10.,30.));
#37525=CARTESIAN_POINT('',(50.,-10.,10.));
#37526=CARTESIAN_POINT('Origin',(50.,10.,10.));
#37527=CARTESIAN_POINT('',(50.,10.,10.));
#37528=CARTESIAN_POINT('',(50.,10.,30.));
#37529=CARTESIAN_POINT('Origin',(60.,0.,30.));
#37530=CARTESIAN_POINT('Origin',(60.,0.,10.));
#37531=CARTESIAN_POINT('',(0.,0.,0.));
#37532=CARTESIAN_POINT('Origin',(0.,0.,0.));
#37533=CARTESIAN_POINT('',(-8.,-9.79717439317883E-16,120.));
#37534=CARTESIAN_POINT('Origin',(0.,0.,120.));
#37535=CARTESIAN_POINT('',(-8.,-9.79717439317883E-16,0.));
#37536=CARTESIAN_POINT('',(-8.,-9.79717439317883E-16,0.));
#37537=CARTESIAN_POINT('Origin',(0.,0.,0.));
#37538=CARTESIAN_POINT('Origin',(0.,0.,120.));
#37539=CARTESIAN_POINT('Origin',(0.,0.,0.));
#37540=CARTESIAN_POINT('',(0.,0.,0.));
#37541=CARTESIAN_POINT('Origin',(0.,0.,80.));
#37542=CARTESIAN_POINT('',(-8.,-9.79717439317883E-16,80.));
#37543=CARTESIAN_POINT('Origin',(0.,0.,80.));
#37544=CARTESIAN_POINT('Origin',(0.,0.,82.));
#37545=CARTESIAN_POINT('',(-16.,1.95943487863577E-15,82.));
#37546=CARTESIAN_POINT('Origin',(0.,0.,82.));
#37547=CARTESIAN_POINT('Origin',(0.,0.,0.));
#37548=CARTESIAN_POINT('',(-8.,-9.79717439317883E-16,0.));
#37549=CARTESIAN_POINT('Origin',(0.,0.,0.));
#37550=CARTESIAN_POINT('',(-8.,-9.79717439317883E-16,0.));
#37551=CARTESIAN_POINT('Origin',(0.,0.,0.));
#37552=CARTESIAN_POINT('',(-16.,1.95943487863577E-15,0.));
#37553=CARTESIAN_POINT('',(-16.,-1.95943487863577E-15,0.));
#37554=CARTESIAN_POINT('Origin',(0.,0.,0.));
#37555=CARTESIAN_POINT('Origin',(0.,0.,0.));
#37556=CARTESIAN_POINT('',(0.,0.,0.));
#37557=CARTESIAN_POINT('Origin',(0.,0.,24.5));
#37558=CARTESIAN_POINT('',(-5.,-6.12323399573677E-16,25.));
#37559=CARTESIAN_POINT('Origin',(0.,0.,25.));
#37560=CARTESIAN_POINT('',(-5.,-6.12323399573677E-16,24.));
#37561=CARTESIAN_POINT('',(-5.,-6.12323399573677E-16,24.5));
#37562=CARTESIAN_POINT('Origin',(0.,0.,24.));
#37563=CARTESIAN_POINT('Origin',(9.,0.,24.));
#37564=CARTESIAN_POINT('',(-6.,7.34788079488412E-16,24.));
#37565=CARTESIAN_POINT('Origin',(0.,0.,24.));
#37566=CARTESIAN_POINT('Origin',(5.,0.,25.));
#37567=CARTESIAN_POINT('',(-6.,-7.34788079488412E-16,25.));
#37568=CARTESIAN_POINT('Origin',(0.,0.,25.));
#37569=CARTESIAN_POINT('Origin',(0.,0.,0.));
#37570=CARTESIAN_POINT('',(-6.,-7.34788079488412E-16,26.));
#37571=CARTESIAN_POINT('Origin',(0.,0.,26.));
#37572=CARTESIAN_POINT('',(-6.,-7.34788079488412E-16,0.));
#37573=CARTESIAN_POINT('Origin',(0.,0.,0.));
#37574=CARTESIAN_POINT('',(-9.,-1.10218211923262E-15,0.));
#37575=CARTESIAN_POINT('Origin',(0.,0.,0.));
#37576=CARTESIAN_POINT('',(-6.,-7.34788079488412E-16,0.));
#37577=CARTESIAN_POINT('Origin',(0.,0.,0.));
#37578=CARTESIAN_POINT('Origin',(0.,0.,-4.));
#37579=CARTESIAN_POINT('',(-9.,-1.10218211923262E-15,-4.));
#37580=CARTESIAN_POINT('',(-9.,-1.10218211923262E-15,-4.));
#37581=CARTESIAN_POINT('Origin',(0.,0.,-4.));
#37582=CARTESIAN_POINT('Origin',(0.,0.,-4.));
#37583=CARTESIAN_POINT('Origin',(0.,0.,0.));
#37584=CARTESIAN_POINT('',(-6.,-7.34788079488412E-16,0.));
#37585=CARTESIAN_POINT('Origin',(0.,0.,26.));
#37586=CARTESIAN_POINT('',(0.,0.,0.));
#37587=CARTESIAN_POINT('Origin',(0.,0.,0.));
#37588=CARTESIAN_POINT('',(-6.,-7.34788079488412E-16,0.));
#37589=CARTESIAN_POINT('Origin',(0.,0.,0.));
#37590=CARTESIAN_POINT('',(-6.,-7.34788079488412E-16,2.));
#37591=CARTESIAN_POINT('',(-6.,-7.34788079488412E-16,0.));
#37592=CARTESIAN_POINT('Origin',(0.,0.,2.));
#37593=CARTESIAN_POINT('Origin',(0.,0.,0.));
#37594=CARTESIAN_POINT('',(-11.,-1.34711147906209E-15,2.));
#37595=CARTESIAN_POINT('Origin',(0.,0.,2.));
#37596=CARTESIAN_POINT('',(-11.,-1.34711147906209E-15,0.));
#37597=CARTESIAN_POINT('',(-11.,-1.34711147906209E-15,0.));
#37598=CARTESIAN_POINT('Origin',(0.,0.,0.));
#37599=CARTESIAN_POINT('Origin',(0.,0.,2.));
#37600=CARTESIAN_POINT('Origin',(0.,0.,0.));
#37601=CARTESIAN_POINT('',(0.,0.,0.));
#37602=CARTESIAN_POINT('Origin',(-1.,0.,1.));
#37603=CARTESIAN_POINT('',(-1.,4.89897948556636,0.));
#37604=CARTESIAN_POINT('',(-1.,4.89897948556636,1.));
#37605=CARTESIAN_POINT('',(-1.,4.89897948556636,0.));
#37606=CARTESIAN_POINT('',(-1.,8.94427190999916,0.));
#37607=CARTESIAN_POINT('',(-1.,0.,0.));
#37608=CARTESIAN_POINT('',(-1.,8.94427190999916,1.));
#37609=CARTESIAN_POINT('',(-1.,8.94427190999916,0.));
#37610=CARTESIAN_POINT('',(-1.,0.,1.));
#37611=CARTESIAN_POINT('Origin',(1.,18.,1.));
#37612=CARTESIAN_POINT('',(1.,4.89897948556636,1.));
#37613=CARTESIAN_POINT('',(1.,4.89897948556636,0.));
#37614=CARTESIAN_POINT('',(1.,4.89897948556636,0.));
#37615=CARTESIAN_POINT('',(1.,8.94427190999916,1.));
#37616=CARTESIAN_POINT('',(1.,9.,1.));
#37617=CARTESIAN_POINT('',(1.,8.94427190999916,0.));
#37618=CARTESIAN_POINT('',(1.,8.94427190999916,0.));
#37619=CARTESIAN_POINT('',(1.,9.,0.));
#37620=CARTESIAN_POINT('Origin',(0.,0.,0.));
#37621=CARTESIAN_POINT('Origin',(0.,0.,0.));
#37622=CARTESIAN_POINT('Origin',(0.,0.,0.));
#37623=CARTESIAN_POINT('Origin',(0.,0.,0.));
#37624=CARTESIAN_POINT('Origin',(0.,0.,1.));
#37625=CARTESIAN_POINT('Origin',(0.,0.,0.));
#37626=CARTESIAN_POINT('Origin',(0.,0.,1.));
#37627=CARTESIAN_POINT('Origin',(0.,0.,1.));
#37628=CARTESIAN_POINT('',(0.,0.,0.));
#37629=CARTESIAN_POINT('',(0.,-40.,0.));
#37630=CARTESIAN_POINT('',(0.,0.,0.));
#37631=CARTESIAN_POINT('',(0.,-126.,0.));
#37632=CARTESIAN_POINT('',(0.,-100.,0.));
#37633=CARTESIAN_POINT('',(-60.,-75.,10.));
#37634=CARTESIAN_POINT('',(-60.,-75.,62.));
#37635=CARTESIAN_POINT('',(-60.,-75.,64.));
#37636=CARTESIAN_POINT('',(0.,0.,0.));
#37637=CARTESIAN_POINT('',(0.,-116.,0.));
#37638=CARTESIAN_POINT('',(0.,-103.,0.));
#37639=CARTESIAN_POINT('',(0.,-116.,42.));
#37640=CARTESIAN_POINT('',(0.,-60.,0.));
#37641=CARTESIAN_POINT('',(70.,-60.,20.));
#37642=CARTESIAN_POINT('',(110.,-60.,20.));
#37643=CARTESIAN_POINT('',(0.,-128.,42.));
#37644=CARTESIAN_POINT('',(0.,-128.,42.));
#37645=CARTESIAN_POINT('',(0.,-104.,42.));
#37646=CARTESIAN_POINT('',(0.,40.,0.));
#37647=CARTESIAN_POINT('',(0.,116.,0.));
#37648=CARTESIAN_POINT('',(-60.,75.,10.));
#37649=CARTESIAN_POINT('',(-60.,75.,62.));
#37650=CARTESIAN_POINT('',(-60.,75.,64.));
#37651=CARTESIAN_POINT('',(0.,106.,0.));
#37652=CARTESIAN_POINT('',(0.,103.,0.));
#37653=CARTESIAN_POINT('',(0.,106.,42.));
#37654=CARTESIAN_POINT('',(0.,60.,0.));
#37655=CARTESIAN_POINT('',(70.,60.,20.));
#37656=CARTESIAN_POINT('',(110.,60.,20.));
#37657=CARTESIAN_POINT('',(0.,-106.,42.));
#37658=CARTESIAN_POINT('',(0.,128.,42.));
#37659=CARTESIAN_POINT('',(0.,128.,42.));
#37660=CARTESIAN_POINT('',(0.,106.,42.));
#37661=CARTESIAN_POINT('',(0.,104.,42.));
#37662=UNCERTAINTY_MEASURE_WITH_UNIT(LENGTH_MEASURE(0.01),#37702,
'DISTANCE_ACCURACY_VALUE',
'Maximum model space distance between geometric entities at asserted c
onnectivities');
#37663=UNCERTAINTY_MEASURE_WITH_UNIT(LENGTH_MEASURE(0.01),#37702,
'DISTANCE_ACCURACY_VALUE',
'Maximum model space distance between geometric entities at asserted c
onnectivities');
#37664=UNCERTAINTY_MEASURE_WITH_UNIT(LENGTH_MEASURE(0.01),#37702,
'DISTANCE_ACCURACY_VALUE',
'Maximum model space distance between geometric entities at asserted c
onnectivities');
#37665=UNCERTAINTY_MEASURE_WITH_UNIT(LENGTH_MEASURE(0.01),#37702,
'DISTANCE_ACCURACY_VALUE',
'Maximum model space distance between geometric entities at asserted c
onnectivities');
#37666=UNCERTAINTY_MEASURE_WITH_UNIT(LENGTH_MEASURE(0.01),#37702,
'DISTANCE_ACCURACY_VALUE',
'Maximum model space distance between geometric entities at asserted c
onnectivities');
#37667=UNCERTAINTY_MEASURE_WITH_UNIT(LENGTH_MEASURE(0.01),#37702,
'DISTANCE_ACCURACY_VALUE',
'Maximum model space distance between geometric entities at asserted c
onnectivities');
#37668=UNCERTAINTY_MEASURE_WITH_UNIT(LENGTH_MEASURE(0.01),#37702,
'DISTANCE_ACCURACY_VALUE',
'Maximum model space distance between geometric entities at asserted c
onnectivities');
#37669=UNCERTAINTY_MEASURE_WITH_UNIT(LENGTH_MEASURE(0.01),#37702,
'DISTANCE_ACCURACY_VALUE',
'Maximum model space distance between geometric entities at asserted c
onnectivities');
#37670=UNCERTAINTY_MEASURE_WITH_UNIT(LENGTH_MEASURE(0.01),#37702,
'DISTANCE_ACCURACY_VALUE',
'Maximum model space distance between geometric entities at asserted c
onnectivities');
#37671=UNCERTAINTY_MEASURE_WITH_UNIT(LENGTH_MEASURE(0.01),#37702,
'DISTANCE_ACCURACY_VALUE',
'Maximum model space distance between geometric entities at asserted c
onnectivities');
#37672=UNCERTAINTY_MEASURE_WITH_UNIT(LENGTH_MEASURE(0.01),#37702,
'DISTANCE_ACCURACY_VALUE',
'Maximum model space distance between geometric entities at asserted c
onnectivities');
#37673=UNCERTAINTY_MEASURE_WITH_UNIT(LENGTH_MEASURE(0.01),#37702,
'DISTANCE_ACCURACY_VALUE',
'Maximum model space distance between geometric entities at asserted c
onnectivities');
#37674=UNCERTAINTY_MEASURE_WITH_UNIT(LENGTH_MEASURE(0.01),#37702,
'DISTANCE_ACCURACY_VALUE',
'Maximum model space distance between geometric entities at asserted c
onnectivities');
#37675=UNCERTAINTY_MEASURE_WITH_UNIT(LENGTH_MEASURE(0.01),#37702,
'DISTANCE_ACCURACY_VALUE',
'Maximum model space distance between geometric entities at asserted c
onnectivities');
#37676=UNCERTAINTY_MEASURE_WITH_UNIT(LENGTH_MEASURE(0.01),#37702,
'DISTANCE_ACCURACY_VALUE',
'Maximum model space distance between geometric entities at asserted c
onnectivities');
#37677=UNCERTAINTY_MEASURE_WITH_UNIT(LENGTH_MEASURE(0.01),#37702,
'DISTANCE_ACCURACY_VALUE',
'Maximum model space distance between geometric entities at asserted c
onnectivities');
#37678=UNCERTAINTY_MEASURE_WITH_UNIT(LENGTH_MEASURE(0.01),#37702,
'DISTANCE_ACCURACY_VALUE',
'Maximum model space distance between geometric entities at asserted c
onnectivities');
#37679=UNCERTAINTY_MEASURE_WITH_UNIT(LENGTH_MEASURE(0.01),#37702,
'DISTANCE_ACCURACY_VALUE',
'Maximum model space distance between geometric entities at asserted c
onnectivities');
#37680=UNCERTAINTY_MEASURE_WITH_UNIT(LENGTH_MEASURE(0.01),#37702,
'DISTANCE_ACCURACY_VALUE',
'Maximum model space distance between geometric entities at asserted c
onnectivities');
#37681=UNCERTAINTY_MEASURE_WITH_UNIT(LENGTH_MEASURE(0.01),#37702,
'DISTANCE_ACCURACY_VALUE',
'Maximum model space distance between geometric entities at asserted c
onnectivities');
#37682=(
GEOMETRIC_REPRESENTATION_CONTEXT(3)
GLOBAL_UNCERTAINTY_ASSIGNED_CONTEXT((#37662))
GLOBAL_UNIT_ASSIGNED_CONTEXT((#37702,#37704,#37705))
REPRESENTATION_CONTEXT('','3D')
);
#37683=(
GEOMETRIC_REPRESENTATION_CONTEXT(3)
GLOBAL_UNCERTAINTY_ASSIGNED_CONTEXT((#37663))
GLOBAL_UNIT_ASSIGNED_CONTEXT((#37702,#37704,#37705))
REPRESENTATION_CONTEXT('','3D')
);
#37684=(
GEOMETRIC_REPRESENTATION_CONTEXT(3)
GLOBAL_UNCERTAINTY_ASSIGNED_CONTEXT((#37664))
GLOBAL_UNIT_ASSIGNED_CONTEXT((#37702,#37704,#37705))
REPRESENTATION_CONTEXT('','3D')
);
#37685=(
GEOMETRIC_REPRESENTATION_CONTEXT(3)
GLOBAL_UNCERTAINTY_ASSIGNED_CONTEXT((#37665))
GLOBAL_UNIT_ASSIGNED_CONTEXT((#37702,#37704,#37705))
REPRESENTATION_CONTEXT('','3D')
);
#37686=(
GEOMETRIC_REPRESENTATION_CONTEXT(3)
GLOBAL_UNCERTAINTY_ASSIGNED_CONTEXT((#37666))
GLOBAL_UNIT_ASSIGNED_CONTEXT((#37702,#37704,#37705))
REPRESENTATION_CONTEXT('','3D')
);
#37687=(
GEOMETRIC_REPRESENTATION_CONTEXT(3)
GLOBAL_UNCERTAINTY_ASSIGNED_CONTEXT((#37667))
GLOBAL_UNIT_ASSIGNED_CONTEXT((#37702,#37704,#37705))
REPRESENTATION_CONTEXT('','3D')
);
#37688=(
GEOMETRIC_REPRESENTATION_CONTEXT(3)
GLOBAL_UNCERTAINTY_ASSIGNED_CONTEXT((#37668))
GLOBAL_UNIT_ASSIGNED_CONTEXT((#37702,#37704,#37705))
REPRESENTATION_CONTEXT('','3D')
);
#37689=(
GEOMETRIC_REPRESENTATION_CONTEXT(3)
GLOBAL_UNCERTAINTY_ASSIGNED_CONTEXT((#37669))
GLOBAL_UNIT_ASSIGNED_CONTEXT((#37702,#37704,#37705))
REPRESENTATION_CONTEXT('','3D')
);
#37690=(
GEOMETRIC_REPRESENTATION_CONTEXT(3)
GLOBAL_UNCERTAINTY_ASSIGNED_CONTEXT((#37670))
GLOBAL_UNIT_ASSIGNED_CONTEXT((#37702,#37704,#37705))
REPRESENTATION_CONTEXT('','3D')
);
#37691=(
GEOMETRIC_REPRESENTATION_CONTEXT(3)
GLOBAL_UNCERTAINTY_ASSIGNED_CONTEXT((#37671))
GLOBAL_UNIT_ASSIGNED_CONTEXT((#37702,#37704,#37705))
REPRESENTATION_CONTEXT('','3D')
);
#37692=(
GEOMETRIC_REPRESENTATION_CONTEXT(3)
GLOBAL_UNCERTAINTY_ASSIGNED_CONTEXT((#37672))
GLOBAL_UNIT_ASSIGNED_CONTEXT((#37702,#37704,#37705))
REPRESENTATION_CONTEXT('','3D')
);
#37693=(
GEOMETRIC_REPRESENTATION_CONTEXT(3)
GLOBAL_UNCERTAINTY_ASSIGNED_CONTEXT((#37673))
GLOBAL_UNIT_ASSIGNED_CONTEXT((#37702,#37704,#37705))
REPRESENTATION_CONTEXT('','3D')
);
#37694=(
GEOMETRIC_REPRESENTATION_CONTEXT(3)
GLOBAL_UNCERTAINTY_ASSIGNED_CONTEXT((#37674))
GLOBAL_UNIT_ASSIGNED_CONTEXT((#37702,#37704,#37705))
REPRESENTATION_CONTEXT('','3D')
);
#37695=(
GEOMETRIC_REPRESENTATION_CONTEXT(3)
GLOBAL_UNCERTAINTY_ASSIGNED_CONTEXT((#37675))
GLOBAL_UNIT_ASSIGNED_CONTEXT((#37702,#37704,#37705))
REPRESENTATION_CONTEXT('','3D')
);
#37696=(
GEOMETRIC_REPRESENTATION_CONTEXT(3)
GLOBAL_UNCERTAINTY_ASSIGNED_CONTEXT((#37676))
GLOBAL_UNIT_ASSIGNED_CONTEXT((#37702,#37704,#37705))
REPRESENTATION_CONTEXT('','3D')
);
#37697=(
GEOMETRIC_REPRESENTATION_CONTEXT(3)
GLOBAL_UNCERTAINTY_ASSIGNED_CONTEXT((#37677))
GLOBAL_UNIT_ASSIGNED_CONTEXT((#37702,#37704,#37705))
REPRESENTATION_CONTEXT('','3D')
);
#37698=(
GEOMETRIC_REPRESENTATION_CONTEXT(3)
GLOBAL_UNCERTAINTY_ASSIGNED_CONTEXT((#37678))
GLOBAL_UNIT_ASSIGNED_CONTEXT((#37702,#37704,#37705))
REPRESENTATION_CONTEXT('','3D')
);
#37699=(
GEOMETRIC_REPRESENTATION_CONTEXT(3)
GLOBAL_UNCERTAINTY_ASSIGNED_CONTEXT((#37679))
GLOBAL_UNIT_ASSIGNED_CONTEXT((#37702,#37704,#37705))
REPRESENTATION_CONTEXT('','3D')
);
#37700=(
GEOMETRIC_REPRESENTATION_CONTEXT(3)
GLOBAL_UNCERTAINTY_ASSIGNED_CONTEXT((#37680))
GLOBAL_UNIT_ASSIGNED_CONTEXT((#37702,#37704,#37705))
REPRESENTATION_CONTEXT('','3D')
);
#37701=(
GEOMETRIC_REPRESENTATION_CONTEXT(3)
GLOBAL_UNCERTAINTY_ASSIGNED_CONTEXT((#37681))
GLOBAL_UNIT_ASSIGNED_CONTEXT((#37702,#37704,#37705))
REPRESENTATION_CONTEXT('','3D')
);
#37702=(
LENGTH_UNIT()
NAMED_UNIT(*)
SI_UNIT(.MILLI.,.METRE.)
);
#37703=(
LENGTH_UNIT()
NAMED_UNIT(*)
SI_UNIT($,.METRE.)
);
#37704=(
NAMED_UNIT(*)
PLANE_ANGLE_UNIT()
SI_UNIT($,.RADIAN.)
);
#37705=(
NAMED_UNIT(*)
SI_UNIT($,.STERADIAN.)
SOLID_ANGLE_UNIT()
);
#37706=SHAPE_DEFINITION_REPRESENTATION(#37725,#37778);
#37707=SHAPE_DEFINITION_REPRESENTATION(#37726,#37779);
#37708=SHAPE_DEFINITION_REPRESENTATION(#37727,#37780);
#37709=SHAPE_DEFINITION_REPRESENTATION(#37728,#37781);
#37710=SHAPE_DEFINITION_REPRESENTATION(#37729,#37782);
#37711=SHAPE_DEFINITION_REPRESENTATION(#37730,#37783);
#37712=SHAPE_DEFINITION_REPRESENTATION(#37731,#37784);
#37713=SHAPE_DEFINITION_REPRESENTATION(#37732,#37785);
#37714=SHAPE_DEFINITION_REPRESENTATION(#37733,#37786);
#37715=SHAPE_DEFINITION_REPRESENTATION(#37734,#37787);
#37716=SHAPE_DEFINITION_REPRESENTATION(#37735,#37788);
#37717=SHAPE_DEFINITION_REPRESENTATION(#37736,#37789);
#37718=SHAPE_DEFINITION_REPRESENTATION(#37737,#37790);
#37719=SHAPE_DEFINITION_REPRESENTATION(#37738,#37791);
#37720=SHAPE_DEFINITION_REPRESENTATION(#37739,#37792);
#37721=SHAPE_DEFINITION_REPRESENTATION(#37740,#37793);
#37722=SHAPE_DEFINITION_REPRESENTATION(#37741,#37794);
#37723=SHAPE_DEFINITION_REPRESENTATION(#37742,#37795);
#37724=SHAPE_DEFINITION_REPRESENTATION(#37743,#37796);
#37725=PRODUCT_DEFINITION_SHAPE('',$,#37798);
#37726=PRODUCT_DEFINITION_SHAPE('',$,#37799);
#37727=PRODUCT_DEFINITION_SHAPE('',$,#37800);
#37728=PRODUCT_DEFINITION_SHAPE('',$,#37801);
#37729=PRODUCT_DEFINITION_SHAPE('',$,#37802);
#37730=PRODUCT_DEFINITION_SHAPE('',$,#37803);
#37731=PRODUCT_DEFINITION_SHAPE('',$,#37804);
#37732=PRODUCT_DEFINITION_SHAPE('',$,#37805);
#37733=PRODUCT_DEFINITION_SHAPE('',$,#37806);
#37734=PRODUCT_DEFINITION_SHAPE('',$,#37807);
#37735=PRODUCT_DEFINITION_SHAPE('',$,#37808);
#37736=PRODUCT_DEFINITION_SHAPE('',$,#37809);
#37737=PRODUCT_DEFINITION_SHAPE('',$,#37810);
#37738=PRODUCT_DEFINITION_SHAPE('',$,#37811);
#37739=PRODUCT_DEFINITION_SHAPE('',$,#37812);
#37740=PRODUCT_DEFINITION_SHAPE('',$,#37813);
#37741=PRODUCT_DEFINITION_SHAPE('',$,#37814);
#37742=PRODUCT_DEFINITION_SHAPE('',$,#37815);
#37743=PRODUCT_DEFINITION_SHAPE('',$,#37816);
#37744=PRODUCT_DEFINITION_SHAPE($,$,#113);
#37745=PRODUCT_DEFINITION_SHAPE($,$,#114);
#37746=PRODUCT_DEFINITION_SHAPE($,$,#115);
#37747=PRODUCT_DEFINITION_SHAPE($,$,#116);
#37748=PRODUCT_DEFINITION_SHAPE($,$,#117);
#37749=PRODUCT_DEFINITION_SHAPE($,$,#118);
#37750=PRODUCT_DEFINITION_SHAPE($,$,#119);
#37751=PRODUCT_DEFINITION_SHAPE($,$,#120);
#37752=PRODUCT_DEFINITION_SHAPE($,$,#121);
#37753=PRODUCT_DEFINITION_SHAPE($,$,#122);
#37754=PRODUCT_DEFINITION_SHAPE($,$,#123);
#37755=PRODUCT_DEFINITION_SHAPE($,$,#124);
#37756=PRODUCT_DEFINITION_SHAPE($,$,#125);
#37757=PRODUCT_DEFINITION_SHAPE($,$,#126);
#37758=PRODUCT_DEFINITION_SHAPE($,$,#127);
#37759=PRODUCT_DEFINITION_SHAPE($,$,#128);
#37760=PRODUCT_DEFINITION_SHAPE($,$,#129);
#37761=PRODUCT_DEFINITION_SHAPE($,$,#130);
#37762=PRODUCT_DEFINITION_SHAPE($,$,#131);
#37763=PRODUCT_DEFINITION_SHAPE($,$,#132);
#37764=PRODUCT_DEFINITION_SHAPE($,$,#133);
#37765=PRODUCT_DEFINITION_SHAPE($,$,#134);
#37766=PRODUCT_DEFINITION_SHAPE($,$,#135);
#37767=PRODUCT_DEFINITION_SHAPE($,$,#136);
#37768=PRODUCT_DEFINITION_SHAPE($,$,#137);
#37769=PRODUCT_DEFINITION_SHAPE($,$,#138);
#37770=PRODUCT_DEFINITION_SHAPE($,$,#139);
#37771=PRODUCT_DEFINITION_SHAPE($,$,#140);
#37772=PRODUCT_DEFINITION_SHAPE($,$,#141);
#37773=PRODUCT_DEFINITION_SHAPE($,$,#142);
#37774=PRODUCT_DEFINITION_SHAPE($,$,#143);
#37775=PRODUCT_DEFINITION_SHAPE($,$,#144);
#37776=PRODUCT_DEFINITION_SHAPE($,$,#145);
#37777=PRODUCT_DEFINITION_SHAPE($,$,#146);
#37778=SHAPE_REPRESENTATION('',(#4361,#4673,#4674,#4675,#4676,#4677,#4678,
#4679,#4680,#4681,#4682,#4683,#4684,#4685,#4686,#4687,#4688,#4689,#4690,
#4691,#4692,#4693,#4694,#4695,#4696,#4697,#4698,#4699,#4700,#4701,#4702,
#4703,#4704,#4705,#4706),#37682);
#37779=SHAPE_REPRESENTATION('',(#4362),#37683);
#37780=SHAPE_REPRESENTATION('',(#4393),#37684);
#37781=SHAPE_REPRESENTATION('',(#4406),#37685);
#37782=SHAPE_REPRESENTATION('',(#4419),#37686);
#37783=SHAPE_REPRESENTATION('',(#4434),#37687);
#37784=SHAPE_REPRESENTATION('',(#4441),#37688);
#37785=SHAPE_REPRESENTATION('',(#4454),#37689);
#37786=SHAPE_REPRESENTATION('',(#4488),#37690);
#37787=SHAPE_REPRESENTATION('',(#4497),#37691);
#37788=SHAPE_REPRESENTATION('',(#4577),#37692);
#37789=SHAPE_REPRESENTATION('',(#4596),#37693);
#37790=SHAPE_REPRESENTATION('',(#4603),#37694);
#37791=SHAPE_REPRESENTATION('',(#4612),#37695);
#37792=SHAPE_REPRESENTATION('',(#4619),#37696);
#37793=SHAPE_REPRESENTATION('',(#4625),#37697);
#37794=SHAPE_REPRESENTATION('',(#4635),#37698);
#37795=SHAPE_REPRESENTATION('',(#4653),#37699);
#37796=SHAPE_REPRESENTATION('',(#4662),#37700);
#37797=PRODUCT_DEFINITION_CONTEXT('part definition',#37856,'design');
#37798=PRODUCT_DEFINITION('TAS-011','TAS-011',#37817,#37797);
#37799=PRODUCT_DEFINITION('Base plate','Base plate',#37818,#37797);
#37800=PRODUCT_DEFINITION('Fixed bed','Fixed bed',#37819,#37797);
#37801=PRODUCT_DEFINITION('Clamping beam','Clamping beam',#37820,#37797);
#37802=PRODUCT_DEFINITION('Folding leaf','Folding leaf',#37821,#37797);
#37803=PRODUCT_DEFINITION('Bed support','Bed support',#37822,#37797);
#37804=PRODUCT_DEFINITION('Fixed hinge cheek','Fixed hinge cheek',#37823,
#37797);
#37805=PRODUCT_DEFINITION('Threaded clamp boss','Threaded clamp boss',#37824,
#37797);
#37806=PRODUCT_DEFINITION('Flat washer M12','Flat washer M12',#37825,#37797);
#37807=PRODUCT_DEFINITION('Socket head cap screw M12x50',
'Socket head cap screw M12x50',#37826,#37797);
#37808=PRODUCT_DEFINITION('Moving hinge arm','Moving hinge arm',#37827,
#37797);
#37809=PRODUCT_DEFINITION('Leaf bridge block','Leaf bridge block',#37828,
#37797);
#37810=PRODUCT_DEFINITION('Hinge bushing','Hinge bushing',#37829,#37797);
#37811=PRODUCT_DEFINITION('Handle mounting block',
'Handle mounting block',#37830,#37797);
#37812=PRODUCT_DEFINITION('Handle rod','Handle rod',#37831,#37797);
#37813=PRODUCT_DEFINITION('Handle Grip','Handle grip',#37832,#37797);
#37814=PRODUCT_DEFINITION('Hinge pin','Hinge pin',#37833,#37797);
#37815=PRODUCT_DEFINITION('Hinge thrust washer','Hinge thrust washer',#37834,
#37797);
#37816=PRODUCT_DEFINITION('Hinge retaining ring','Hinge retaining ring',
#37835,#37797);
#37817=PRODUCT_DEFINITION_FORMATION('',$,#37858);
#37818=PRODUCT_DEFINITION_FORMATION('',$,#37859);
#37819=PRODUCT_DEFINITION_FORMATION('',$,#37860);
#37820=PRODUCT_DEFINITION_FORMATION('',$,#37861);
#37821=PRODUCT_DEFINITION_FORMATION('',$,#37862);
#37822=PRODUCT_DEFINITION_FORMATION('',$,#37863);
#37823=PRODUCT_DEFINITION_FORMATION('',$,#37864);
#37824=PRODUCT_DEFINITION_FORMATION('',$,#37865);
#37825=PRODUCT_DEFINITION_FORMATION('',$,#37866);
#37826=PRODUCT_DEFINITION_FORMATION('',$,#37867);
#37827=PRODUCT_DEFINITION_FORMATION('',$,#37868);
#37828=PRODUCT_DEFINITION_FORMATION('',$,#37869);
#37829=PRODUCT_DEFINITION_FORMATION('',$,#37870);
#37830=PRODUCT_DEFINITION_FORMATION('',$,#37871);
#37831=PRODUCT_DEFINITION_FORMATION('',$,#37872);
#37832=PRODUCT_DEFINITION_FORMATION('',$,#37873);
#37833=PRODUCT_DEFINITION_FORMATION('',$,#37874);
#37834=PRODUCT_DEFINITION_FORMATION('',$,#37875);
#37835=PRODUCT_DEFINITION_FORMATION('',$,#37876);
#37836=PRODUCT_RELATED_PRODUCT_CATEGORY('TAS-011','TAS-011',(#37858));
#37837=PRODUCT_RELATED_PRODUCT_CATEGORY('Base plate','Base plate',(#37859));
#37838=PRODUCT_RELATED_PRODUCT_CATEGORY('Fixed bed','Fixed bed',(#37860));
#37839=PRODUCT_RELATED_PRODUCT_CATEGORY('Clamping beam','Clamping beam',
(#37861));
#37840=PRODUCT_RELATED_PRODUCT_CATEGORY('Folding leaf','Folding leaf',(#37862));
#37841=PRODUCT_RELATED_PRODUCT_CATEGORY('Bed support','Bed support',(#37863));
#37842=PRODUCT_RELATED_PRODUCT_CATEGORY('Fixed hinge cheek',
'Fixed hinge cheek',(#37864));
#37843=PRODUCT_RELATED_PRODUCT_CATEGORY('Threaded clamp boss',
'Threaded clamp boss',(#37865));
#37844=PRODUCT_RELATED_PRODUCT_CATEGORY('Flat washer M12',
'Flat washer M12',(#37866));
#37845=PRODUCT_RELATED_PRODUCT_CATEGORY('Socket head cap screw M12x50',
'Socket head cap screw M12x50',(#37867));
#37846=PRODUCT_RELATED_PRODUCT_CATEGORY('Moving hinge arm',
'Moving hinge arm',(#37868));
#37847=PRODUCT_RELATED_PRODUCT_CATEGORY('Leaf bridge block',
'Leaf bridge block',(#37869));
#37848=PRODUCT_RELATED_PRODUCT_CATEGORY('Hinge bushing','Hinge bushing',
(#37870));
#37849=PRODUCT_RELATED_PRODUCT_CATEGORY('Handle mounting block',
'Handle mounting block',(#37871));
#37850=PRODUCT_RELATED_PRODUCT_CATEGORY('Handle rod','Handle rod',(#37872));
#37851=PRODUCT_RELATED_PRODUCT_CATEGORY('Handle grip','Handle grip',(#37873));
#37852=PRODUCT_RELATED_PRODUCT_CATEGORY('Hinge pin','Hinge pin',(#37874));
#37853=PRODUCT_RELATED_PRODUCT_CATEGORY('Hinge thrust washer',
'Hinge thrust washer',(#37875));
#37854=PRODUCT_RELATED_PRODUCT_CATEGORY('Hinge retaining ring',
'Hinge retaining ring',(#37876));
#37855=APPLICATION_PROTOCOL_DEFINITION('international standard',
'automotive_design',2009,#37856);
#37856=APPLICATION_CONTEXT(
'Core Data for Automotive Mechanical Design Process');
#37857=PRODUCT_CONTEXT('part definition',#37856,'mechanical');
#37858=PRODUCT('TAS-011','TAS-011',
'Independent manual bench leaf bending machine,200mm work width. Fabri
cated welded frame and folding leaf, repeated bushed and fully retaine
d hinge hardware, two handles with bonded grips, beveled clamping beam
 and modeledM12 clamp screws.2mm omitted-workpiece assembly reference 
gap, not a capacity claim. Native135deg hinge travel. Weld sizing, pro
duction fits, material condition, bending capacity, strength and life 
unassigned.',(#37857));
#37859=PRODUCT('Base plate','Base plate','Base plate',(#37857));
#37860=PRODUCT('Fixed bed','Fixed bed',$,(#37857));
#37861=PRODUCT('Clamping beam','Clamping beam',$,(#37857));
#37862=PRODUCT('Folding leaf','Folding leaf',$,(#37857));
#37863=PRODUCT('Bed support','Bed support',$,(#37857));
#37864=PRODUCT('Fixed hinge cheek','Fixed hinge cheek',$,(#37857));
#37865=PRODUCT('Threaded clamp boss','Threaded clamp boss',$,(#37857));
#37866=PRODUCT('Flat washer M12','Flat washer M12',$,(#37857));
#37867=PRODUCT('Socket head cap screw M12x50',
'Socket head cap screw M12x50',$,(#37857));
#37868=PRODUCT('Moving hinge arm','Moving hinge arm',$,(#37857));
#37869=PRODUCT('Leaf bridge block','Leaf bridge block',$,(#37857));
#37870=PRODUCT('Hinge bushing','Hinge bushing',$,(#37857));
#37871=PRODUCT('Handle mounting block','Handle mounting block',$,(#37857));
#37872=PRODUCT('Handle rod','Handle rod',$,(#37857));
#37873=PRODUCT('Handle Grip','Handle grip',$,(#37857));
#37874=PRODUCT('Hinge pin','Hinge pin','Hinge pin',(#37857));
#37875=PRODUCT('Hinge thrust washer','Hinge thrust washer',$,(#37857));
#37876=PRODUCT('Hinge retaining ring','Hinge retaining ring',$,(#37857));
#37877=PRESENTATION_STYLE_ASSIGNMENT((#37885));
#37878=PRESENTATION_STYLE_ASSIGNMENT((#37886));
#37879=PRESENTATION_STYLE_ASSIGNMENT((#37887));
#37880=PRESENTATION_STYLE_ASSIGNMENT((#37888));
#37881=PRESENTATION_STYLE_ASSIGNMENT((#37889));
#37882=PRESENTATION_STYLE_ASSIGNMENT((#37890));
#37883=PRESENTATION_STYLE_ASSIGNMENT((#37891));
#37884=PRESENTATION_STYLE_ASSIGNMENT((#37892));
#37885=SURFACE_STYLE_USAGE(.BOTH.,#37893);
#37886=SURFACE_STYLE_USAGE(.BOTH.,#37894);
#37887=SURFACE_STYLE_USAGE(.BOTH.,#37895);
#37888=SURFACE_STYLE_USAGE(.BOTH.,#37896);
#37889=SURFACE_STYLE_USAGE(.BOTH.,#37897);
#37890=SURFACE_STYLE_USAGE(.BOTH.,#37898);
#37891=SURFACE_STYLE_USAGE(.BOTH.,#37899);
#37892=SURFACE_STYLE_USAGE(.BOTH.,#37900);
#37893=SURFACE_SIDE_STYLE('',(#37901));
#37894=SURFACE_SIDE_STYLE('',(#37902));
#37895=SURFACE_SIDE_STYLE('',(#37903));
#37896=SURFACE_SIDE_STYLE('',(#37904));
#37897=SURFACE_SIDE_STYLE('',(#37905));
#37898=SURFACE_SIDE_STYLE('',(#37906));
#37899=SURFACE_SIDE_STYLE('',(#37907));
#37900=SURFACE_SIDE_STYLE('',(#37908));
#37901=SURFACE_STYLE_FILL_AREA(#37909);
#37902=SURFACE_STYLE_FILL_AREA(#37910);
#37903=SURFACE_STYLE_FILL_AREA(#37911);
#37904=SURFACE_STYLE_FILL_AREA(#37912);
#37905=SURFACE_STYLE_FILL_AREA(#37913);
#37906=SURFACE_STYLE_FILL_AREA(#37914);
#37907=SURFACE_STYLE_FILL_AREA(#37915);
#37908=SURFACE_STYLE_FILL_AREA(#37916);
#37909=FILL_AREA_STYLE('Steel - Satin',(#37917));
#37910=FILL_AREA_STYLE('Opaque(23,69,131)',(#37918));
#37911=FILL_AREA_STYLE('Opaque(104,114,127)',(#37919));
#37912=FILL_AREA_STYLE('Opaque(185,192,202)',(#37920));
#37913=FILL_AREA_STYLE('Opaque(81,175,227)',(#37921));
#37914=FILL_AREA_STYLE('Opaque(169,212,242)',(#37922));
#37915=FILL_AREA_STYLE('Opaque(64,72,82)',(#37923));
#37916=FILL_AREA_STYLE('Opaque(147,157,170)',(#37924));
#37917=FILL_AREA_STYLE_COLOUR('Steel - Satin',#37925);
#37918=FILL_AREA_STYLE_COLOUR('Opaque(23,69,131)',#37926);
#37919=FILL_AREA_STYLE_COLOUR('Opaque(104,114,127)',#37927);
#37920=FILL_AREA_STYLE_COLOUR('Opaque(185,192,202)',#37928);
#37921=FILL_AREA_STYLE_COLOUR('Opaque(81,175,227)',#37929);
#37922=FILL_AREA_STYLE_COLOUR('Opaque(169,212,242)',#37930);
#37923=FILL_AREA_STYLE_COLOUR('Opaque(64,72,82)',#37931);
#37924=FILL_AREA_STYLE_COLOUR('Opaque(147,157,170)',#37932);
#37925=COLOUR_RGB('Steel - Satin',0.627450980392157,0.627450980392157,0.627450980392157);
#37926=COLOUR_RGB('Opaque(23,69,131)',0.0901960784313725,0.270588235294118,
0.513725490196078);
#37927=COLOUR_RGB('Opaque(104,114,127)',0.407843137254902,0.447058823529412,
0.498039215686275);
#37928=COLOUR_RGB('Opaque(185,192,202)',0.725490196078431,0.752941176470588,
0.792156862745098);
#37929=COLOUR_RGB('Opaque(81,175,227)',0.317647058823529,0.686274509803922,
0.890196078431372);
#37930=COLOUR_RGB('Opaque(169,212,242)',0.662745098039216,0.831372549019608,
0.949019607843137);
#37931=COLOUR_RGB('Opaque(64,72,82)',0.250980392156863,0.282352941176471,
0.32156862745098);
#37932=COLOUR_RGB('Opaque(147,157,170)',0.576470588235294,0.615686274509804,
0.666666666666667);
ENDSEC;
END-ISO-10303-21;
